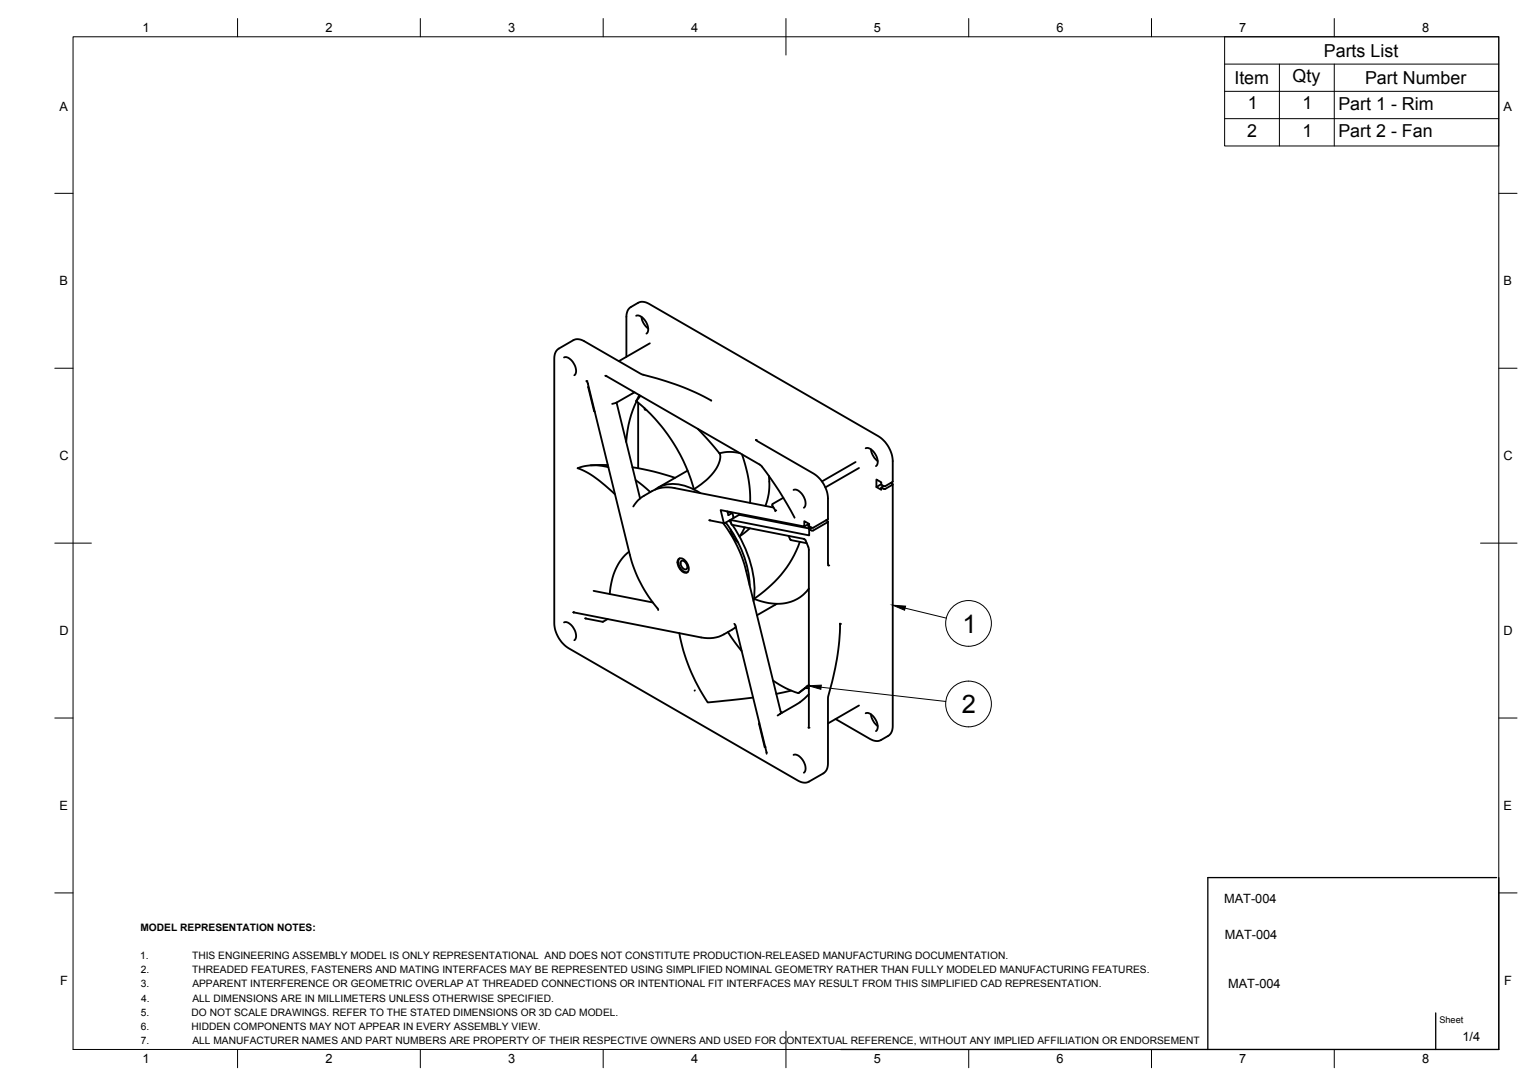
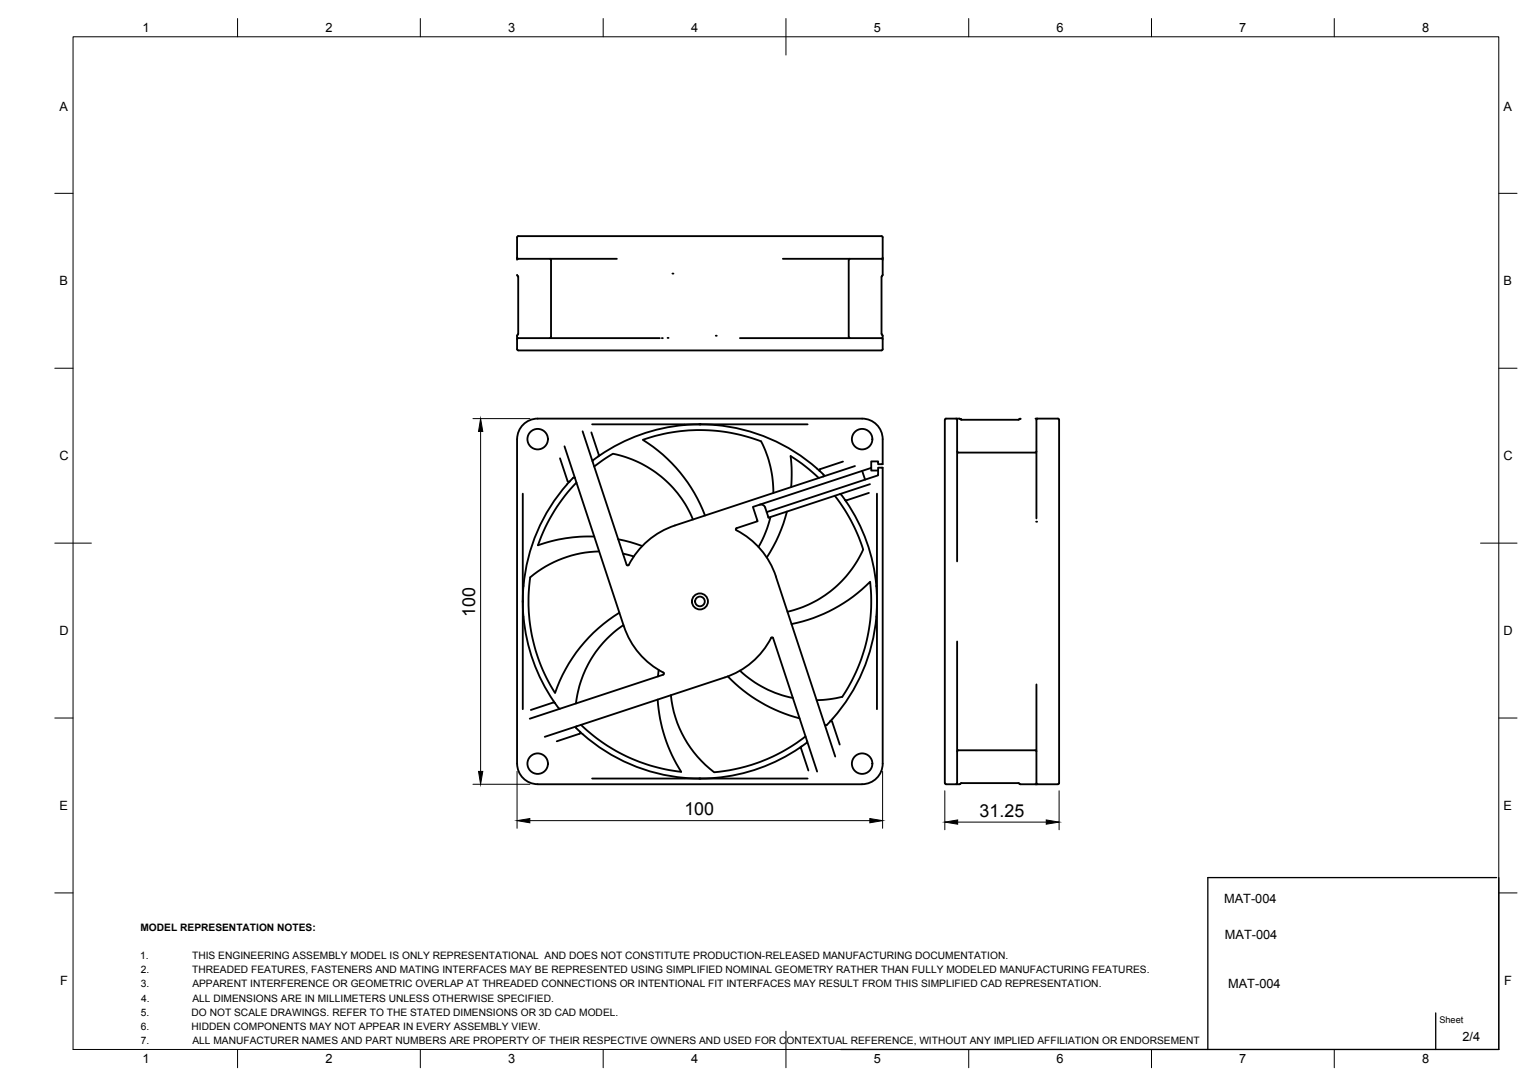
ISO-10303-21;
HEADER;
/* Generated by software containing ST-Developer
 * from STEP Tools, Inc. (www.steptools.com) 
 */

FILE_DESCRIPTION(
/* description */ ('STEP AP214'),
/* implementation_level */ '2;1');

FILE_NAME(
/* name */ 'MAT-004.step',
/* time_stamp */ '2026-11-14T05:34:33-08:00',
/* author */ (''),
/* organization */ (''),
/* preprocessor_version */ 'ST-DEVELOPER v20.2',
/* originating_system */ 'Autodesk Translation Framework v15.17.0.0',
/* authorisation */ '');

FILE_SCHEMA (('AUTOMOTIVE_DESIGN { 1 0 10303 214 3 1 1 }'));
ENDSEC;

DATA;
#10=MECHANICAL_DESIGN_GEOMETRIC_PRESENTATION_REPRESENTATION('',(#23,#24),
#37625);
#11=ITEM_DEFINED_TRANSFORMATION($,$,#11523,#12991);
#12=ITEM_DEFINED_TRANSFORMATION($,$,#12950,#12992);
#13=(
REPRESENTATION_RELATIONSHIP($,$,#37639,#37638)
REPRESENTATION_RELATIONSHIP_WITH_TRANSFORMATION(#11)
SHAPE_REPRESENTATION_RELATIONSHIP()
);
#14=(
REPRESENTATION_RELATIONSHIP($,$,#37640,#37638)
REPRESENTATION_RELATIONSHIP_WITH_TRANSFORMATION(#12)
SHAPE_REPRESENTATION_RELATIONSHIP()
);
#15=CONTEXT_DEPENDENT_SHAPE_REPRESENTATION(#13,#37636);
#16=CONTEXT_DEPENDENT_SHAPE_REPRESENTATION(#14,#37637);
#17=NEXT_ASSEMBLY_USAGE_OCCURRENCE('Part 1 - Rim:1','Part 1 - Rim:1',
'Part 1 - Rim:1',#37642,#37643,'Part 1 - Rim:1');
#18=NEXT_ASSEMBLY_USAGE_OCCURRENCE('Part 2 - Fan:1','Part 2 - Fan:1',
'Part 2 - Fan:1',#37642,#37644,'Part 2 - Fan:1');
#19=SHAPE_REPRESENTATION_RELATIONSHIP('SRR','None',#37639,#21);
#20=SHAPE_REPRESENTATION_RELATIONSHIP('SRR','None',#37640,#22);
#21=ADVANCED_BREP_SHAPE_REPRESENTATION('',(#25),#37623);
#22=ADVANCED_BREP_SHAPE_REPRESENTATION('',(#26),#37624);
#23=STYLED_ITEM('',(#37658),#25);
#24=STYLED_ITEM('',(#37659),#26);
#25=MANIFOLD_SOLID_BREP('Body1',#11497);
#26=MANIFOLD_SOLID_BREP('Body1',#11498);
#27=SPHERICAL_SURFACE('',#12271,0.3125);
#28=SPHERICAL_SURFACE('',#12276,0.3125);
#29=SPHERICAL_SURFACE('',#12302,0.3125);
#30=SPHERICAL_SURFACE('',#12304,0.3125);
#31=SPHERICAL_SURFACE('',#12340,0.3125);
#32=SPHERICAL_SURFACE('',#12342,0.3125);
#33=SPHERICAL_SURFACE('',#12382,0.3125);
#34=SPHERICAL_SURFACE('',#12385,0.3125);
#35=SPHERICAL_SURFACE('',#12394,0.3125);
#36=SPHERICAL_SURFACE('',#12396,0.3125);
#37=SPHERICAL_SURFACE('',#12445,0.3125);
#38=SPHERICAL_SURFACE('',#12447,0.3125);
#39=SPHERICAL_SURFACE('',#12466,0.3125);
#40=SPHERICAL_SURFACE('',#12481,0.3125);
#41=SPHERICAL_SURFACE('',#12525,0.3125);
#42=SPHERICAL_SURFACE('',#12532,0.3125);
#43=SPHERICAL_SURFACE('',#12539,0.3125);
#44=SPHERICAL_SURFACE('',#12541,0.3125);
#45=SPHERICAL_SURFACE('',#12549,0.3125);
#46=SPHERICAL_SURFACE('',#12552,0.3125);
#47=SPHERICAL_SURFACE('',#12570,0.3125);
#48=SPHERICAL_SURFACE('',#12573,0.3125);
#49=SPHERICAL_SURFACE('',#12575,0.3125);
#50=SPHERICAL_SURFACE('',#12580,0.3125);
#51=SPHERICAL_SURFACE('',#12597,0.3125);
#52=SPHERICAL_SURFACE('',#12605,0.3125);
#53=SPHERICAL_SURFACE('',#12628,0.3125);
#54=SPHERICAL_SURFACE('',#12633,0.3125);
#55=SPHERICAL_SURFACE('',#12637,0.3125);
#56=SPHERICAL_SURFACE('',#12640,0.3125);
#57=SPHERICAL_SURFACE('',#12665,0.3125);
#58=SPHERICAL_SURFACE('',#12668,0.3125);
#59=SPHERICAL_SURFACE('',#12674,0.3125);
#60=SPHERICAL_SURFACE('',#12676,0.3125);
#61=SPHERICAL_SURFACE('',#12702,0.3125);
#62=SPHERICAL_SURFACE('',#12704,0.3125);
#63=SPHERICAL_SURFACE('',#12706,0.3125);
#64=SPHERICAL_SURFACE('',#12711,0.3125);
#65=SPHERICAL_SURFACE('',#12733,0.3125);
#66=SPHERICAL_SURFACE('',#12735,0.3125);
#67=SPHERICAL_SURFACE('',#12759,0.3125);
#68=SPHERICAL_SURFACE('',#12761,0.3125);
#69=SPHERICAL_SURFACE('',#12763,0.3125);
#70=SPHERICAL_SURFACE('',#12765,0.3125);
#71=SPHERICAL_SURFACE('',#12779,0.3125);
#72=SPHERICAL_SURFACE('',#12781,0.3125);
#73=SPHERICAL_SURFACE('',#12788,0.3125);
#74=SPHERICAL_SURFACE('',#12790,0.3125);
#75=(
BOUNDED_SURFACE()
B_SPLINE_SURFACE(3,2,((#23896,#23897,#23898),(#23899,#23900,#23901),(#23902,
#23903,#23904),(#23905,#23906,#23907)),.UNSPECIFIED.,.F.,.F.,.F.)
B_SPLINE_SURFACE_WITH_KNOTS((4,4),(3,3),(0.0326127356995135,0.0421285143028756),
(0.,1.),.UNSPECIFIED.)
GEOMETRIC_REPRESENTATION_ITEM()
RATIONAL_B_SPLINE_SURFACE(((1.,0.77336849210705,1.),(1.,0.770480922349025,
1.),(1.,0.767957745429666,1.),(1.,0.765689104422505,1.)))
REPRESENTATION_ITEM('')
SURFACE()
);
#76=(
BOUNDED_SURFACE()
B_SPLINE_SURFACE(3,2,((#23985,#23986,#23987),(#23988,#23989,#23990),(#23991,
#23992,#23993),(#23994,#23995,#23996),(#23997,#23998,#23999),(#24000,#24001,
#24002),(#24003,#24004,#24005),(#24006,#24007,#24008)),.UNSPECIFIED.,.F.,
 .F.,.F.)
B_SPLINE_SURFACE_WITH_KNOTS((4,2,2,4),(3,3),(0.000802853902805026,0.00108948501086238,
0.00137611611891974,0.00194937833503446),(0.,1.),.UNSPECIFIED.)
GEOMETRIC_REPRESENTATION_ITEM()
RATIONAL_B_SPLINE_SURFACE(((1.,0.923879532511285,1.),(1.,0.93126028758527,
1.),(1.,0.931596165488004,1.),(1.,0.918734528780574,1.),(1.,0.905994810924641,
1.),(1.,0.858462949893107,1.),(1.,0.814112175968656,1.),(1.,0.765689104422502,
1.)))
REPRESENTATION_ITEM('')
SURFACE()
);
#77=(
BOUNDED_SURFACE()
B_SPLINE_SURFACE(3,2,((#24068,#24069,#24070),(#24071,#24072,#24073),(#24074,
#24075,#24076),(#24077,#24078,#24079),(#24080,#24081,#24082),(#24083,#24084,
#24085),(#24086,#24087,#24088),(#24089,#24090,#24091)),.UNSPECIFIED.,.F.,
 .F.,.F.)
B_SPLINE_SURFACE_WITH_KNOTS((4,2,2,4),(3,3),(0.000686358375502128,0.000929437613321109,
0.00117251685114009,0.00165867532677805),(0.,1.),.UNSPECIFIED.)
GEOMETRIC_REPRESENTATION_ITEM()
RATIONAL_B_SPLINE_SURFACE(((1.,0.923879532511287,1.),(1.,0.92889985757716,
1.),(1.,0.929018384212628,1.),(1.,0.920008474882563,1.),(1.,0.910871684991149,
1.),(1.,0.87513924549097,1.),(1.,0.84081307837336,1.),(1.,0.802338883728525,
1.)))
REPRESENTATION_ITEM('')
SURFACE()
);
#78=(
BOUNDED_SURFACE()
B_SPLINE_SURFACE(3,2,((#24101,#24102,#24103),(#24104,#24105,#24106),(#24107,
#24108,#24109),(#24110,#24111,#24112),(#24113,#24114,#24115),(#24116,#24117,
#24118),(#24119,#24120,#24121),(#24122,#24123,#24124),(#24125,#24126,#24127),
(#24128,#24129,#24130)),.UNSPECIFIED.,.F.,.F.,.F.)
B_SPLINE_SURFACE_WITH_KNOTS((4,2,2,2,4),(3,3),(0.0314170682308584,0.0383717968941293,
0.0418491612257648,0.0453265255574003,0.0592359828839421),(0.,1.00015514532272),
 .UNSPECIFIED.)
GEOMETRIC_REPRESENTATION_ITEM()
RATIONAL_B_SPLINE_SURFACE(((1.,0.893712741719904,1.00003297994197),(1.,
0.896924595267972,1.00003198333386),(1.,0.900137133821891,1.0000309865132),
(1.,0.904798383538125,1.00002954017102),(1.,0.906325496636901,1.00002906632211),
(1.,0.909290323001115,1.00002814636422),(1.,0.910726187593686,1.00002770082887),
(1.,0.917498844645671,1.00002559933674),(1.,0.921671404518462,1.00002430463045),
(1.,0.923199103012375,1.0000238305999)))
REPRESENTATION_ITEM('')
SURFACE()
);
#79=(
BOUNDED_SURFACE()
B_SPLINE_SURFACE(3,2,((#24156,#24157,#24158),(#24159,#24160,#24161),(#24162,
#24163,#24164),(#24165,#24166,#24167),(#24168,#24169,#24170),(#24171,#24172,
#24173),(#24174,#24175,#24176),(#24177,#24178,#24179),(#24180,#24181,#24182),
(#24183,#24184,#24185)),.UNSPECIFIED.,.F.,.F.,.F.)
B_SPLINE_SURFACE_WITH_KNOTS((4,2,2,2,4),(3,3),(0.0303364035364412,0.0372910338575461,
0.0407683490180985,0.0442456641786509,0.0581549248208605),(0.,1.),
 .UNSPECIFIED.)
GEOMETRIC_REPRESENTATION_ITEM()
RATIONAL_B_SPLINE_SURFACE(((1.,0.893729285230293,1.),(1.,0.8969398694082,
1.),(1.,0.900150686104865,1.),(1.,0.904808789101856,1.),(1.,0.906334760566901,
1.),(1.,0.909297199463308,1.),(1.,0.91073457572851,1.),(1.,0.917512859277436,
1.),(1.,0.921684639637439,1.),(1.,0.923210992612934,1.)))
REPRESENTATION_ITEM('')
SURFACE()
);
#80=(
BOUNDED_SURFACE()
B_SPLINE_SURFACE(3,2,((#24220,#24221,#24222),(#24223,#24224,#24225),(#24226,
#24227,#24228),(#24229,#24230,#24231),(#24232,#24233,#24234),(#24235,#24236,
#24237)),.UNSPECIFIED.,.F.,.F.,.F.)
B_SPLINE_SURFACE_WITH_KNOTS((4,2,4),(3,3),(0.000158496916905221,0.000711650690198974,
0.00126480446349273),(0.,1.),.UNSPECIFIED.)
GEOMETRIC_REPRESENTATION_ITEM()
RATIONAL_B_SPLINE_SURFACE(((1.,0.707106781186549,1.),(1.,0.750150820630032,
1.),(1.,0.789088418359452,1.),(1.,0.861437064777228,1.),(1.,0.895323131481853,
1.),(1.,0.92387953251129,1.)))
REPRESENTATION_ITEM('')
SURFACE()
);
#81=(
BOUNDED_SURFACE()
B_SPLINE_SURFACE(3,2,((#24242,#24243,#24244),(#24245,#24246,#24247),(#24248,
#24249,#24250),(#24251,#24252,#24253),(#24254,#24255,#24256),(#24257,#24258,
#24259),(#24260,#24261,#24262),(#24263,#24264,#24265)),.UNSPECIFIED.,.F.,
 .F.,.F.)
B_SPLINE_SURFACE_WITH_KNOTS((4,2,2,4),(3,3),(0.000174437971377146,0.00101920216019031,
0.00137118723886246,0.00186396634900332),(0.,1.00024356555363),
 .UNSPECIFIED.)
GEOMETRIC_REPRESENTATION_ITEM()
RATIONAL_B_SPLINE_SURFACE(((1.,0.539098756316927,1.00022451933317),(1.,
0.633858154865208,1.00017835908243),(1.,0.717178341053912,1.00013777122788),
(1.,0.814824555144991,1.00009020471949),(1.,0.841538081526998,1.0000771917298),
(1.,0.898531920368047,1.00004942825798),(1.,0.925786672706503,1.0000361516203),
(1.,0.937456960617578,1.00003046666003)))
REPRESENTATION_ITEM('')
SURFACE()
);
#82=(
BOUNDED_SURFACE()
B_SPLINE_SURFACE(3,2,((#24441,#24442,#24443),(#24444,#24445,#24446),(#24447,
#24448,#24449),(#24450,#24451,#24452),(#24453,#24454,#24455),(#24456,#24457,
#24458)),.UNSPECIFIED.,.F.,.F.,.F.)
B_SPLINE_SURFACE_WITH_KNOTS((4,2,4),(3,3),(0.000796035510927852,0.00146280219164561,
0.00212956887236337),(0.,1.00047905246342),.UNSPECIFIED.)
GEOMETRIC_REPRESENTATION_ITEM()
RATIONAL_B_SPLINE_SURFACE(((1.,0.680382792871542,1.00030622682085),(1.,
0.734649451169007,1.00025423366818),(1.,0.782184849656497,1.00020868976868),
(1.,0.8686687938328,1.00012582907568),(1.,0.90836300942771,1.00008779785215),
(1.,0.940539343963641,1.0000569695475)))
REPRESENTATION_ITEM('')
SURFACE()
);
#83=(
BOUNDED_SURFACE()
B_SPLINE_SURFACE(3,2,((#24462,#24463,#24464),(#24465,#24466,#24467),(#24468,
#24469,#24470),(#24471,#24472,#24473)),.UNSPECIFIED.,.F.,.F.,.F.)
B_SPLINE_SURFACE_WITH_KNOTS((4,4),(3,3),(0.0647248597593566,0.0667277597197425),
(0.,1.),.UNSPECIFIED.)
GEOMETRIC_REPRESENTATION_ITEM()
RATIONAL_B_SPLINE_SURFACE(((1.,0.77254330703138,1.),(1.,0.773053168552101,
1.),(1.,0.773574707201174,1.),(1.,0.774108727913442,1.)))
REPRESENTATION_ITEM('')
SURFACE()
);
#84=(
BOUNDED_SURFACE()
B_SPLINE_SURFACE(3,2,((#24557,#24558,#24559),(#24560,#24561,#24562),(#24563,
#24564,#24565),(#24566,#24567,#24568)),.UNSPECIFIED.,.F.,.F.,.F.)
B_SPLINE_SURFACE_WITH_KNOTS((4,4),(3,3),(0.0554293707990946,0.067219986976584),
(0.,1.00093204202966),.UNSPECIFIED.)
GEOMETRIC_REPRESENTATION_ITEM()
RATIONAL_B_SPLINE_SURFACE(((1.,0.586730971631016,1.00077036820799),(1.,
0.580458668850621,1.00078206030762),(1.,0.573277155045983,1.00079544725303),
(1.,0.564689221730742,1.00081145588262)))
REPRESENTATION_ITEM('')
SURFACE()
);
#85=(
BOUNDED_SURFACE()
B_SPLINE_SURFACE(3,2,((#24588,#24589,#24590),(#24591,#24592,#24593),(#24594,
#24595,#24596),(#24597,#24598,#24599),(#24600,#24601,#24602),(#24603,#24604,
#24605),(#24606,#24607,#24608),(#24609,#24610,#24611),(#24612,#24613,#24614),
(#24615,#24616,#24617)),.UNSPECIFIED.,.F.,.F.,.F.)
B_SPLINE_SURFACE_WITH_KNOTS((4,2,2,2,4),(3,3),(0.000140109886117696,0.000666559814939625,
0.00108521714444999,0.00150387447396035,0.00203032440278269),(-0.000871030384560204,
1.),.UNSPECIFIED.)
GEOMETRIC_REPRESENTATION_ITEM()
RATIONAL_B_SPLINE_SURFACE(((1.00092572483597,0.468603591574399,1.),(1.00081905401985,
0.5298361375373,1.),(1.00071568618447,0.589172664263207,1.),(1.00054995854446,
0.684305763488853,1.),(1.00048250324099,0.723027319401472,1.),(1.00035800741942,
0.794492002940391,1.),(1.00030258788071,0.826304635251683,1.),(1.00018948908564,
0.891227051893231,1.),(1.00013836850255,0.920571942721851,1.),(1.00011502671673,
0.933970893113149,1.)))
REPRESENTATION_ITEM('')
SURFACE()
);
#86=(
BOUNDED_SURFACE()
B_SPLINE_SURFACE(3,2,((#24621,#24622,#24623),(#24624,#24625,#24626),(#24627,
#24628,#24629),(#24630,#24631,#24632)),.UNSPECIFIED.,.F.,.F.,.F.)
B_SPLINE_SURFACE_WITH_KNOTS((4,4),(3,3),(0.0554293708282248,0.0672199869474538),
(0.,1.00093204200053),.UNSPECIFIED.)
GEOMETRIC_REPRESENTATION_ITEM()
RATIONAL_B_SPLINE_SURFACE(((1.,0.586730971596549,1.00077036818398),(1.,
0.580458668842862,1.00078206028319),(1.,0.573277155072649,1.00079544722812),
(1.,0.564689221807079,1.00081145585712)))
REPRESENTATION_ITEM('')
SURFACE()
);
#87=(
BOUNDED_SURFACE()
B_SPLINE_SURFACE(3,2,((#24651,#24652,#24653),(#24654,#24655,#24656),(#24657,
#24658,#24659),(#24660,#24661,#24662),(#24663,#24664,#24665),(#24666,#24667,
#24668)),.UNSPECIFIED.,.F.,.F.,.F.)
B_SPLINE_SURFACE_WITH_KNOTS((4,2,4),(3,3),(0.000315513320331966,0.000961720209151386,
0.00160792712680523),(-0.00216992936483643,1.),.UNSPECIFIED.)
GEOMETRIC_REPRESENTATION_ITEM()
RATIONAL_B_SPLINE_SURFACE(((1.00140856318051,0.675435706956244,1.),(1.00113480498433,
0.73851568564515,1.),(1.00088601384726,0.795842698473231,1.),(1.00048533380217,
0.888168294775817,1.),(1.00032603746989,0.924873713592471,1.),(1.00031273915803,
0.927937940493073,1.)))
REPRESENTATION_ITEM('')
SURFACE()
);
#88=(
BOUNDED_SURFACE()
B_SPLINE_SURFACE(3,2,((#24670,#24671,#24672),(#24673,#24674,#24675),(#24676,
#24677,#24678),(#24679,#24680,#24681),(#24682,#24683,#24684),(#24685,#24686,
#24687)),.UNSPECIFIED.,.F.,.F.,.F.)
B_SPLINE_SURFACE_WITH_KNOTS((4,2,4),(3,3),(0.000402895580047919,0.000905401753400751,
0.00140790792675358),(0.,1.),.UNSPECIFIED.)
GEOMETRIC_REPRESENTATION_ITEM()
RATIONAL_B_SPLINE_SURFACE(((1.,0.813540597401216,1.),(1.,0.813784197152837,
1.),(1.,0.801974141898952,1.),(1.,0.763153562323537,1.),(1.,0.735816595983232,
1.),(1.,0.707106781186551,1.)))
REPRESENTATION_ITEM('')
SURFACE()
);
#89=(
BOUNDED_SURFACE()
B_SPLINE_SURFACE(3,2,((#24694,#24695,#24696),(#24697,#24698,#24699),(#24700,
#24701,#24702),(#24703,#24704,#24705),(#24706,#24707,#24708),(#24709,#24710,
#24711)),.UNSPECIFIED.,.F.,.F.,.F.)
B_SPLINE_SURFACE_WITH_KNOTS((4,2,4),(3,3),(0.000800222346544408,0.00146699934948425,
0.00213377635242409),(0.,1.0004790524742),.UNSPECIFIED.)
GEOMETRIC_REPRESENTATION_ITEM()
RATIONAL_B_SPLINE_SURFACE(((1.,0.680382792868073,1.00030622682775),(1.,
0.73464945116617,1.0002542336739),(1.,0.782184849654142,1.00020868977338),
(1.,0.868668793831392,1.00012582907851),(1.,0.908363009426711,1.00008779785413),
(1.,0.940539343963006,1.00005696954878)))
REPRESENTATION_ITEM('')
SURFACE()
);
#90=(
BOUNDED_SURFACE()
B_SPLINE_SURFACE(3,2,((#24741,#24742,#24743),(#24744,#24745,#24746),(#24747,
#24748,#24749),(#24750,#24751,#24752),(#24753,#24754,#24755),(#24756,#24757,
#24758),(#24759,#24760,#24761),(#24762,#24763,#24764),(#24765,#24766,#24767),
(#24768,#24769,#24770)),.UNSPECIFIED.,.F.,.F.,.F.)
B_SPLINE_SURFACE_WITH_KNOTS((4,2,2,2,4),(3,3),(0.0314170682308576,0.0383717968941285,
0.041849161225764,0.0453265255573995,0.0592359828839414),(0.,1.00015514533033),
 .UNSPECIFIED.)
GEOMETRIC_REPRESENTATION_ITEM()
RATIONAL_B_SPLINE_SURFACE(((1.,0.893712741719095,1.00003297994359),(1.,
0.896924595266501,1.00003198333543),(1.,0.900137133822039,1.00003098651472),
(1.,0.904798383536946,1.00002954017247),(1.,0.906325496636188,1.00002906632354),
(1.,0.909290323000425,1.0000281463656),(1.,0.910726187593075,1.00002770083023),
(1.,0.917498844644786,1.000025599338),(1.,0.921671404518056,1.00002430463164),
(1.,0.923199103011791,1.00002383060107)))
REPRESENTATION_ITEM('')
SURFACE()
);
#91=(
BOUNDED_SURFACE()
B_SPLINE_SURFACE(3,2,((#24796,#24797,#24798),(#24799,#24800,#24801),(#24802,
#24803,#24804),(#24805,#24806,#24807),(#24808,#24809,#24810),(#24811,#24812,
#24813),(#24814,#24815,#24816),(#24817,#24818,#24819),(#24820,#24821,#24822),
(#24823,#24824,#24825)),.UNSPECIFIED.,.F.,.F.,.F.)
B_SPLINE_SURFACE_WITH_KNOTS((4,2,2,2,4),(3,3),(0.0303364035364412,0.0372910338575461,
0.0407683490180985,0.0442456641786509,0.0581549248208606),(0.,1.),
 .UNSPECIFIED.)
GEOMETRIC_REPRESENTATION_ITEM()
RATIONAL_B_SPLINE_SURFACE(((1.,0.893729285230296,1.),(1.,0.89693986940752,
1.),(1.,0.900150686105771,1.),(1.,0.904808789101402,1.),(1.,0.906334760567093,
1.),(1.,0.909297199463109,1.),(1.,0.91073457572825,1.),(1.,0.917512859278478,
1.),(1.,0.921684639636655,1.),(1.,0.923210992612934,1.)))
REPRESENTATION_ITEM('')
SURFACE()
);
#92=(
BOUNDED_SURFACE()
B_SPLINE_SURFACE(3,2,((#24827,#24828,#24829),(#24830,#24831,#24832),(#24833,
#24834,#24835),(#24836,#24837,#24838),(#24839,#24840,#24841),(#24842,#24843,
#24844),(#24845,#24846,#24847),(#24848,#24849,#24850),(#24851,#24852,#24853),
(#24854,#24855,#24856)),.UNSPECIFIED.,.F.,.F.,.F.)
B_SPLINE_SURFACE_WITH_KNOTS((4,2,2,2,4),(3,3),(0.000140109886348097,0.00066655981493961,
0.00108521714444997,0.00150387447396033,0.00203032440255225),(-0.000871030383072034,
1.),.UNSPECIFIED.)
GEOMETRIC_REPRESENTATION_ITEM()
RATIONAL_B_SPLINE_SURFACE(((1.00092572483425,0.468603591655602,1.),(1.00081905401836,
0.529836137589938,1.),(1.00071568618321,0.589172664287011,1.),(1.00054995854352,
0.684305763489321,1.),(1.00048250324016,0.723027319402148,1.),(1.00035800741881,
0.794492002940432,1.),(1.00030258788019,0.826304635252028,1.),(1.00018948908534,
0.891227051877456,1.),(1.00013836850236,0.920571942696442,1.),(1.00011502671656,
0.933970893095549,1.)))
REPRESENTATION_ITEM('')
SURFACE()
);
#93=(
BOUNDED_SURFACE()
B_SPLINE_SURFACE(3,2,((#24858,#24859,#24860),(#24861,#24862,#24863),(#24864,
#24865,#24866),(#24867,#24868,#24869),(#24870,#24871,#24872),(#24873,#24874,
#24875),(#24876,#24877,#24878),(#24879,#24880,#24881)),.UNSPECIFIED.,.F.,
 .F.,.F.)
B_SPLINE_SURFACE_WITH_KNOTS((4,2,2,4),(3,3),(0.000174437971377159,0.00101920216019031,
0.00137118723886246,0.00186396634900331),(0.,1.00024356555507),
 .UNSPECIFIED.)
GEOMETRIC_REPRESENTATION_ITEM()
RATIONAL_B_SPLINE_SURFACE(((1.,0.53909875631573,1.0002245193345),(1.,0.633858154865746,
1.00017835908349),(1.,0.717178341052667,1.0001377712287),(1.,0.814824555145073,
1.00009020472002),(1.,0.841538081527084,1.00007719173026),(1.,0.89853192036746,
1.00004942825828),(1.,0.92578667270721,1.00003615162051),(1.,0.937456960616711,
1.00003046666021)))
REPRESENTATION_ITEM('')
SURFACE()
);
#94=(
BOUNDED_SURFACE()
B_SPLINE_SURFACE(3,2,((#24935,#24936,#24937),(#24938,#24939,#24940),(#24941,
#24942,#24943),(#24944,#24945,#24946),(#24947,#24948,#24949),(#24950,#24951,
#24952),(#24953,#24954,#24955),(#24956,#24957,#24958),(#24959,#24960,#24961),
(#24962,#24963,#24964)),.UNSPECIFIED.,.F.,.F.,.F.)
B_SPLINE_SURFACE_WITH_KNOTS((4,2,2,2,4),(3,3),(0.000329019594184255,0.000643209132708098,
0.000817758876492274,0.00116685836406063,0.00200469706399122),(-0.00396994925378904,
1.),.UNSPECIFIED.)
GEOMETRIC_REPRESENTATION_ITEM()
RATIONAL_B_SPLINE_SURFACE(((1.00073501708023,0.907427396013615,1.),(1.000615151231,
0.922524043548762,1.),(1.00054588724346,0.931247579180259,1.),(1.00054531256499,
0.931319957746567,1.),(1.00056655237271,0.928644884796654,1.),(1.00068340691792,
0.913927499543016,1.),(1.00082907221214,0.895581510097415,1.),(1.00142178903535,
0.820931081928685,1.),(1.00200380422997,0.747628483153123,1.),(1.00265356605592,
0.665793453986162,1.)))
REPRESENTATION_ITEM('')
SURFACE()
);
#95=(
BOUNDED_SURFACE()
B_SPLINE_SURFACE(3,2,((#25082,#25083,#25084),(#25085,#25086,#25087),(#25088,
#25089,#25090),(#25091,#25092,#25093)),.UNSPECIFIED.,.F.,.F.,.F.)
B_SPLINE_SURFACE_WITH_KNOTS((4,4),(3,3),(0.0650014074844314,0.0670796431839287),
(0.,1.),.UNSPECIFIED.)
GEOMETRIC_REPRESENTATION_ITEM()
RATIONAL_B_SPLINE_SURFACE(((1.,0.601781042690493,1.),(1.,0.600836260738882,
1.),(1.,0.599866989417514,1.),(1.,0.598871405423905,1.)))
REPRESENTATION_ITEM('')
SURFACE()
);
#96=(
BOUNDED_SURFACE()
B_SPLINE_SURFACE(3,2,((#25157,#25158,#25159),(#25160,#25161,#25162),(#25163,
#25164,#25165),(#25166,#25167,#25168),(#25169,#25170,#25171),(#25172,#25173,
#25174)),.UNSPECIFIED.,.F.,.F.,.F.)
B_SPLINE_SURFACE_WITH_KNOTS((4,2,4),(3,3),(0.000158380329178595,0.000711237088130122,
0.00126409384708165),(0.,1.),.UNSPECIFIED.)
GEOMETRIC_REPRESENTATION_ITEM()
RATIONAL_B_SPLINE_SURFACE(((1.,0.707106781186546,1.),(1.,0.750152861189045,
1.),(1.,0.789073569306456,1.),(1.,0.861356580931207,1.),(1.,0.895247679276223,
1.),(1.,0.923879532511291,1.)))
REPRESENTATION_ITEM('')
SURFACE()
);
#97=(
BOUNDED_SURFACE()
B_SPLINE_SURFACE(3,2,((#25243,#25244,#25245),(#25246,#25247,#25248),(#25249,
#25250,#25251),(#25252,#25253,#25254)),.UNSPECIFIED.,.F.,.F.,.F.)
B_SPLINE_SURFACE_WITH_KNOTS((4,4),(3,3),(0.0650014074844314,0.0670796431839287),
(0.,1.),.UNSPECIFIED.)
GEOMETRIC_REPRESENTATION_ITEM()
RATIONAL_B_SPLINE_SURFACE(((1.,0.601781042690495,1.),(1.,0.600836260738928,
1.),(1.,0.599866989417502,1.),(1.,0.598871405423905,1.)))
REPRESENTATION_ITEM('')
SURFACE()
);
#98=(
BOUNDED_SURFACE()
B_SPLINE_SURFACE(3,2,((#25256,#25257,#25258),(#25259,#25260,#25261),(#25262,
#25263,#25264),(#25265,#25266,#25267),(#25268,#25269,#25270),(#25271,#25272,
#25273)),.UNSPECIFIED.,.F.,.F.,.F.)
B_SPLINE_SURFACE_WITH_KNOTS((4,2,4),(3,3),(0.000402651921819617,0.000906087614430024,
0.00140952330704043),(0.,1.),.UNSPECIFIED.)
GEOMETRIC_REPRESENTATION_ITEM()
RATIONAL_B_SPLINE_SURFACE(((1.,0.813540597401216,1.),(1.,0.813739345537075,
1.),(1.,0.802648961762859,1.),(1.,0.764608789261971,1.),(1.,0.737258306119054,
1.),(1.,0.707106781186554,1.)))
REPRESENTATION_ITEM('')
SURFACE()
);
#99=(
BOUNDED_SURFACE()
B_SPLINE_SURFACE(3,2,((#25312,#25313,#25314),(#25315,#25316,#25317),(#25318,
#25319,#25320),(#25321,#25322,#25323),(#25324,#25325,#25326),(#25327,#25328,
#25329),(#25330,#25331,#25332),(#25333,#25334,#25335),(#25336,#25337,#25338),
(#25339,#25340,#25341)),.UNSPECIFIED.,.F.,.F.,.F.)
B_SPLINE_SURFACE_WITH_KNOTS((4,2,2,2,4),(3,3),(0.000758206618216268,0.00101809884720581,
0.00127799107619535,0.00153788330518489,0.00179777553417443),(0.,1.),
 .UNSPECIFIED.)
GEOMETRIC_REPRESENTATION_ITEM()
RATIONAL_B_SPLINE_SURFACE(((1.,0.707106781186548,1.),(1.,0.686991483272875,
1.),(1.,0.666460369298716,1.),(1.,0.62447089523074,1.),(1.,0.604201592515098,
1.),(1.,0.566291012805826,1.),(1.,0.549844363605541,1.),(1.,0.525862225699567,
1.),(1.,0.51912808872997,1.),(1.,0.51911513123826,1.)))
REPRESENTATION_ITEM('')
SURFACE()
);
#100=(
BOUNDED_SURFACE()
B_SPLINE_SURFACE(3,2,((#25342,#25343,#25344),(#25345,#25346,#25347),(#25348,
#25349,#25350),(#25351,#25352,#25353),(#25354,#25355,#25356),(#25357,#25358,
#25359),(#25360,#25361,#25362),(#25363,#25364,#25365),(#25366,#25367,#25368),
(#25369,#25370,#25371)),.UNSPECIFIED.,.F.,.F.,.F.)
B_SPLINE_SURFACE_WITH_KNOTS((4,2,2,2,4),(3,3),(0.000329019594184018,0.000643209132708091,
0.000817758876492263,0.00116685836406061,0.00200469706399384),(-0.00396994923486767,
1.),.UNSPECIFIED.)
GEOMETRIC_REPRESENTATION_ITEM()
RATIONAL_B_SPLINE_SURFACE(((1.00073501707671,0.907427396016355,1.),(1.00061515122806,
0.922524043549619,1.),(1.00054588724085,0.931247579181756,1.),(1.00054531256238,
0.93131995774775,1.),(1.00056655237,0.928644884798117,1.),(1.00068340691465,
0.913927499544403,1.),(1.00082907220817,0.895581510099604,1.),(1.00142178902855,
0.820931081931361,1.),(1.00200380422038,0.74762848315811,1.),(1.00265356604323,
0.665793453991339,1.)))
REPRESENTATION_ITEM('')
SURFACE()
);
#101=(
BOUNDED_SURFACE()
B_SPLINE_SURFACE(3,2,((#25375,#25376,#25377),(#25378,#25379,#25380),(#25381,
#25382,#25383),(#25384,#25385,#25386)),.UNSPECIFIED.,.F.,.F.,.F.)
B_SPLINE_SURFACE_WITH_KNOTS((4,4),(3,3),(0.0326127356995135,0.0421285143028756),
(0.,1.),.UNSPECIFIED.)
GEOMETRIC_REPRESENTATION_ITEM()
RATIONAL_B_SPLINE_SURFACE(((1.,0.773368492107047,1.),(1.,0.770480922349026,
1.),(1.,0.767957745429661,1.),(1.,0.765689104422504,1.)))
REPRESENTATION_ITEM('')
SURFACE()
);
#102=(
BOUNDED_SURFACE()
B_SPLINE_SURFACE(3,2,((#25464,#25465,#25466),(#25467,#25468,#25469),(#25470,
#25471,#25472),(#25473,#25474,#25475)),.UNSPECIFIED.,.F.,.F.,.F.)
B_SPLINE_SURFACE_WITH_KNOTS((4,4),(3,3),(0.0313106092150184,0.0408266168605713),
(0.,1.),.UNSPECIFIED.)
GEOMETRIC_REPRESENTATION_ITEM()
RATIONAL_B_SPLINE_SURFACE(((1.,0.773368492015519,1.),(1.,0.77048091928462,
1.),(1.,0.7679577451536,1.),(1.,0.765689104422504,1.)))
REPRESENTATION_ITEM('')
SURFACE()
);
#103=(
BOUNDED_SURFACE()
B_SPLINE_SURFACE(3,2,((#25567,#25568,#25569),(#25570,#25571,#25572),(#25573,
#25574,#25575),(#25576,#25577,#25578),(#25579,#25580,#25581),(#25582,#25583,
#25584)),.UNSPECIFIED.,.F.,.F.,.F.)
B_SPLINE_SURFACE_WITH_KNOTS((4,2,4),(3,3),(0.000315513320334842,0.000961720209151388,
0.00160792712680523),(-0.00216992936498931,1.),.UNSPECIFIED.)
GEOMETRIC_REPRESENTATION_ITEM()
RATIONAL_B_SPLINE_SURFACE(((1.0014085631806,0.675435706956732,1.),(1.0011348049844,
0.73851568564622,1.),(1.00088601384732,0.795842698472947,1.),(1.0004853338022,
0.888168294776257,1.),(1.00032603746992,0.924873713591867,1.),(1.00031273915805,
0.92793794049336,1.)))
REPRESENTATION_ITEM('')
SURFACE()
);
#104=(
BOUNDED_SURFACE()
B_SPLINE_SURFACE(3,2,((#25632,#25633,#25634),(#25635,#25636,#25637),(#25638,
#25639,#25640),(#25641,#25642,#25643),(#25644,#25645,#25646),(#25647,#25648,
#25649),(#25650,#25651,#25652),(#25653,#25654,#25655)),.UNSPECIFIED.,.F.,
 .F.,.F.)
B_SPLINE_SURFACE_WITH_KNOTS((4,2,2,4),(3,3),(0.000802853902805014,0.00108948501086237,
0.00137611611891973,0.00194937833503444),(0.,1.),.UNSPECIFIED.)
GEOMETRIC_REPRESENTATION_ITEM()
RATIONAL_B_SPLINE_SURFACE(((1.,0.923879532511287,1.),(1.,0.931260287585301,
1.),(1.,0.931596165487967,1.),(1.,0.918734528780613,1.),(1.,0.90599481092429,
1.),(1.,0.858462949893807,1.),(1.,0.81411217596811,1.),(1.,0.765689104422511,
1.)))
REPRESENTATION_ITEM('')
SURFACE()
);
#105=(
BOUNDED_SURFACE()
B_SPLINE_SURFACE(3,2,((#25715,#25716,#25717),(#25718,#25719,#25720),(#25721,
#25722,#25723),(#25724,#25725,#25726),(#25727,#25728,#25729),(#25730,#25731,
#25732),(#25733,#25734,#25735),(#25736,#25737,#25738)),.UNSPECIFIED.,.F.,
 .F.,.F.)
B_SPLINE_SURFACE_WITH_KNOTS((4,2,2,4),(3,3),(0.000686358375502152,0.000929437613321132,
0.00117251685114011,0.00165867532677807),(0.,1.),.UNSPECIFIED.)
GEOMETRIC_REPRESENTATION_ITEM()
RATIONAL_B_SPLINE_SURFACE(((1.,0.923879532511286,1.),(1.,0.928899857577065,
1.),(1.,0.929018384212755,1.),(1.,0.920008474882436,1.),(1.,0.910871684991113,
1.),(1.,0.875139245491043,1.),(1.,0.840813078373301,1.),(1.,0.802338883728528,
1.)))
REPRESENTATION_ITEM('')
SURFACE()
);
#106=(
BOUNDED_SURFACE()
B_SPLINE_SURFACE(3,2,((#25739,#25740,#25741),(#25742,#25743,#25744),(#25745,
#25746,#25747),(#25748,#25749,#25750),(#25751,#25752,#25753),(#25754,#25755,
#25756),(#25757,#25758,#25759),(#25760,#25761,#25762)),.UNSPECIFIED.,.F.,
 .F.,.F.)
B_SPLINE_SURFACE_WITH_KNOTS((4,2,2,4),(3,3),(0.000802853902805007,0.00108948501086237,
0.00137611611891972,0.00194937833503444),(0.,1.),.UNSPECIFIED.)
GEOMETRIC_REPRESENTATION_ITEM()
RATIONAL_B_SPLINE_SURFACE(((1.,0.923879532511287,1.),(1.,0.931260287585252,
1.),(1.,0.931596165488031,1.),(1.,0.918734528780548,1.),(1.,0.905994810924283,
1.),(1.,0.858462949893815,1.),(1.,0.814112175968112,1.),(1.,0.765689104422505,
1.)))
REPRESENTATION_ITEM('')
SURFACE()
);
#107=(
BOUNDED_SURFACE()
B_SPLINE_SURFACE(3,2,((#25822,#25823,#25824),(#25825,#25826,#25827),(#25828,
#25829,#25830),(#25831,#25832,#25833),(#25834,#25835,#25836),(#25837,#25838,
#25839),(#25840,#25841,#25842),(#25843,#25844,#25845)),.UNSPECIFIED.,.F.,
 .F.,.F.)
B_SPLINE_SURFACE_WITH_KNOTS((4,2,2,4),(3,3),(0.000686358375502721,0.000929437613321688,
0.00117251685114066,0.00165867532677859),(0.,1.),.UNSPECIFIED.)
GEOMETRIC_REPRESENTATION_ITEM()
RATIONAL_B_SPLINE_SURFACE(((1.,0.923879532511325,1.),(1.,0.928899857576951,
1.),(1.,0.929018384212867,1.),(1.,0.920008474882321,1.),(1.,0.910871684991292,
1.),(1.,0.875139245490692,1.),(1.,0.840813078373569,1.),(1.,0.802338883728525,
1.)))
REPRESENTATION_ITEM('')
SURFACE()
);
#108=(
BOUNDED_SURFACE()
B_SPLINE_SURFACE(3,2,((#25905,#25906,#25907),(#25908,#25909,#25910),(#25911,
#25912,#25913),(#25914,#25915,#25916),(#25917,#25918,#25919),(#25920,#25921,
#25922),(#25923,#25924,#25925),(#25926,#25927,#25928),(#25929,#25930,#25931),
(#25932,#25933,#25934)),.UNSPECIFIED.,.F.,.F.,.F.)
B_SPLINE_SURFACE_WITH_KNOTS((4,2,2,2,4),(3,3),(0.00051215679899462,0.000771582496110788,
0.00103100819322696,0.00129043389034312,0.00154985958745929),(0.,1.),
 .UNSPECIFIED.)
GEOMETRIC_REPRESENTATION_ITEM()
RATIONAL_B_SPLINE_SURFACE(((1.,0.707106781186548,1.),(1.,0.687254414974402,
1.),(1.,0.666880865311976,1.),(1.,0.625068437161317,1.),(1.,0.604779625068006,
1.),(1.,0.566741718306699,1.),(1.,0.550156755482303,1.),(1.,0.52595679230038,
1.),(1.,0.519123228378,1.),(1.,0.51911513123826,1.)))
REPRESENTATION_ITEM('')
SURFACE()
);
#109=(
BOUNDED_SURFACE()
B_SPLINE_SURFACE(3,2,((#25985,#25986,#25987),(#25988,#25989,#25990),(#25991,
#25992,#25993),(#25994,#25995,#25996)),.UNSPECIFIED.,.F.,.F.,.F.)
B_SPLINE_SURFACE_WITH_KNOTS((4,4),(3,3),(0.0647248597593566,0.0667277597197425),
(0.,1.),.UNSPECIFIED.)
GEOMETRIC_REPRESENTATION_ITEM()
RATIONAL_B_SPLINE_SURFACE(((1.,0.772543307031375,1.),(1.,0.773053168552095,
1.),(1.,0.773574707201188,1.),(1.,0.774108727913435,1.)))
REPRESENTATION_ITEM('')
SURFACE()
);
#110=(
BOUNDED_SURFACE()
B_SPLINE_SURFACE(3,2,((#26003,#26004,#26005),(#26006,#26007,#26008),(#26009,
#26010,#26011),(#26012,#26013,#26014),(#26015,#26016,#26017),(#26018,#26019,
#26020),(#26021,#26022,#26023),(#26024,#26025,#26026),(#26027,#26028,#26029),
(#26030,#26031,#26032)),.UNSPECIFIED.,.F.,.F.,.F.)
B_SPLINE_SURFACE_WITH_KNOTS((4,2,2,2,4),(3,3),(0.031417068230858,0.0383717968941289,
0.0418491612257644,0.0453265255573999,0.0592359828839417),(0.,1.00015514531871),
 .UNSPECIFIED.)
GEOMETRIC_REPRESENTATION_ITEM()
RATIONAL_B_SPLINE_SURFACE(((1.,0.893712741720332,1.00003297994112),(1.,
0.896924595268385,1.00003198333304),(1.,0.900137133822292,1.0000309865124),
(1.,0.904798383538507,1.00002954017025),(1.,0.906325496637147,1.00002906632136),
(1.,0.90929032300161,1.0000281463635),(1.,0.910726187594044,1.00002770082816),
(1.,0.917498844646002,1.00002559933608),(1.,0.921671404518776,1.00002430462982),
(1.,0.923199103012683,1.00002383059928)))
REPRESENTATION_ITEM('')
SURFACE()
);
#111=(
BOUNDED_SURFACE()
B_SPLINE_SURFACE(3,2,((#26058,#26059,#26060),(#26061,#26062,#26063),(#26064,
#26065,#26066),(#26067,#26068,#26069),(#26070,#26071,#26072),(#26073,#26074,
#26075),(#26076,#26077,#26078),(#26079,#26080,#26081),(#26082,#26083,#26084),
(#26085,#26086,#26087)),.UNSPECIFIED.,.F.,.F.,.F.)
B_SPLINE_SURFACE_WITH_KNOTS((4,2,2,2,4),(3,3),(0.03033640353644,0.0372910338575448,
0.0407683490180972,0.0442456641786496,0.0581549248208593),(0.,1.),
 .UNSPECIFIED.)
GEOMETRIC_REPRESENTATION_ITEM()
RATIONAL_B_SPLINE_SURFACE(((1.,0.893729285230292,1.),(1.,0.896939869408588,
1.),(1.,0.900150686104346,1.),(1.,0.904808789102115,1.),(1.,0.906334760566706,
1.),(1.,0.909297199463503,1.),(1.,0.91073457572825,1.),(1.,0.917512859278477,
1.),(1.,0.921684639636657,1.),(1.,0.923210992612934,1.)))
REPRESENTATION_ITEM('')
SURFACE()
);
#112=(
BOUNDED_SURFACE()
B_SPLINE_SURFACE(3,2,((#26122,#26123,#26124),(#26125,#26126,#26127),(#26128,
#26129,#26130),(#26131,#26132,#26133),(#26134,#26135,#26136),(#26137,#26138,
#26139)),.UNSPECIFIED.,.F.,.F.,.F.)
B_SPLINE_SURFACE_WITH_KNOTS((4,2,4),(3,3),(0.000158484458110993,0.000711605405373087,
0.00126472635263518),(0.,1.),.UNSPECIFIED.)
GEOMETRIC_REPRESENTATION_ITEM()
RATIONAL_B_SPLINE_SURFACE(((1.,0.707106781186548,1.),(1.,0.750150943531002,
1.),(1.,0.789086629669813,1.),(1.,0.861428008632711,1.),(1.,0.895315681224068,
1.),(1.,0.923879532511287,1.)))
REPRESENTATION_ITEM('')
SURFACE()
);
#113=(
BOUNDED_SURFACE()
B_SPLINE_SURFACE(3,2,((#26146,#26147,#26148),(#26149,#26150,#26151),(#26152,
#26153,#26154),(#26155,#26156,#26157),(#26158,#26159,#26160),(#26161,#26162,
#26163),(#26164,#26165,#26166),(#26167,#26168,#26169),(#26170,#26171,#26172),
(#26173,#26174,#26175)),.UNSPECIFIED.,.F.,.F.,.F.)
B_SPLINE_SURFACE_WITH_KNOTS((4,2,2,2,4),(3,3),(0.000758206618216247,0.00101809884720579,
0.00127799107619532,0.00153788330518486,0.0017977755341744),(0.,1.),
 .UNSPECIFIED.)
GEOMETRIC_REPRESENTATION_ITEM()
RATIONAL_B_SPLINE_SURFACE(((1.,0.707106781186548,1.),(1.,0.686991483272796,
1.),(1.,0.666460369298813,1.),(1.,0.624470895230632,1.),(1.,0.604201592515102,
1.),(1.,0.56629101280583,1.),(1.,0.549844363605635,1.),(1.,0.525862225699477,
1.),(1.,0.519128088730044,1.),(1.,0.51911513123826,1.)))
REPRESENTATION_ITEM('')
SURFACE()
);
#114=(
BOUNDED_SURFACE()
B_SPLINE_SURFACE(3,2,((#26306,#26307,#26308),(#26309,#26310,#26311),(#26312,
#26313,#26314),(#26315,#26316,#26317),(#26318,#26319,#26320),(#26321,#26322,
#26323)),.UNSPECIFIED.,.F.,.F.,.F.)
B_SPLINE_SURFACE_WITH_KNOTS((4,2,4),(3,3),(0.0008282178255691,0.00149505479343247,
0.00216189176129584),(0.,1.00047905254905),.UNSPECIFIED.)
GEOMETRIC_REPRESENTATION_ITEM()
RATIONAL_B_SPLINE_SURFACE(((1.,0.680382792843981,1.00030622687562),(1.,
0.734649451146706,1.00025423371364),(1.,0.782184849637538,1.00020868980601),
(1.,0.868668793821875,1.00012582909818),(1.,0.908363009419454,1.00008779786785),
(1.,0.940539343958763,1.00005696955769)))
REPRESENTATION_ITEM('')
SURFACE()
);
#115=(
BOUNDED_SURFACE()
B_SPLINE_SURFACE(3,2,((#26327,#26328,#26329),(#26330,#26331,#26332),(#26333,
#26334,#26335),(#26336,#26337,#26338)),.UNSPECIFIED.,.F.,.F.,.F.)
B_SPLINE_SURFACE_WITH_KNOTS((4,4),(3,3),(0.0647248597593566,0.0667277597197425),
(0.,1.),.UNSPECIFIED.)
GEOMETRIC_REPRESENTATION_ITEM()
RATIONAL_B_SPLINE_SURFACE(((1.,0.772543307031376,1.),(1.,0.773053168552096,
1.),(1.,0.773574707201185,1.),(1.,0.774108727913434,1.)))
REPRESENTATION_ITEM('')
SURFACE()
);
#116=(
BOUNDED_SURFACE()
B_SPLINE_SURFACE(3,2,((#26514,#26515,#26516),(#26517,#26518,#26519),(#26520,
#26521,#26522),(#26523,#26524,#26525)),.UNSPECIFIED.,.F.,.F.,.F.)
B_SPLINE_SURFACE_WITH_KNOTS((4,4),(3,3),(0.0554293708229056,0.0672199869527731),
(0.,1.00093204200585),.UNSPECIFIED.)
GEOMETRIC_REPRESENTATION_ITEM()
RATIONAL_B_SPLINE_SURFACE(((1.,0.586730971602853,1.00077036818836),(1.,
0.580458668844265,1.00078206028765),(1.,0.573277155067799,1.00079544723266),
(1.,0.564689221793136,1.00081145586177)))
REPRESENTATION_ITEM('')
SURFACE()
);
#117=(
BOUNDED_SURFACE()
B_SPLINE_SURFACE(3,2,((#26544,#26545,#26546),(#26547,#26548,#26549),(#26550,
#26551,#26552),(#26553,#26554,#26555),(#26556,#26557,#26558),(#26559,#26560,
#26561)),.UNSPECIFIED.,.F.,.F.,.F.)
B_SPLINE_SURFACE_WITH_KNOTS((4,2,4),(3,3),(0.000315513320331309,0.000961720209151386,
0.00160792712678291),(-0.00216992935563672,1.),.UNSPECIFIED.)
GEOMETRIC_REPRESENTATION_ITEM()
RATIONAL_B_SPLINE_SURFACE(((1.00140856317452,0.675435706958829,1.),(1.0011348049795,
0.738515685647825,1.),(1.00088601384349,0.795842698474753,1.),(1.00048533380011,
0.888168294775546,1.),(1.00032603746852,0.924873713590241,1.),(1.0003127391567,
0.927937940493613,1.)))
REPRESENTATION_ITEM('')
SURFACE()
);
#118=(
BOUNDED_SURFACE()
B_SPLINE_SURFACE(3,2,((#26563,#26564,#26565),(#26566,#26567,#26568),(#26569,
#26570,#26571),(#26572,#26573,#26574),(#26575,#26576,#26577),(#26578,#26579,
#26580)),.UNSPECIFIED.,.F.,.F.,.F.)
B_SPLINE_SURFACE_WITH_KNOTS((4,2,4),(3,3),(0.000402895580047916,0.000905401753400752,
0.00140790792675359),(0.,1.),.UNSPECIFIED.)
GEOMETRIC_REPRESENTATION_ITEM()
RATIONAL_B_SPLINE_SURFACE(((1.,0.813540597401216,1.),(1.,0.813784197152609,
1.),(1.,0.801974141899261,1.),(1.,0.763153562323214,1.),(1.,0.735816595983473,
1.),(1.,0.707106781186551,1.)))
REPRESENTATION_ITEM('')
SURFACE()
);
#119=(
BOUNDED_SURFACE()
B_SPLINE_SURFACE(3,2,((#26581,#26582,#26583),(#26584,#26585,#26586),(#26587,
#26588,#26589),(#26590,#26591,#26592),(#26593,#26594,#26595),(#26596,#26597,
#26598),(#26599,#26600,#26601),(#26602,#26603,#26604),(#26605,#26606,#26607),
(#26608,#26609,#26610)),.UNSPECIFIED.,.F.,.F.,.F.)
B_SPLINE_SURFACE_WITH_KNOTS((4,2,2,2,4),(3,3),(0.000512156798994636,0.000771582496110804,
0.00103100819322697,0.00129043389034314,0.00154985958745931),(0.,1.),
 .UNSPECIFIED.)
GEOMETRIC_REPRESENTATION_ITEM()
RATIONAL_B_SPLINE_SURFACE(((1.,0.707106781186548,1.),(1.,0.687254414974208,
1.),(1.,0.666880865312242,1.),(1.,0.625068437161066,1.),(1.,0.604779625068108,
1.),(1.,0.566741718306607,1.),(1.,0.550156755482368,1.),(1.,0.525956792300315,
1.),(1.,0.519123228378055,1.),(1.,0.51911513123826,1.)))
REPRESENTATION_ITEM('')
SURFACE()
);
#120=(
BOUNDED_SURFACE()
B_SPLINE_SURFACE(3,2,((#26613,#26614,#26615),(#26616,#26617,#26618),(#26619,
#26620,#26621),(#26622,#26623,#26624),(#26625,#26626,#26627),(#26628,#26629,
#26630)),.UNSPECIFIED.,.F.,.F.,.F.)
B_SPLINE_SURFACE_WITH_KNOTS((4,2,4),(3,3),(0.000402895580047916,0.000905401753400748,
0.00140790792675358),(0.,1.),.UNSPECIFIED.)
GEOMETRIC_REPRESENTATION_ITEM()
RATIONAL_B_SPLINE_SURFACE(((1.,0.813540597401212,1.),(1.,0.813784197152736,
1.),(1.,0.801974141899088,1.),(1.,0.763153562323395,1.),(1.,0.735816595983341,
1.),(1.,0.707106781186551,1.)))
REPRESENTATION_ITEM('')
SURFACE()
);
#121=(
BOUNDED_SURFACE()
B_SPLINE_SURFACE(3,2,((#26632,#26633,#26634),(#26635,#26636,#26637),(#26638,
#26639,#26640),(#26641,#26642,#26643),(#26644,#26645,#26646),(#26647,#26648,
#26649),(#26650,#26651,#26652),(#26653,#26654,#26655),(#26656,#26657,#26658),
(#26659,#26660,#26661)),.UNSPECIFIED.,.F.,.F.,.F.)
B_SPLINE_SURFACE_WITH_KNOTS((4,2,2,2,4),(3,3),(0.000140109886326165,0.000666559814939612,
0.00108521714444997,0.00150387447396033,0.00203032440257419),(-0.000871030383667572,
1.),.UNSPECIFIED.)
GEOMETRIC_REPRESENTATION_ITEM()
RATIONAL_B_SPLINE_SURFACE(((1.0009257248349,0.468603591646683,1.),(1.00081905401893,
0.529836137586218,1.),(1.0007156861837,0.58917266428352,1.),(1.0005499585439,
0.684305763489983,1.),(1.0004825032405,0.723027319401027,1.),(1.00035800741905,
0.794492002941265,1.),(1.0003025878804,0.82630463525224,1.),(1.00018948908547,
0.891227051878505,1.),(1.00013836850245,0.920571942699409,1.),(1.00011502671664,
0.933970893096821,1.)))
REPRESENTATION_ITEM('')
SURFACE()
);
#122=(
BOUNDED_SURFACE()
B_SPLINE_SURFACE(3,2,((#26662,#26663,#26664),(#26665,#26666,#26667),(#26668,
#26669,#26670),(#26671,#26672,#26673),(#26674,#26675,#26676),(#26677,#26678,
#26679),(#26680,#26681,#26682),(#26683,#26684,#26685)),.UNSPECIFIED.,.F.,
 .F.,.F.)
B_SPLINE_SURFACE_WITH_KNOTS((4,2,2,4),(3,3),(0.000174437971377122,0.00101920216019029,
0.00137118723886245,0.00186396634900331),(0.,1.00024356555371),
 .UNSPECIFIED.)
GEOMETRIC_REPRESENTATION_ITEM()
RATIONAL_B_SPLINE_SURFACE(((1.,0.539098756316595,1.00022451933325),(1.,
0.633858154865795,1.00017835908249),(1.,0.71717834105338,1.00013777122792),
(1.,0.814824555145193,1.00009020471952),(1.,0.841538081526984,1.00007719172983),
(1.,0.898531920368038,1.000049428258),(1.,0.925786672706506,1.00003615162031),
(1.,0.937456960617548,1.00003046666004)))
REPRESENTATION_ITEM('')
SURFACE()
);
#123=(
BOUNDED_SURFACE()
B_SPLINE_SURFACE(3,2,((#26739,#26740,#26741),(#26742,#26743,#26744),(#26745,
#26746,#26747),(#26748,#26749,#26750),(#26751,#26752,#26753),(#26754,#26755,
#26756),(#26757,#26758,#26759),(#26760,#26761,#26762),(#26763,#26764,#26765),
(#26766,#26767,#26768)),.UNSPECIFIED.,.F.,.F.,.F.)
B_SPLINE_SURFACE_WITH_KNOTS((4,2,2,2,4),(3,3),(0.000329019594182719,0.000643209132708097,
0.00081775887649227,0.00116685836406061,0.00200469706399139),(-0.00396994925120382,
1.),.UNSPECIFIED.)
GEOMETRIC_REPRESENTATION_ITEM()
RATIONAL_B_SPLINE_SURFACE(((1.00073501707975,0.907427396014608,1.),(1.0006151512306,
0.922524043548314,1.),(1.0005458872431,0.931247579180626,1.),(1.00054531256463,
0.93131995774664,1.),(1.00056655237234,0.928644884796926,1.),(1.00068340691748,
0.913927499543062,1.),(1.0008290722116,0.895581510097823,1.),(1.00142178903442,
0.820931081928786,1.),(1.00200380422865,0.747628483154187,1.),(1.00265356605419,
0.665793453986733,1.)))
REPRESENTATION_ITEM('')
SURFACE()
);
#124=(
BOUNDED_SURFACE()
B_SPLINE_SURFACE(3,2,((#26878,#26879,#26880),(#26881,#26882,#26883),(#26884,
#26885,#26886),(#26887,#26888,#26889)),.UNSPECIFIED.,.F.,.F.,.F.)
B_SPLINE_SURFACE_WITH_KNOTS((4,4),(3,3),(0.0650014074844314,0.0670796431839287),
(0.,1.),.UNSPECIFIED.)
GEOMETRIC_REPRESENTATION_ITEM()
RATIONAL_B_SPLINE_SURFACE(((1.,0.601781042690497,1.),(1.,0.600836260738914,
1.),(1.,0.599866989417508,1.),(1.,0.598871405423911,1.)))
REPRESENTATION_ITEM('')
SURFACE()
);
#125=(
BOUNDED_SURFACE()
B_SPLINE_SURFACE(3,2,((#26893,#26894,#26895),(#26896,#26897,#26898),(#26899,
#26900,#26901),(#26902,#26903,#26904),(#26905,#26906,#26907),(#26908,#26909,
#26910)),.UNSPECIFIED.,.F.,.F.,.F.)
B_SPLINE_SURFACE_WITH_KNOTS((4,2,4),(3,3),(0.000402651921819611,0.000906087614430015,
0.00140952330704042),(0.,1.),.UNSPECIFIED.)
GEOMETRIC_REPRESENTATION_ITEM()
RATIONAL_B_SPLINE_SURFACE(((1.,0.813540597401223,1.),(1.,0.81373934553701,
1.),(1.,0.802648961762943,1.),(1.,0.764608789261887,1.),(1.,0.737258306119129,
1.),(1.,0.707106781186548,1.)))
REPRESENTATION_ITEM('')
SURFACE()
);
#126=(
BOUNDED_SURFACE()
B_SPLINE_SURFACE(3,2,((#26948,#26949,#26950),(#26951,#26952,#26953),(#26954,
#26955,#26956),(#26957,#26958,#26959),(#26960,#26961,#26962),(#26963,#26964,
#26965)),.UNSPECIFIED.,.F.,.F.,.F.)
B_SPLINE_SURFACE_WITH_KNOTS((4,2,4),(3,3),(0.000351891753521461,0.000906087614430015,
0.00146028347533855),(0.,1.0000507601683),.UNSPECIFIED.)
GEOMETRIC_REPRESENTATION_ITEM()
RATIONAL_B_SPLINE_SURFACE(((1.,0.813123248342986,1.00001897179073),(1.,
0.815885817109806,1.00001869133382),(1.,0.804556789508961,1.00001984146051),
(1.,0.762678995446481,1.00002409290826),(1.,0.731644634342391,1.00002724352705),
(0.999999999999999,0.697891377178904,1.00003067016908)))
REPRESENTATION_ITEM('')
SURFACE()
);
#127=(
BOUNDED_SURFACE()
B_SPLINE_SURFACE(3,2,((#26983,#26984,#26985),(#26986,#26987,#26988),(#26989,
#26990,#26991),(#26992,#26993,#26994),(#26995,#26996,#26997),(#26998,#26999,
#27000),(#27001,#27002,#27003),(#27004,#27005,#27006),(#27007,#27008,#27009),
(#27010,#27011,#27012)),.UNSPECIFIED.,.F.,.F.,.F.)
B_SPLINE_SURFACE_WITH_KNOTS((4,2,2,2,4),(3,3),(0.000758206618216247,0.00101809884720579,
0.00127799107619532,0.00153788330518486,0.0017977755341744),(0.,1.),
 .UNSPECIFIED.)
GEOMETRIC_REPRESENTATION_ITEM()
RATIONAL_B_SPLINE_SURFACE(((1.,0.707106781186548,1.),(1.,0.686991483272722,
1.),(1.,0.666460369298913,1.),(1.,0.624470895230527,1.),(1.,0.604201592515,
1.),(1.,0.566291012805924,1.),(1.,0.54984436360562,1.),(1.,0.525862225699491,
1.),(1.,0.519128088730035,1.),(1.,0.51911513123826,1.)))
REPRESENTATION_ITEM('')
SURFACE()
);
#128=(
BOUNDED_SURFACE()
B_SPLINE_SURFACE(3,2,((#27110,#27111,#27112),(#27113,#27114,#27115),(#27116,
#27117,#27118),(#27119,#27120,#27121),(#27122,#27123,#27124),(#27125,#27126,
#27127),(#27128,#27129,#27130),(#27131,#27132,#27133),(#27134,#27135,#27136),
(#27137,#27138,#27139)),.UNSPECIFIED.,.F.,.F.,.F.)
B_SPLINE_SURFACE_WITH_KNOTS((4,2,2,2,4),(3,3),(0.000512156798994631,0.0007715824961108,
0.00103100819322697,0.00129043389034314,0.00154985958745931),(0.,1.),
 .UNSPECIFIED.)
GEOMETRIC_REPRESENTATION_ITEM()
RATIONAL_B_SPLINE_SURFACE(((1.,0.707106781186548,1.),(1.,0.687254414974094,
1.),(1.,0.666880865312397,1.),(1.,0.62506843716091,1.),(1.,0.604779625068046,
1.),(1.,0.56674171830669,1.),(1.,0.550156755482675,1.),(1.,0.525956792299999,
1.),(1.,0.519123228378293,1.),(1.,0.51911513123826,1.)))
REPRESENTATION_ITEM('')
SURFACE()
);
#129=(
BOUNDED_SURFACE()
B_SPLINE_SURFACE(3,2,((#27247,#27248,#27249),(#27250,#27251,#27252),(#27253,
#27254,#27255),(#27256,#27257,#27258),(#27259,#27260,#27261),(#27262,#27263,
#27264),(#27265,#27266,#27267),(#27268,#27269,#27270),(#27271,#27272,#27273),
(#27274,#27275,#27276)),.UNSPECIFIED.,.F.,.F.,.F.)
B_SPLINE_SURFACE_WITH_KNOTS((4,2,2,2,4),(3,3),(0.000758206618216244,0.00101809884720578,
0.00127799107619532,0.00153788330518486,0.0017977755341744),(0.,1.),
 .UNSPECIFIED.)
GEOMETRIC_REPRESENTATION_ITEM()
RATIONAL_B_SPLINE_SURFACE(((1.,0.707106781186548,1.),(1.,0.686991483272723,
1.),(1.,0.666460369298916,1.),(1.,0.62447089523053,1.),(1.,0.604201592515084,
1.),(1.,0.566291012805851,1.),(1.,0.549844363605341,1.),(1.,0.525862225699786,
1.),(1.,0.519128088729817,1.),(1.,0.519115131238269,1.)))
REPRESENTATION_ITEM('')
SURFACE()
);
#130=(
BOUNDED_SURFACE()
B_SPLINE_SURFACE(3,2,((#27282,#27283,#27284),(#27285,#27286,#27287),(#27288,
#27289,#27290),(#27291,#27292,#27293)),.UNSPECIFIED.,.F.,.F.,.F.)
B_SPLINE_SURFACE_WITH_KNOTS((4,4),(3,3),(0.0650014074844314,0.0670796431839287),
(0.,1.),.UNSPECIFIED.)
GEOMETRIC_REPRESENTATION_ITEM()
RATIONAL_B_SPLINE_SURFACE(((1.,0.601781042690495,1.),(1.,0.600836260738911,
1.),(1.,0.599866989417508,1.),(1.,0.598871405423905,1.)))
REPRESENTATION_ITEM('')
SURFACE()
);
#131=(
BOUNDED_SURFACE()
B_SPLINE_SURFACE(3,2,((#27355,#27356,#27357),(#27358,#27359,#27360),(#27361,
#27362,#27363),(#27364,#27365,#27366),(#27367,#27368,#27369),(#27370,#27371,
#27372),(#27373,#27374,#27375),(#27376,#27377,#27378)),.UNSPECIFIED.,.F.,
 .F.,.F.)
B_SPLINE_SURFACE_WITH_KNOTS((4,2,2,4),(3,3),(0.000174437971377159,0.00101920216019031,
0.00137118723886246,0.00186396634900331),(0.,1.00024356555379),
 .UNSPECIFIED.)
GEOMETRIC_REPRESENTATION_ITEM()
RATIONAL_B_SPLINE_SURFACE(((1.,0.53909875631675,1.00022451933332),(1.,0.633858154865377,
1.00017835908255),(1.,0.717178341053683,1.00013777122797),(1.,0.81482455514504,
1.00009020471955),(1.,0.841538081527261,1.00007719172985),(1.,0.898531920367626,
1.00004942825801),(1.,0.925786672707243,1.00003615162032),(1.,0.937456960616858,
1.00003046666005)))
REPRESENTATION_ITEM('')
SURFACE()
);
#132=(
BOUNDED_SURFACE()
B_SPLINE_SURFACE(3,2,((#27432,#27433,#27434),(#27435,#27436,#27437),(#27438,
#27439,#27440),(#27441,#27442,#27443),(#27444,#27445,#27446),(#27447,#27448,
#27449),(#27450,#27451,#27452),(#27453,#27454,#27455),(#27456,#27457,#27458),
(#27459,#27460,#27461)),.UNSPECIFIED.,.F.,.F.,.F.)
B_SPLINE_SURFACE_WITH_KNOTS((4,2,2,2,4),(3,3),(0.000329019594184677,0.000643209132708098,
0.000817758876492274,0.00116685836406063,0.0020046970639932),(-0.00396994925886359,
1.),.UNSPECIFIED.)
GEOMETRIC_REPRESENTATION_ITEM()
RATIONAL_B_SPLINE_SURFACE(((1.00073501708117,0.907427396013494,1.),(1.00061515123179,
0.922524043548232,1.),(1.00054588724416,0.931247579179964,1.),(1.00054531256569,
0.93131995774619,1.),(1.00056655237344,0.928644884796249,1.),(1.0006834069188,
0.913927499542673,1.),(1.0008290722132,0.89558151009713,1.),(1.00142178903718,
0.820931081927077,1.),(1.00200380423254,0.747628483152259,1.),(1.00265356605933,
0.665793453983509,1.)))
REPRESENTATION_ITEM('')
SURFACE()
);
#133=(
BOUNDED_SURFACE()
B_SPLINE_SURFACE(3,2,((#27466,#27467,#27468),(#27469,#27470,#27471),(#27472,
#27473,#27474),(#27475,#27476,#27477)),.UNSPECIFIED.,.F.,.F.,.F.)
B_SPLINE_SURFACE_WITH_KNOTS((4,4),(3,3),(0.0554293708055474,0.0672199869701312),
(0.,1.00093204202321),.UNSPECIFIED.)
GEOMETRIC_REPRESENTATION_ITEM()
RATIONAL_B_SPLINE_SURFACE(((1.,0.586730971623377,1.00077036820267),(1.,
0.580458668848917,1.00078206030221),(1.,0.573277155051876,1.00079544724751),
(1.,0.564689221747664,1.00081145587697)))
REPRESENTATION_ITEM('')
SURFACE()
);
#134=(
BOUNDED_SURFACE()
B_SPLINE_SURFACE(3,2,((#27492,#27493,#27494),(#27495,#27496,#27497),(#27498,
#27499,#27500),(#27501,#27502,#27503),(#27504,#27505,#27506),(#27507,#27508,
#27509),(#27510,#27511,#27512),(#27513,#27514,#27515),(#27516,#27517,#27518),
(#27519,#27520,#27521)),.UNSPECIFIED.,.F.,.F.,.F.)
B_SPLINE_SURFACE_WITH_KNOTS((4,2,2,2,4),(3,3),(0.000512156798994632,0.000771582496110797,
0.00103100819322696,0.00129043389034313,0.00154985958745929),(0.,1.),
 .UNSPECIFIED.)
GEOMETRIC_REPRESENTATION_ITEM()
RATIONAL_B_SPLINE_SURFACE(((1.,0.707106781186553,1.),(1.,0.687254414974218,
1.),(1.,0.66688086531225,1.),(1.,0.625068437161066,1.),(1.,0.604779625067387,
1.),(1.,0.566741718307357,1.),(1.,0.550156755482311,1.),(1.,0.525956792300389,
1.),(1.,0.519123228378017,1.),(1.,0.519115131238272,1.)))
REPRESENTATION_ITEM('')
SURFACE()
);
#135=(
BOUNDED_SURFACE()
B_SPLINE_SURFACE(3,2,((#27525,#27526,#27527),(#27528,#27529,#27530),(#27531,
#27532,#27533),(#27534,#27535,#27536),(#27537,#27538,#27539),(#27540,#27541,
#27542)),.UNSPECIFIED.,.F.,.F.,.F.)
B_SPLINE_SURFACE_WITH_KNOTS((4,2,4),(3,3),(0.00081372363230002,0.00148053147917474,
0.00214733932604946),(0.,1.00047905251364),.UNSPECIFIED.)
GEOMETRIC_REPRESENTATION_ITEM()
RATIONAL_B_SPLINE_SURFACE(((1.,0.680382792855505,1.00030622685297),(1.,
0.734649451155677,1.00025423369484),(1.,0.782184849645572,1.00020868979057),
(1.,0.868668793826199,1.00012582908887),(1.,0.908363009423125,1.00008779786136),
(1.,0.940539343960651,1.00005696955348)))
REPRESENTATION_ITEM('')
SURFACE()
);
#136=(
BOUNDED_SURFACE()
B_SPLINE_SURFACE(3,2,((#27569,#27570,#27571),(#27572,#27573,#27574),(#27575,
#27576,#27577),(#27578,#27579,#27580),(#27581,#27582,#27583),(#27584,#27585,
#27586),(#27587,#27588,#27589),(#27590,#27591,#27592),(#27593,#27594,#27595),
(#27596,#27597,#27598)),.UNSPECIFIED.,.F.,.F.,.F.)
B_SPLINE_SURFACE_WITH_KNOTS((4,2,2,2,4),(3,3),(0.00014010988641719,0.000666559814939611,
0.00108521714444997,0.00150387447396033,0.00203032440248315),(-0.000871030382132827,
1.),.UNSPECIFIED.)
GEOMETRIC_REPRESENTATION_ITEM()
RATIONAL_B_SPLINE_SURFACE(((1.00092572483321,0.468603591680183,1.),(1.00081905401745,
0.529836137605996,1.),(1.00071568618242,0.589172664294323,1.),(1.00054995854293,
0.684305763489641,1.),(1.00048250323964,0.723027319402385,1.),(1.00035800741842,
0.794492002940648,1.),(1.00030258787986,0.826304635252159,1.),(1.00018948908515,
0.89122705187285,1.),(1.00013836850222,0.920571942688749,1.),(1.00011502671645,
0.933970893090378,1.)))
REPRESENTATION_ITEM('')
SURFACE()
);
#137=(
BOUNDED_SURFACE()
B_SPLINE_SURFACE(3,2,((#27638,#27639,#27640),(#27641,#27642,#27643),(#27644,
#27645,#27646),(#27647,#27648,#27649),(#27650,#27651,#27652),(#27653,#27654,
#27655),(#27656,#27657,#27658),(#27659,#27660,#27661),(#27662,#27663,#27664),
(#27665,#27666,#27667)),.UNSPECIFIED.,.F.,.F.,.F.)
B_SPLINE_SURFACE_WITH_KNOTS((4,2,2,2,4),(3,3),(0.0314170682308593,0.0383717968941302,
0.0418491612257657,0.0453265255574011,0.059235982883943),(0.,1.00015514532807),
 .UNSPECIFIED.)
GEOMETRIC_REPRESENTATION_ITEM()
RATIONAL_B_SPLINE_SURFACE(((1.,0.893712741719336,1.00003297994311),(1.,
0.896924595267128,1.00003198333497),(1.,0.900137133821746,1.00003098651427),
(1.,0.904798383537421,1.00002954017204),(1.,0.90632549663627,1.00002906632311),
(1.,0.90929032300076,1.00002814636519),(1.,0.910726187593208,1.00002770082983),
(1.,0.917498844645229,1.00002559933763),(1.,0.921671404518043,1.00002430463129),
(1.,0.923199103011964,1.00002383060072)))
REPRESENTATION_ITEM('')
SURFACE()
);
#138=(
BOUNDED_SURFACE()
B_SPLINE_SURFACE(3,2,((#27693,#27694,#27695),(#27696,#27697,#27698),(#27699,
#27700,#27701),(#27702,#27703,#27704),(#27705,#27706,#27707),(#27708,#27709,
#27710),(#27711,#27712,#27713),(#27714,#27715,#27716),(#27717,#27718,#27719),
(#27720,#27721,#27722)),.UNSPECIFIED.,.F.,.F.,.F.)
B_SPLINE_SURFACE_WITH_KNOTS((4,2,2,2,4),(3,3),(0.030336403536441,0.0372910338575459,
0.0407683490180983,0.0442456641786507,0.0581549248208604),(0.,1.),
 .UNSPECIFIED.)
GEOMETRIC_REPRESENTATION_ITEM()
RATIONAL_B_SPLINE_SURFACE(((1.,0.893729285230291,1.),(1.,0.89693986940859,
1.),(1.,0.900150686104346,1.),(1.,0.904808789102114,1.),(1.,0.906334760566898,
1.),(1.,0.909297199463304,1.),(1.,0.91073457572851,1.),(1.,0.917512859277436,
1.),(1.,0.921684639637439,1.),(1.,0.923210992612934,1.)))
REPRESENTATION_ITEM('')
SURFACE()
);
#139=(
BOUNDED_SURFACE()
B_SPLINE_SURFACE(3,2,((#27724,#27725,#27726),(#27727,#27728,#27729),(#27730,
#27731,#27732),(#27733,#27734,#27735),(#27736,#27737,#27738),(#27739,#27740,
#27741)),.UNSPECIFIED.,.F.,.F.,.F.)
B_SPLINE_SURFACE_WITH_KNOTS((4,2,4),(3,3),(0.000351891754458639,0.000906087614430021,
0.00146028347440139),(0.,1.00005076016736),.UNSPECIFIED.)
GEOMETRIC_REPRESENTATION_ITEM()
RATIONAL_B_SPLINE_SURFACE(((1.,0.813123248357043,1.00001897179038),(1.,
0.815885817072131,1.00001869133348),(1.,0.804556789473276,1.00001984146015),
(1.,0.762678995482577,1.00002409290781),(1.,0.73164463444712,1.00002724352654),
(1.,0.697891377350557,1.00003067016849)))
REPRESENTATION_ITEM('')
SURFACE()
);
#140=(
BOUNDED_SURFACE()
B_SPLINE_SURFACE(3,2,((#27745,#27746,#27747),(#27748,#27749,#27750),(#27751,
#27752,#27753),(#27754,#27755,#27756),(#27757,#27758,#27759),(#27760,#27761,
#27762)),.UNSPECIFIED.,.F.,.F.,.F.)
B_SPLINE_SURFACE_WITH_KNOTS((4,2,4),(3,3),(0.000158430205536936,0.000711411267607371,
0.00126439232967781),(0.,1.),.UNSPECIFIED.)
GEOMETRIC_REPRESENTATION_ITEM()
RATIONAL_B_SPLINE_SURFACE(((1.,0.707106781186549,1.),(1.,0.750151746622362,
1.),(1.,0.789079409670008,1.),(1.,0.861389858264012,1.),(1.,0.895281520101449,
1.),(1.,0.92387953251129,1.)))
REPRESENTATION_ITEM('')
SURFACE()
);
#141=(
BOUNDED_SURFACE()
B_SPLINE_SURFACE(3,2,((#27872,#27873,#27874),(#27875,#27876,#27877),(#27878,
#27879,#27880),(#27881,#27882,#27883),(#27884,#27885,#27886),(#27887,#27888,
#27889)),.UNSPECIFIED.,.F.,.F.,.F.)
B_SPLINE_SURFACE_WITH_KNOTS((4,2,4),(3,3),(0.000402895580047922,0.000905401753400751,
0.00140790792675358),(0.,1.),.UNSPECIFIED.)
GEOMETRIC_REPRESENTATION_ITEM()
RATIONAL_B_SPLINE_SURFACE(((1.,0.813540597401209,1.),(1.,0.813784197152548,
1.),(1.,0.801974141899337,1.),(1.,0.763153562323141,1.),(1.,0.735816595983534,
1.),(1.,0.707106781186548,1.)))
REPRESENTATION_ITEM('')
SURFACE()
);
#142=(
BOUNDED_SURFACE()
B_SPLINE_SURFACE(3,2,((#27891,#27892,#27893),(#27894,#27895,#27896),(#27897,
#27898,#27899),(#27900,#27901,#27902),(#27903,#27904,#27905),(#27906,#27907,
#27908)),.UNSPECIFIED.,.F.,.F.,.F.)
B_SPLINE_SURFACE_WITH_KNOTS((4,2,4),(3,3),(0.000315513320329165,0.000961720209151403,
0.00160792712680524),(-0.00216992936573831,1.),.UNSPECIFIED.)
GEOMETRIC_REPRESENTATION_ITEM()
RATIONAL_B_SPLINE_SURFACE(((1.0014085631811,0.675435706954971,1.),(1.0011348049848,
0.738515685644707,1.),(1.00088601384763,0.795842698472626,1.),(1.00048533380237,
0.88816829477593,1.),(1.00032603747003,0.924873713592137,1.),(1.00031273915816,
0.927937940493142,1.)))
REPRESENTATION_ITEM('')
SURFACE()
);
#143=(
BOUNDED_SURFACE()
B_SPLINE_SURFACE(3,2,((#27955,#27956,#27957),(#27958,#27959,#27960),(#27961,
#27962,#27963),(#27964,#27965,#27966),(#27967,#27968,#27969),(#27970,#27971,
#27972),(#27973,#27974,#27975),(#27976,#27977,#27978)),.UNSPECIFIED.,.F.,
 .F.,.F.)
B_SPLINE_SURFACE_WITH_KNOTS((4,2,2,4),(3,3),(0.000686358375502124,0.000929437613321101,
0.00117251685114008,0.00165867532677803),(0.,1.),.UNSPECIFIED.)
GEOMETRIC_REPRESENTATION_ITEM()
RATIONAL_B_SPLINE_SURFACE(((1.,0.923879532511285,1.),(1.,0.928899857577083,
1.),(1.,0.929018384212736,1.),(1.,0.920008474882453,1.),(1.,0.91087168499111,
1.),(1.,0.875139245491054,1.),(1.,0.840813078373297,1.),(1.,0.802338883728532,
1.)))
REPRESENTATION_ITEM('')
SURFACE()
);
#144=(
BOUNDED_SURFACE()
B_SPLINE_SURFACE(3,2,((#28068,#28069,#28070),(#28071,#28072,#28073),(#28074,
#28075,#28076),(#28077,#28078,#28079)),.UNSPECIFIED.,.F.,.F.,.F.)
B_SPLINE_SURFACE_WITH_KNOTS((4,4),(3,3),(0.0647248597593566,0.0667277597197425),
(0.,1.),.UNSPECIFIED.)
GEOMETRIC_REPRESENTATION_ITEM()
RATIONAL_B_SPLINE_SURFACE(((1.,0.772543307031377,1.),(1.,0.773053168552098,
1.),(1.,0.773574707201177,1.),(1.,0.774108727913437,1.)))
REPRESENTATION_ITEM('')
SURFACE()
);
#145=(
BOUNDED_SURFACE()
B_SPLINE_SURFACE(3,2,((#28081,#28082,#28083),(#28084,#28085,#28086),(#28087,
#28088,#28089),(#28090,#28091,#28092)),.UNSPECIFIED.,.F.,.F.,.F.)
B_SPLINE_SURFACE_WITH_KNOTS((4,4),(3,3),(0.0326127356995135,0.0421285143028756),
(0.,1.),.UNSPECIFIED.)
GEOMETRIC_REPRESENTATION_ITEM()
RATIONAL_B_SPLINE_SURFACE(((1.,0.773368492107045,1.),(1.,0.770480922349017,
1.),(1.,0.767957745429662,1.),(1.,0.765689104422499,1.)))
REPRESENTATION_ITEM('')
SURFACE()
);
#146=(
BOUNDED_SURFACE()
B_SPLINE_SURFACE(3,2,((#28185,#28186,#28187),(#28188,#28189,#28190),(#28191,
#28192,#28193),(#28194,#28195,#28196),(#28197,#28198,#28199),(#28200,#28201,
#28202),(#28203,#28204,#28205),(#28206,#28207,#28208)),.UNSPECIFIED.,.F.,
 .F.,.F.)
B_SPLINE_SURFACE_WITH_KNOTS((4,2,2,4),(3,3),(0.000802853902804998,0.00108948501086235,
0.00137611611891971,0.00194937833503442),(0.,1.),.UNSPECIFIED.)
GEOMETRIC_REPRESENTATION_ITEM()
RATIONAL_B_SPLINE_SURFACE(((1.,0.923879532511286,1.),(1.,0.93126028758523,
1.),(1.,0.931596165488065,1.),(1.,0.918734528780506,1.),(1.,0.905994810924508,
1.),(1.,0.858462949893356,1.),(1.,0.814112175968461,1.),(1.,0.765689104422506,
1.)))
REPRESENTATION_ITEM('')
SURFACE()
);
#147=(
BOUNDED_SURFACE()
B_SPLINE_SURFACE(3,2,((#28242,#28243,#28244),(#28245,#28246,#28247),(#28248,
#28249,#28250),(#28251,#28252,#28253),(#28254,#28255,#28256),(#28257,#28258,
#28259)),.UNSPECIFIED.,.F.,.F.,.F.)
B_SPLINE_SURFACE_WITH_KNOTS((4,2,4),(3,3),(0.00125184933893988,0.00239738856741525,
0.00354292779589063),(0.,1.),.UNSPECIFIED.)
GEOMETRIC_REPRESENTATION_ITEM()
RATIONAL_B_SPLINE_SURFACE(((1.,0.707106781186548,1.),(1.,0.752499298133503,
1.),(1.,0.791707406457373,1.),(1.,0.86205547054867,1.),(1.,0.893085809396533,
1.),(1.,0.9210299078221,1.)))
REPRESENTATION_ITEM('')
SURFACE()
);
#148=(
BOUNDED_SURFACE()
B_SPLINE_SURFACE(3,2,((#28264,#28265,#28266),(#28267,#28268,#28269),(#28270,
#28271,#28272),(#28273,#28274,#28275)),.UNSPECIFIED.,.F.,.F.,.F.)
B_SPLINE_SURFACE_WITH_KNOTS((4,4),(3,3),(0.307250934553085,0.313798890571649),
(0.,1.),.UNSPECIFIED.)
GEOMETRIC_REPRESENTATION_ITEM()
RATIONAL_B_SPLINE_SURFACE(((1.,0.712804186852904,1.),(1.,0.71296450813891,
1.),(1.,0.71313821972869,1.),(1.,0.713329401304079,1.)))
REPRESENTATION_ITEM('')
SURFACE()
);
#149=(
BOUNDED_SURFACE()
B_SPLINE_SURFACE(3,2,((#28299,#28300,#28301),(#28302,#28303,#28304),(#28305,
#28306,#28307),(#28308,#28309,#28310),(#28311,#28312,#28313),(#28314,#28315,
#28316),(#28317,#28318,#28319),(#28320,#28321,#28322)),.UNSPECIFIED.,.F.,
 .F.,.F.)
B_SPLINE_SURFACE_WITH_KNOTS((4,2,2,4),(3,3),(0.0301024650456266,0.0387558943228362,
0.0430826089614409,0.0474093236000457),(0.,1.),.UNSPECIFIED.)
GEOMETRIC_REPRESENTATION_ITEM()
RATIONAL_B_SPLINE_SURFACE(((1.,0.921029907823249,1.),(1.,0.922877070064105,
1.),(1.,0.923876933766823,1.),(1.,0.92388082420723,1.),(1.,0.923630934244524,
1.),(1.,0.92266268253527,1.),(1.,0.921946472339213,1.),(1.,0.921029907823249,
1.)))
REPRESENTATION_ITEM('')
SURFACE()
);
#150=(
BOUNDED_SURFACE()
B_SPLINE_SURFACE(3,2,((#28335,#28336,#28337),(#28338,#28339,#28340),(#28341,
#28342,#28343),(#28344,#28345,#28346),(#28347,#28348,#28349),(#28350,#28351,
#28352)),.UNSPECIFIED.,.F.,.F.,.F.)
B_SPLINE_SURFACE_WITH_KNOTS((4,2,4),(3,3),(0.000625612417698575,0.00177266924615975,
0.00291972607462092),(0.,1.),.UNSPECIFIED.)
GEOMETRIC_REPRESENTATION_ITEM()
RATIONAL_B_SPLINE_SURFACE(((1.,0.921029907823245,1.),(1.,0.89303286027976,
1.),(1.,0.862014836405081,1.),(1.,0.791625319509651,1.),(1.,0.752373092952147,
1.),(1.,0.707106781186546,1.)))
REPRESENTATION_ITEM('')
SURFACE()
);
#151=(
BOUNDED_SURFACE()
B_SPLINE_SURFACE(3,2,((#28383,#28384,#28385),(#28386,#28387,#28388),(#28389,
#28390,#28391),(#28392,#28393,#28394)),.UNSPECIFIED.,.F.,.F.,.F.)
B_SPLINE_SURFACE_WITH_KNOTS((4,4),(3,3),(0.307250934553085,0.313798890571649),
(0.,1.),.UNSPECIFIED.)
GEOMETRIC_REPRESENTATION_ITEM()
RATIONAL_B_SPLINE_SURFACE(((1.,0.712804186852904,1.),(1.,0.712964508138907,
1.),(1.,0.713138219728696,1.),(1.,0.713329401304078,1.)))
REPRESENTATION_ITEM('')
SURFACE()
);
#152=(
BOUNDED_SURFACE()
B_SPLINE_SURFACE(3,2,((#28421,#28422,#28423),(#28424,#28425,#28426),(#28427,
#28428,#28429),(#28430,#28431,#28432),(#28433,#28434,#28435),(#28436,#28437,
#28438)),.UNSPECIFIED.,.F.,.F.,.F.)
B_SPLINE_SURFACE_WITH_KNOTS((4,2,4),(3,3),(0.000678304539097152,0.00122793525694894,
0.00177756597480073),(0.,1.),.UNSPECIFIED.)
GEOMETRIC_REPRESENTATION_ITEM()
RATIONAL_B_SPLINE_SURFACE(((1.,0.70710678118654,1.),(1.,0.746184084332961,
1.),(1.,0.782509959683157,1.),(1.,0.849214842808394,1.),(1.,0.879717238316117,
1.),(1.,0.907850513788111,1.)))
REPRESENTATION_ITEM('')
SURFACE()
);
#153=(
BOUNDED_SURFACE()
B_SPLINE_SURFACE(3,2,((#28448,#28449,#28450),(#28451,#28452,#28453),(#28454,
#28455,#28456),(#28457,#28458,#28459),(#28460,#28461,#28462),(#28463,#28464,
#28465)),.UNSPECIFIED.,.F.,.F.,.F.)
B_SPLINE_SURFACE_WITH_KNOTS((4,2,4),(3,3),(0.000625612417698574,0.00177266924615979,
0.002919726074621),(0.,1.),.UNSPECIFIED.)
GEOMETRIC_REPRESENTATION_ITEM()
RATIONAL_B_SPLINE_SURFACE(((1.,0.921029907823249,1.),(1.,0.893032860280521,
1.),(1.,0.862014836404084,1.),(1.,0.791625319510648,1.),(1.,0.7523730929514,
1.),(1.,0.707106781186553,1.)))
REPRESENTATION_ITEM('')
SURFACE()
);
#154=(
BOUNDED_SURFACE()
B_SPLINE_SURFACE(3,2,((#28474,#28475,#28476),(#28477,#28478,#28479),(#28480,
#28481,#28482),(#28483,#28484,#28485),(#28486,#28487,#28488),(#28489,#28490,
#28491),(#28492,#28493,#28494),(#28495,#28496,#28497),(#28498,#28499,#28500),
(#28501,#28502,#28503),(#28504,#28505,#28506),(#28507,#28508,#28509),(#28510,
#28511,#28512),(#28513,#28514,#28515),(#28516,#28517,#28518),(#28519,#28520,
#28521),(#28522,#28523,#28524),(#28525,#28526,#28527)),.UNSPECIFIED.,.F.,
 .F.,.F.)
B_SPLINE_SURFACE_WITH_KNOTS((4,2,2,2,2,2,2,2,4),(3,3),(0.0489197875214898,
0.0601853600247889,0.0657063758111463,0.068466883704325,0.0712273915975036,
0.0822694231702183,0.085029931063397,0.0877904389565757,0.093311454742933),
(0.,1.00022354093058),.UNSPECIFIED.)
GEOMETRIC_REPRESENTATION_ITEM()
RATIONAL_B_SPLINE_SURFACE(((1.,0.907555692141296,1.00004133017321),(1.,
0.912172103884354,1.00003926625926),(1.,0.91629725938563,1.00003742197706),
(1.,0.92068483810848,1.0000354603702),(1.,0.921842485532916,1.00003494280703),
(1.,0.92303257596533,1.00003441073919),(1.,0.923338391926672,1.00003427401442),
(1.,0.923751986701146,1.0000340891037),(1.,0.923857671595064,1.0000340418539),
(1.,0.923881080298134,1.00003403138829),(1.,0.922241806174626,1.00003476427802),
(1.,0.918599911621013,1.00003639250301),(1.,0.917794373423119,1.00003675264453),
(1.,0.916066405850502,1.00003752518749),(1.,0.91514227300216,1.00003793835052),
(1.,0.912223658689289,1.00003924321004),(1.,0.910083556365811,1.00004020001097),
(1.,0.907829914607839,1.00004120757332)))
REPRESENTATION_ITEM('')
SURFACE()
);
#155=(
BOUNDED_SURFACE()
B_SPLINE_SURFACE(3,2,((#28569,#28570,#28571),(#28572,#28573,#28574),(#28575,
#28576,#28577),(#28578,#28579,#28580),(#28581,#28582,#28583),(#28584,#28585,
#28586),(#28587,#28588,#28589),(#28590,#28591,#28592)),.UNSPECIFIED.,.F.,
 .F.,.F.)
B_SPLINE_SURFACE_WITH_KNOTS((4,2,2,4),(3,3),(0.0301024650456266,0.0387558943228361,
0.0430826089614409,0.0474093236000456),(0.,1.),.UNSPECIFIED.)
GEOMETRIC_REPRESENTATION_ITEM()
RATIONAL_B_SPLINE_SURFACE(((1.,0.921029907823249,1.),(1.,0.922877070064102,
1.),(1.,0.923876933766823,1.),(1.,0.92388082420723,1.),(1.,0.923630934244043,
1.),(1.,0.922662682535757,1.),(1.,0.921946472338846,1.),(1.,0.921029907823249,
1.)))
REPRESENTATION_ITEM('')
SURFACE()
);
#156=(
BOUNDED_SURFACE()
B_SPLINE_SURFACE(3,2,((#28598,#28599,#28600),(#28601,#28602,#28603),(#28604,
#28605,#28606),(#28607,#28608,#28609)),.UNSPECIFIED.,.F.,.F.,.F.)
B_SPLINE_SURFACE_WITH_KNOTS((4,4),(3,3),(0.307250934553084,0.313798890571649),
(0.,1.),.UNSPECIFIED.)
GEOMETRIC_REPRESENTATION_ITEM()
RATIONAL_B_SPLINE_SURFACE(((1.,0.712804186852904,1.),(1.,0.712964508138908,
1.),(1.,0.713138219728696,1.),(1.,0.713329401304078,1.)))
REPRESENTATION_ITEM('')
SURFACE()
);
#157=(
BOUNDED_SURFACE()
B_SPLINE_SURFACE(3,2,((#28616,#28617,#28618),(#28619,#28620,#28621),(#28622,
#28623,#28624),(#28625,#28626,#28627),(#28628,#28629,#28630),(#28631,#28632,
#28633)),.UNSPECIFIED.,.F.,.F.,.F.)
B_SPLINE_SURFACE_WITH_KNOTS((4,2,4),(3,3),(0.00086265399393263,0.00141381336854384,
0.00196497274315506),(0.,1.),.UNSPECIFIED.)
GEOMETRIC_REPRESENTATION_ITEM()
RATIONAL_B_SPLINE_SURFACE(((1.,0.707106781186548,1.),(1.,0.746708654901981,
1.),(1.,0.782505247018089,1.),(1.,0.84894802268141,1.),(1.,0.87977370861613,
1.),(1.,0.90785051378974,1.)))
REPRESENTATION_ITEM('')
SURFACE()
);
#158=(
BOUNDED_SURFACE()
B_SPLINE_SURFACE(3,2,((#28637,#28638,#28639),(#28640,#28641,#28642),(#28643,
#28644,#28645),(#28646,#28647,#28648),(#28649,#28650,#28651),(#28652,#28653,
#28654)),.UNSPECIFIED.,.F.,.F.,.F.)
B_SPLINE_SURFACE_WITH_KNOTS((4,2,4),(3,3),(0.00125184933893988,0.00239738856741524,
0.00354292779589061),(0.,1.),.UNSPECIFIED.)
GEOMETRIC_REPRESENTATION_ITEM()
RATIONAL_B_SPLINE_SURFACE(((1.,0.707106781186555,1.),(1.,0.752499298132554,
1.),(1.,0.791707406458655,1.),(1.,0.862055470547405,1.),(1.,0.893085809397482,
1.),(1.,0.921029907822106,1.)))
REPRESENTATION_ITEM('')
SURFACE()
);
#159=(
BOUNDED_SURFACE()
B_SPLINE_SURFACE(3,2,((#28656,#28657,#28658),(#28659,#28660,#28661),(#28662,
#28663,#28664),(#28665,#28666,#28667),(#28668,#28669,#28670),(#28671,#28672,
#28673)),.UNSPECIFIED.,.F.,.F.,.F.)
B_SPLINE_SURFACE_WITH_KNOTS((4,2,4),(3,3),(0.00125184933893988,0.00239738856741526,
0.00354292779589064),(0.,1.),.UNSPECIFIED.)
GEOMETRIC_REPRESENTATION_ITEM()
RATIONAL_B_SPLINE_SURFACE(((1.,0.707106781186548,1.),(1.,0.752499298132371,
1.),(1.,0.791707406458881,1.),(1.,0.862055470547165,1.),(1.,0.893085809397659,
1.),(1.,0.9210299078221,1.)))
REPRESENTATION_ITEM('')
SURFACE()
);
#160=(
BOUNDED_SURFACE()
B_SPLINE_SURFACE(3,2,((#28721,#28722,#28723),(#28724,#28725,#28726),(#28727,
#28728,#28729),(#28730,#28731,#28732),(#28733,#28734,#28735),(#28736,#28737,
#28738)),.UNSPECIFIED.,.F.,.F.,.F.)
B_SPLINE_SURFACE_WITH_KNOTS((4,2,4),(3,3),(0.0491065561917184,0.0576730069527121,
0.0662394577137058),(0.,1.),.UNSPECIFIED.)
GEOMETRIC_REPRESENTATION_ITEM()
RATIONAL_B_SPLINE_SURFACE(((1.,0.921029907823248,1.),(1.,0.922875643094769,
1.),(1.,0.923881929396489,1.),(1.,0.923877126948933,1.),(1.,0.922867245922119,
1.),(1.,0.921029907823249,1.)))
REPRESENTATION_ITEM('')
SURFACE()
);
#161=(
BOUNDED_SURFACE()
B_SPLINE_SURFACE(3,2,((#28750,#28751,#28752),(#28753,#28754,#28755),(#28756,
#28757,#28758),(#28759,#28760,#28761),(#28762,#28763,#28764),(#28765,#28766,
#28767)),.UNSPECIFIED.,.F.,.F.,.F.)
B_SPLINE_SURFACE_WITH_KNOTS((4,2,4),(3,3),(0.000862653993932642,0.00141381336854385,
0.00196497274315505),(0.,1.),.UNSPECIFIED.)
GEOMETRIC_REPRESENTATION_ITEM()
RATIONAL_B_SPLINE_SURFACE(((1.,0.70710678118654,1.),(1.,0.746708654901505,
1.),(1.,0.782505247018736,1.),(1.,0.84894802268075,1.),(1.,0.879773708616637,
1.),(1.,0.907850513789743,1.)))
REPRESENTATION_ITEM('')
SURFACE()
);
#162=(
BOUNDED_SURFACE()
B_SPLINE_SURFACE(3,2,((#28777,#28778,#28779),(#28780,#28781,#28782),(#28783,
#28784,#28785),(#28786,#28787,#28788),(#28789,#28790,#28791),(#28792,#28793,
#28794)),.UNSPECIFIED.,.F.,.F.,.F.)
B_SPLINE_SURFACE_WITH_KNOTS((4,2,4),(3,3),(0.000625612417698576,0.00177266924615977,
0.00291972607462096),(0.,1.),.UNSPECIFIED.)
GEOMETRIC_REPRESENTATION_ITEM()
RATIONAL_B_SPLINE_SURFACE(((1.,0.92102990782325,1.),(1.,0.893032860280475,
1.),(1.,0.862014836404147,1.),(1.,0.791625319510585,1.),(1.,0.752373092951458,
1.),(1.,0.707106781186553,1.)))
REPRESENTATION_ITEM('')
SURFACE()
);
#163=(
BOUNDED_SURFACE()
B_SPLINE_SURFACE(3,2,((#28818,#28819,#28820),(#28821,#28822,#28823),(#28824,
#28825,#28826),(#28827,#28828,#28829),(#28830,#28831,#28832),(#28833,#28834,
#28835),(#28836,#28837,#28838),(#28839,#28840,#28841),(#28842,#28843,#28844),
(#28845,#28846,#28847),(#28848,#28849,#28850),(#28851,#28852,#28853),(#28854,
#28855,#28856),(#28857,#28858,#28859),(#28860,#28861,#28862),(#28863,#28864,
#28865),(#28866,#28867,#28868),(#28869,#28870,#28871)),.UNSPECIFIED.,.F.,
 .F.,.F.)
B_SPLINE_SURFACE_WITH_KNOTS((4,2,2,2,2,2,2,2,4),(3,3),(0.0489197875016647,
0.060185360024789,0.0657063758111463,0.068466883704325,0.0712273915975037,
0.0822694231702183,0.085029931063397,0.0877904389565757,0.0933114547429331),
(0.,1.00022354095041),.UNSPECIFIED.)
GEOMETRIC_REPRESENTATION_ITEM()
RATIONAL_B_SPLINE_SURFACE(((1.,0.907555692115104,1.00004133017689),(1.,
0.912172103867759,1.00003926626275),(1.,0.916297259379205,1.00003742198038),
(1.,0.920684838106704,1.00003546037334),(1.,0.921842485531367,1.00003494281013),
(1.,0.923032575963804,1.00003441074224),(1.,0.923338391925153,1.00003427401746),
(1.,0.923751986699634,1.00003408910672),(1.,0.923857671593554,1.00003404185692),
(1.,0.923881080296625,1.00003403139131),(1.,0.922241806173293,1.0000347642811),
(1.,0.918599911619347,1.00003639250624),(1.,0.917794373421593,1.00003675264779),
(1.,0.916066405848735,1.00003752519082),(1.,0.915142273000684,1.00003793835389),
(1.,0.912223658687137,1.00003924321352),(1.,0.910083556364339,1.00004020001454),
(1.,0.907829914606016,1.00004120757698)))
REPRESENTATION_ITEM('')
SURFACE()
);
#164=(
BOUNDED_SURFACE()
B_SPLINE_SURFACE(3,2,((#28898,#28899,#28900),(#28901,#28902,#28903),(#28904,
#28905,#28906),(#28907,#28908,#28909)),.UNSPECIFIED.,.F.,.F.,.F.)
B_SPLINE_SURFACE_WITH_KNOTS((4,4),(3,3),(0.306318309032005,0.312866265050619),
(0.,1.),.UNSPECIFIED.)
GEOMETRIC_REPRESENTATION_ITEM()
RATIONAL_B_SPLINE_SURFACE(((1.,0.712804186852904,1.),(1.,0.712964508138909,
1.),(1.,0.713138219728695,1.),(1.,0.713329401304078,1.)))
REPRESENTATION_ITEM('')
SURFACE()
);
#165=(
BOUNDED_SURFACE()
B_SPLINE_SURFACE(3,2,((#28925,#28926,#28927),(#28928,#28929,#28930),(#28931,
#28932,#28933),(#28934,#28935,#28936)),.UNSPECIFIED.,.F.,.F.,.F.)
B_SPLINE_SURFACE_WITH_KNOTS((4,4),(3,3),(0.307250934553084,0.313798890571649),
(0.,1.),.UNSPECIFIED.)
GEOMETRIC_REPRESENTATION_ITEM()
RATIONAL_B_SPLINE_SURFACE(((1.,0.712804186852904,1.),(1.,0.712964508138909,
1.),(1.,0.713138219728695,1.),(1.,0.713329401304078,1.)))
REPRESENTATION_ITEM('')
SURFACE()
);
#166=(
BOUNDED_SURFACE()
B_SPLINE_SURFACE(3,2,((#28962,#28963,#28964),(#28965,#28966,#28967),(#28968,
#28969,#28970),(#28971,#28972,#28973),(#28974,#28975,#28976),(#28977,#28978,
#28979)),.UNSPECIFIED.,.F.,.F.,.F.)
B_SPLINE_SURFACE_WITH_KNOTS((4,2,4),(3,3),(0.00067830453909708,0.00122793525694887,
0.00177756597480066),(0.,1.),.UNSPECIFIED.)
GEOMETRIC_REPRESENTATION_ITEM()
RATIONAL_B_SPLINE_SURFACE(((1.,0.70710678118654,1.),(1.,0.74618408433299,
1.),(1.,0.78250995968311,1.),(1.,0.849214842808429,1.),(1.,0.879717238316075,
1.),(1.,0.907850513788108,1.)))
REPRESENTATION_ITEM('')
SURFACE()
);
#167=(
BOUNDED_SURFACE()
B_SPLINE_SURFACE(3,2,((#28981,#28982,#28983),(#28984,#28985,#28986),(#28987,
#28988,#28989),(#28990,#28991,#28992),(#28993,#28994,#28995),(#28996,#28997,
#28998)),.UNSPECIFIED.,.F.,.F.,.F.)
B_SPLINE_SURFACE_WITH_KNOTS((4,2,4),(3,3),(0.000678304539097056,0.00122793525694883,
0.0017775659748006),(0.,1.),.UNSPECIFIED.)
GEOMETRIC_REPRESENTATION_ITEM()
RATIONAL_B_SPLINE_SURFACE(((1.,0.707106781186548,1.),(1.,0.746184084332992,
1.),(1.,0.782509959683127,1.),(1.,0.849214842808424,1.),(1.,0.8797172383161,
1.),(1.,0.90785051378811,1.)))
REPRESENTATION_ITEM('')
SURFACE()
);
#168=(
BOUNDED_SURFACE()
B_SPLINE_SURFACE(3,2,((#29008,#29009,#29010),(#29011,#29012,#29013),(#29014,
#29015,#29016),(#29017,#29018,#29019),(#29020,#29021,#29022),(#29023,#29024,
#29025)),.UNSPECIFIED.,.F.,.F.,.F.)
B_SPLINE_SURFACE_WITH_KNOTS((4,2,4),(3,3),(0.000625612417698575,0.00177266924615975,
0.00291972607462092),(0.,1.),.UNSPECIFIED.)
GEOMETRIC_REPRESENTATION_ITEM()
RATIONAL_B_SPLINE_SURFACE(((1.,0.921029907823245,1.),(1.,0.89303286027976,
1.),(1.,0.862014836405081,1.),(1.,0.791625319509651,1.),(1.,0.752373092952147,
1.),(1.,0.707106781186546,1.)))
REPRESENTATION_ITEM('')
SURFACE()
);
#169=(
BOUNDED_SURFACE()
B_SPLINE_SURFACE(3,2,((#29047,#29048,#29049),(#29050,#29051,#29052),(#29053,
#29054,#29055),(#29056,#29057,#29058),(#29059,#29060,#29061),(#29062,#29063,
#29064),(#29065,#29066,#29067),(#29068,#29069,#29070),(#29071,#29072,#29073),
(#29074,#29075,#29076),(#29077,#29078,#29079),(#29080,#29081,#29082),(#29083,
#29084,#29085),(#29086,#29087,#29088),(#29089,#29090,#29091),(#29092,#29093,
#29094),(#29095,#29096,#29097),(#29098,#29099,#29100),(#29101,#29102,#29103),
(#29104,#29105,#29106)),.UNSPECIFIED.,.F.,.F.,.F.)
B_SPLINE_SURFACE_WITH_KNOTS((4,2,2,2,2,2,2,2,2,4),(3,3),(0.0165870372170484,
0.0222388347236946,0.0250006537634149,0.0277624728031351,0.0388097489620161,
0.0415715680017363,0.0443333870414566,0.049857025120897,0.0553806632003375,
0.0610324607069837),(-0.000128159427205692,1.),.UNSPECIFIED.)
GEOMETRIC_REPRESENTATION_ITEM()
RATIONAL_B_SPLINE_SURFACE(((1.00002366285482,0.907681957774734,1.),(1.00002307158425,
0.909988735295067,1.),(1.00002250978471,0.912180534803509,1.),(1.0000217503978,
0.915143199855024,1.),(1.00002151350586,0.916067407863037,1.),(1.00002107037521,
0.917796233671169,1.),(1.00002086466642,0.918598784051383,1.),(1.00001993577826,
0.922222739703994,1.),(1.00001951311599,0.923871710355246,1.),(1.00001951373601,
0.923869291421499,1.),(1.00001953985541,0.923767389414861,1.),(1.00001964298269,
0.923365049627104,1.),(1.00001971973799,0.923065597204644,1.),(1.00002002011192,
0.921893721121883,1.),(1.0000203140672,0.920746886721891,1.),(1.0000210516324,
0.917869356720474,1.),(1.00002149497007,0.916139723229799,1.),(1.00002250053566,
0.912216618982122,1.),(1.00002306616987,0.910009858911181,1.),(1.00002366324673,
0.907680428794268,1.)))
REPRESENTATION_ITEM('')
SURFACE()
);
#170=(
BOUNDED_SURFACE()
B_SPLINE_SURFACE(3,2,((#29115,#29116,#29117),(#29118,#29119,#29120),(#29121,
#29122,#29123),(#29124,#29125,#29126),(#29127,#29128,#29129),(#29130,#29131,
#29132),(#29133,#29134,#29135),(#29136,#29137,#29138)),.UNSPECIFIED.,.F.,
 .F.,.F.)
B_SPLINE_SURFACE_WITH_KNOTS((4,2,2,4),(3,3),(0.0301024650456266,0.0387558943228362,
0.0430826089614409,0.0474093236000457),(0.,1.),.UNSPECIFIED.)
GEOMETRIC_REPRESENTATION_ITEM()
RATIONAL_B_SPLINE_SURFACE(((1.,0.921029907823249,1.),(1.,0.922877070064105,
1.),(1.,0.923876933766823,1.),(1.,0.92388082420723,1.),(1.,0.923630934244524,
1.),(1.,0.92266268253527,1.),(1.,0.921946472339213,1.),(1.,0.921029907823249,
1.)))
REPRESENTATION_ITEM('')
SURFACE()
);
#171=(
BOUNDED_SURFACE()
B_SPLINE_SURFACE(3,2,((#29148,#29149,#29150),(#29151,#29152,#29153),(#29154,
#29155,#29156),(#29157,#29158,#29159),(#29160,#29161,#29162),(#29163,#29164,
#29165)),.UNSPECIFIED.,.F.,.F.,.F.)
B_SPLINE_SURFACE_WITH_KNOTS((4,2,4),(3,3),(0.000862653993932655,0.00141381336854386,
0.00196497274315507),(0.,1.),.UNSPECIFIED.)
GEOMETRIC_REPRESENTATION_ITEM()
RATIONAL_B_SPLINE_SURFACE(((1.,0.707106781186548,1.),(1.,0.746708654901537,
1.),(1.,0.782505247018702,1.),(1.,0.848948022680798,1.),(1.,0.879773708616591,
1.),(1.,0.907850513789744,1.)))
REPRESENTATION_ITEM('')
SURFACE()
);
#172=(
BOUNDED_SURFACE()
B_SPLINE_SURFACE(3,2,((#29188,#29189,#29190),(#29191,#29192,#29193),(#29194,
#29195,#29196),(#29197,#29198,#29199),(#29200,#29201,#29202),(#29203,#29204,
#29205)),.UNSPECIFIED.,.F.,.F.,.F.)
B_SPLINE_SURFACE_WITH_KNOTS((4,2,4),(3,3),(0.00125184933893988,0.00239738856741524,
0.00354292779589061),(0.,1.),.UNSPECIFIED.)
GEOMETRIC_REPRESENTATION_ITEM()
RATIONAL_B_SPLINE_SURFACE(((1.,0.707106781186555,1.),(1.,0.752499298132528,
1.),(1.,0.791707406458668,1.),(1.,0.862055470547376,1.),(1.,0.893085809397505,
1.),(1.,0.9210299078221,1.)))
REPRESENTATION_ITEM('')
SURFACE()
);
#173=(
BOUNDED_SURFACE()
B_SPLINE_SURFACE(3,2,((#29229,#29230,#29231),(#29232,#29233,#29234),(#29235,
#29236,#29237),(#29238,#29239,#29240)),.UNSPECIFIED.,.F.,.F.,.F.)
B_SPLINE_SURFACE_WITH_KNOTS((4,4),(3,3),(0.306318309032005,0.312866265050619),
(0.,1.),.UNSPECIFIED.)
GEOMETRIC_REPRESENTATION_ITEM()
RATIONAL_B_SPLINE_SURFACE(((1.,0.71280418685291,1.),(1.,0.712964508138911,
1.),(1.,0.713138219728701,1.),(1.,0.713329401304078,1.)))
REPRESENTATION_ITEM('')
SURFACE()
);
#174=(
BOUNDED_SURFACE()
B_SPLINE_SURFACE(3,2,((#29271,#29272,#29273),(#29274,#29275,#29276),(#29277,
#29278,#29279),(#29280,#29281,#29282),(#29283,#29284,#29285),(#29286,#29287,
#29288)),.UNSPECIFIED.,.F.,.F.,.F.)
B_SPLINE_SURFACE_WITH_KNOTS((4,2,4),(3,3),(0.00086265399393263,0.00141381336854384,
0.00196497274315506),(0.,1.),.UNSPECIFIED.)
GEOMETRIC_REPRESENTATION_ITEM()
RATIONAL_B_SPLINE_SURFACE(((1.,0.707106781186548,1.),(1.,0.746708654901981,
1.),(1.,0.782505247018089,1.),(1.,0.84894802268141,1.),(1.,0.87977370861613,
1.),(1.,0.907850513789739,1.)))
REPRESENTATION_ITEM('')
SURFACE()
);
#175=(
BOUNDED_SURFACE()
B_SPLINE_SURFACE(3,2,((#29300,#29301,#29302),(#29303,#29304,#29305),(#29306,
#29307,#29308),(#29309,#29310,#29311),(#29312,#29313,#29314),(#29315,#29316,
#29317),(#29318,#29319,#29320),(#29321,#29322,#29323),(#29324,#29325,#29326),
(#29327,#29328,#29329),(#29330,#29331,#29332),(#29333,#29334,#29335),(#29336,
#29337,#29338),(#29339,#29340,#29341),(#29342,#29343,#29344),(#29345,#29346,
#29347),(#29348,#29349,#29350),(#29351,#29352,#29353)),.UNSPECIFIED.,.F.,
 .F.,.F.)
B_SPLINE_SURFACE_WITH_KNOTS((4,2,2,2,2,2,2,2,4),(3,3),(0.0489197875179387,
0.0601853600247889,0.0657063758111463,0.068466883704325,0.0712273915975036,
0.0822694231702183,0.085029931063397,0.0877904389565757,0.093311454742933),
(0.,1.00022354093414),.UNSPECIFIED.)
GEOMETRIC_REPRESENTATION_ITEM()
RATIONAL_B_SPLINE_SURFACE(((1.,0.907555692136622,1.00004133017387),(1.,
0.912172103881105,1.00003926625988),(1.,0.916297259384821,1.00003742197765),
(1.,0.920684838107995,1.00003546037076),(1.,0.921842485532638,1.00003494280759),
(1.,0.923032575965056,1.00003441073973),(1.,0.9233383919264,1.00003427401496),
(1.,0.923751986700875,1.00003408910424),(1.,0.923857671594793,1.00003404185444),
(1.,0.923881080297864,1.00003403138883),(1.,0.922241806174143,1.00003476427857),
(1.,0.918599911620776,1.00003639250359),(1.,0.917794373422827,1.00003675264511),
(1.,0.916066405850204,1.00003752518808),(1.,0.915142273001859,1.00003793835112),
(1.,0.912223658688977,1.00003924321066),(1.,0.910083556365492,1.00004020001161),
(1.,0.907829914607512,1.00004120757398)))
REPRESENTATION_ITEM('')
SURFACE()
);
#176=(
BOUNDED_SURFACE()
B_SPLINE_SURFACE(3,2,((#29363,#29364,#29365),(#29366,#29367,#29368),(#29369,
#29370,#29371),(#29372,#29373,#29374)),.UNSPECIFIED.,.F.,.F.,.F.)
B_SPLINE_SURFACE_WITH_KNOTS((4,4),(3,3),(0.307250934553086,0.31379889057165),
(0.,1.),.UNSPECIFIED.)
GEOMETRIC_REPRESENTATION_ITEM()
RATIONAL_B_SPLINE_SURFACE(((1.,0.712804186852904,1.),(1.,0.712964508138908,
1.),(1.,0.713138219728696,1.),(1.,0.713329401304078,1.)))
REPRESENTATION_ITEM('')
SURFACE()
);
#177=(
BOUNDED_SURFACE()
B_SPLINE_SURFACE(3,2,((#29376,#29377,#29378),(#29379,#29380,#29381),(#29382,
#29383,#29384),(#29385,#29386,#29387),(#29388,#29389,#29390),(#29391,#29392,
#29393)),.UNSPECIFIED.,.F.,.F.,.F.)
B_SPLINE_SURFACE_WITH_KNOTS((4,2,4),(3,3),(0.000678304539097038,0.00122793525694883,
0.00177756597480063),(0.,1.),.UNSPECIFIED.)
GEOMETRIC_REPRESENTATION_ITEM()
RATIONAL_B_SPLINE_SURFACE(((1.,0.70710678118654,1.),(1.,0.746184084332961,
1.),(1.,0.782509959683157,1.),(1.,0.849214842808395,1.),(1.,0.879717238316122,
1.),(1.,0.907850513788111,1.)))
REPRESENTATION_ITEM('')
SURFACE()
);
#178=(
BOUNDED_SURFACE()
B_SPLINE_SURFACE(3,2,((#29431,#29432,#29433),(#29434,#29435,#29436),(#29437,
#29438,#29439),(#29440,#29441,#29442)),.UNSPECIFIED.,.F.,.F.,.F.)
B_SPLINE_SURFACE_WITH_KNOTS((4,4),(3,3),(0.307250934553086,0.31379889057165),
(0.,1.),.UNSPECIFIED.)
GEOMETRIC_REPRESENTATION_ITEM()
RATIONAL_B_SPLINE_SURFACE(((1.,0.712804186852903,1.),(1.,0.712964508138911,
1.),(1.,0.713138219728697,1.),(1.,0.713329401304077,1.)))
REPRESENTATION_ITEM('')
SURFACE()
);
#179=(
BOUNDED_SURFACE()
B_SPLINE_SURFACE(3,2,((#31143,#31144,#31145),(#31146,#31147,#31148),(#31149,
#31150,#31151),(#31152,#31153,#31154),(#31155,#31156,#31157),(#31158,#31159,
#31160)),.UNSPECIFIED.,.F.,.F.,.F.)
B_SPLINE_SURFACE_WITH_KNOTS((4,2,4),(3,3),(0.00106076019035493,0.00169847101257237,
0.00233618183478981),(0.,1.),.UNSPECIFIED.)
GEOMETRIC_REPRESENTATION_ITEM()
RATIONAL_B_SPLINE_SURFACE(((1.,0.707106781186634,1.),(1.,0.749398144477624,
1.),(1.,0.787950893928372,1.),(1.,0.859993702049886,1.),(1.,0.893886360722003,
1.),(1.,0.923879532510764,1.)))
REPRESENTATION_ITEM('')
SURFACE()
);
#180=(
BOUNDED_SURFACE()
B_SPLINE_SURFACE(3,2,((#31184,#31185,#31186),(#31187,#31188,#31189),(#31190,
#31191,#31192),(#31193,#31194,#31195),(#31196,#31197,#31198),(#31199,#31200,
#31201)),.UNSPECIFIED.,.F.,.F.,.F.)
B_SPLINE_SURFACE_WITH_KNOTS((4,2,4),(3,3),(0.000793141102904165,0.00155796281789264,
0.00232278453288111),(-0.000567486199232424,1.),.UNSPECIFIED.)
GEOMETRIC_REPRESENTATION_ITEM()
RATIONAL_B_SPLINE_SURFACE(((1.0003619027993,0.681135153781566,1.),(1.0003023133926,
0.733638110485494,1.),(1.00024889602588,0.780703014258753,1.),(1.00015092061996,
0.867027057078915,1.),(1.00010588522079,0.906706787818273,1.),(1.00006613376639,
0.941730947393786,1.)))
REPRESENTATION_ITEM('')
SURFACE()
);
#181=(
BOUNDED_SURFACE()
B_SPLINE_SURFACE(3,2,((#31225,#31226,#31227),(#31228,#31229,#31230),(#31231,
#31232,#31233),(#31234,#31235,#31236),(#31237,#31238,#31239),(#31240,#31241,
#31242),(#31243,#31244,#31245),(#31246,#31247,#31248)),.UNSPECIFIED.,.F.,
 .F.,.F.)
B_SPLINE_SURFACE_WITH_KNOTS((4,2,2,4),(3,3),(0.0113699589602356,0.0215499319036472,
0.0263330282216041,0.031727010144494),(0.,1.00072721389233),
 .UNSPECIFIED.)
GEOMETRIC_REPRESENTATION_ITEM()
RATIONAL_B_SPLINE_SURFACE(((0.999999999999999,0.904674950757355,1.00013864340019),
(1.,0.909119912835753,1.00013217852384),(1.,0.913289332689208,1.00012611440376),
(1.,0.918180475671682,1.00011900058951),(1.,0.91955733112885,1.00011699805268),
(1.,0.92190730676968,1.00011358018281),(1.,0.922815134510754,1.00011225981292),
(1.,0.923326705446227,1.00011151576994)))
REPRESENTATION_ITEM('')
SURFACE()
);
#182=(
BOUNDED_SURFACE()
B_SPLINE_SURFACE(3,2,((#31249,#31250,#31251),(#31252,#31253,#31254),(#31255,
#31256,#31257),(#31258,#31259,#31260),(#31261,#31262,#31263),(#31264,#31265,
#31266),(#31267,#31268,#31269),(#31270,#31271,#31272)),.UNSPECIFIED.,.F.,
 .F.,.F.)
B_SPLINE_SURFACE_WITH_KNOTS((4,2,2,4),(3,3),(0.0119004725603816,0.0216177878121986,
0.0264008481563397,0.0313322083477393),(-0.000264627279374309,1.),
 .UNSPECIFIED.)
GEOMETRIC_REPRESENTATION_ITEM()
RATIONAL_B_SPLINE_SURFACE(((1.00005010827284,0.90532292634548,1.),(1.00004787696662,
0.909538867776431,1.),(1.0000457907739,0.913480624500144,1.),(1.0000432831544,
0.918218646038307,1.),(1.00004255484361,0.919594752826323,1.),(1.00004136830048,
0.921836666698683,1.),(1.00004091524432,0.922692693631796,1.),(1.0000406351647,
0.923221890052849,1.)))
REPRESENTATION_ITEM('')
SURFACE()
);
#183=(
BOUNDED_SURFACE()
B_SPLINE_SURFACE(3,2,((#31405,#31406,#31407),(#31408,#31409,#31410),(#31411,
#31412,#31413),(#31414,#31415,#31416),(#31417,#31418,#31419),(#31420,#31421,
#31422)),.UNSPECIFIED.,.F.,.F.,.F.)
B_SPLINE_SURFACE_WITH_KNOTS((4,2,4),(3,3),(0.000848991610552184,0.00148839833350338,
0.00212780505645457),(0.,1.),.UNSPECIFIED.)
GEOMETRIC_REPRESENTATION_ITEM()
RATIONAL_B_SPLINE_SURFACE(((1.,0.707106781186638,1.),(1.,0.749413725208667,
1.),(1.,0.788293333703998,1.),(1.,0.860148103423894,1.),(1.,0.893310888592562,
1.),(1.,0.923879532511264,1.)))
REPRESENTATION_ITEM('')
SURFACE()
);
#184=(
BOUNDED_SURFACE()
B_SPLINE_SURFACE(3,2,((#31448,#31449,#31450),(#31451,#31452,#31453),(#31454,
#31455,#31456),(#31457,#31458,#31459),(#31460,#31461,#31462),(#31463,#31464,
#31465)),.UNSPECIFIED.,.F.,.F.,.F.)
B_SPLINE_SURFACE_WITH_KNOTS((4,2,4),(3,3),(0.00106076019035492,0.00169895425208248,
0.00233714831381003),(0.,1.),.UNSPECIFIED.)
GEOMETRIC_REPRESENTATION_ITEM()
RATIONAL_B_SPLINE_SURFACE(((1.,0.707106781186618,1.),(1.,0.749428557966193,
1.),(1.,0.787940856472646,1.),(1.,0.859781915358774,1.),(1.,0.893307888347381,
1.),(1.,0.923879532511264,1.)))
REPRESENTATION_ITEM('')
SURFACE()
);
#185=(
BOUNDED_SURFACE()
B_SPLINE_SURFACE(3,2,((#31489,#31490,#31491),(#31492,#31493,#31494),(#31495,
#31496,#31497),(#31498,#31499,#31500),(#31501,#31502,#31503),(#31504,#31505,
#31506)),.UNSPECIFIED.,.F.,.F.,.F.)
B_SPLINE_SURFACE_WITH_KNOTS((4,2,4),(3,3),(0.00106076019035499,0.00169856943267974,
0.00233637867500449),(0.,1.),.UNSPECIFIED.)
GEOMETRIC_REPRESENTATION_ITEM()
RATIONAL_B_SPLINE_SURFACE(((1.,0.707106781186626,1.),(1.,0.749404516349508,
1.),(1.,0.787956723757177,1.),(1.,0.859986866015709,1.),(1.,0.893873946401784,
1.),(1.,0.923879532510069,1.)))
REPRESENTATION_ITEM('')
SURFACE()
);
#186=(
BOUNDED_SURFACE()
B_SPLINE_SURFACE(3,2,((#31530,#31531,#31532),(#31533,#31534,#31535),(#31536,
#31537,#31538),(#31539,#31540,#31541),(#31542,#31543,#31544),(#31545,#31546,
#31547),(#31548,#31549,#31550),(#31551,#31552,#31553)),.UNSPECIFIED.,.F.,
 .F.,.F.)
B_SPLINE_SURFACE_WITH_KNOTS((4,2,2,4),(3,3),(0.0119004725412382,0.0216177878121984,
0.0264008481563395,0.0313322083668821),(-0.000264627298517322,1.),
 .UNSPECIFIED.)
GEOMETRIC_REPRESENTATION_ITEM()
RATIONAL_B_SPLINE_SURFACE(((1.00005010827648,0.905322926318752,1.),(1.00004787697009,
0.90953886775917,1.),(1.00004579077722,0.913480624492233,1.),(1.00004328315754,
0.918218646036742,1.),(1.00004255484669,0.919594752824784,1.),(1.00004136830347,
0.921836666701605,1.),(1.00004091524728,0.922692693636962,1.),(1.00004063516764,
0.923221890057542,1.)))
REPRESENTATION_ITEM('')
SURFACE()
);
#187=(
BOUNDED_SURFACE()
B_SPLINE_SURFACE(3,2,((#31556,#31557,#31558),(#31559,#31560,#31561),(#31562,
#31563,#31564),(#31565,#31566,#31567),(#31568,#31569,#31570),(#31571,#31572,
#31573),(#31574,#31575,#31576),(#31577,#31578,#31579)),.UNSPECIFIED.,.F.,
 .F.,.F.)
B_SPLINE_SURFACE_WITH_KNOTS((4,2,2,4),(3,3),(0.0113699590143702,0.0215499319036474,
0.0263330282216043,0.0317270100903599),(0.,1.0007272138382),
 .UNSPECIFIED.)
GEOMETRIC_REPRESENTATION_ITEM()
RATIONAL_B_SPLINE_SURFACE(((1.,0.904674950833136,1.00013864338976),(1.,
0.9091199128866,1.00013217851393),(1.,0.913289332709887,1.00012611439435),
(1.,0.918180475676915,1.00011900058065),(1.,0.91955733113338,1.00011699804396),
(1.,0.921907306761203,1.00011358017437),(1.,0.922815134496923,1.00011225980459),
(1.,0.923326705434899,1.00011151576166)))
REPRESENTATION_ITEM('')
SURFACE()
);
#188=(
BOUNDED_SURFACE()
B_SPLINE_SURFACE(3,2,((#31580,#31581,#31582),(#31583,#31584,#31585),(#31586,
#31587,#31588),(#31589,#31590,#31591),(#31592,#31593,#31594),(#31595,#31596,
#31597),(#31598,#31599,#31600),(#31601,#31602,#31603)),.UNSPECIFIED.,.F.,
 .F.,.F.)
B_SPLINE_SURFACE_WITH_KNOTS((4,2,2,4),(3,3),(0.0119004725305903,0.0216177878121981,
0.0264008481563393,0.0313322083775296),(-0.000264627309164933,1.),
 .UNSPECIFIED.)
GEOMETRIC_REPRESENTATION_ITEM()
RATIONAL_B_SPLINE_SURFACE(((1.0000501082785,0.905322926303854,1.),(1.00004787697202,
0.909538867750149,1.),(1.00004579077906,0.913480624487108,1.),(1.00004328315928,
0.918218646036229,1.),(1.00004255484841,0.919594752823839,1.),(1.00004136830513,
0.921836666703322,1.),(1.00004091524892,0.922692693639759,1.),(1.00004063516927,
0.92322189006016,1.)))
REPRESENTATION_ITEM('')
SURFACE()
);
#189=(
BOUNDED_SURFACE()
B_SPLINE_SURFACE(3,2,((#31614,#31615,#31616),(#31617,#31618,#31619),(#31620,
#31621,#31622),(#31623,#31624,#31625),(#31626,#31627,#31628),(#31629,#31630,
#31631),(#31632,#31633,#31634),(#31635,#31636,#31637)),.UNSPECIFIED.,.F.,
 .F.,.F.)
B_SPLINE_SURFACE_WITH_KNOTS((4,2,2,4),(3,3),(0.0113699590001087,0.0215499319036469,
0.0263330282216038,0.0317270101046203),(0.,1.00072721385246),
 .UNSPECIFIED.)
GEOMETRIC_REPRESENTATION_ITEM()
RATIONAL_B_SPLINE_SURFACE(((1.,0.904674950813353,1.00013864339251),(1.,
0.909119912872212,1.00013217851654),(1.,0.913289332705507,1.00012611439682),
(1.,0.918180475675032,1.00011900058298),(1.,0.919557331132055,1.00011699804626),
(1.,0.921907306763585,1.00011358017659),(1.,0.922815134500407,1.00011225980678),
(1.,0.923326705437937,1.00011151576384)))
REPRESENTATION_ITEM('')
SURFACE()
);
#190=(
BOUNDED_SURFACE()
B_SPLINE_SURFACE(3,2,((#31840,#31841,#31842),(#31843,#31844,#31845),(#31846,
#31847,#31848),(#31849,#31850,#31851),(#31852,#31853,#31854),(#31855,#31856,
#31857)),.UNSPECIFIED.,.F.,.F.,.F.)
B_SPLINE_SURFACE_WITH_KNOTS((4,2,4),(3,3),(0.000793141102904163,0.00155796281789264,
0.00232278453288111),(-0.000567486199155168,1.),.UNSPECIFIED.)
GEOMETRIC_REPRESENTATION_ITEM()
RATIONAL_B_SPLINE_SURFACE(((1.00036190279925,0.681135153781591,1.),(1.00030231339256,
0.733638110485514,1.),(1.00024889602585,0.78070301425877,1.),(1.00015092061994,
0.867027057078926,1.),(1.00010588522078,0.90670678781828,1.),(1.00006613376638,
0.941730947393792,1.)))
REPRESENTATION_ITEM('')
SURFACE()
);
#191=(
BOUNDED_SURFACE()
B_SPLINE_SURFACE(3,2,((#31881,#31882,#31883),(#31884,#31885,#31886),(#31887,
#31888,#31889),(#31890,#31891,#31892),(#31893,#31894,#31895),(#31896,#31897,
#31898)),.UNSPECIFIED.,.F.,.F.,.F.)
B_SPLINE_SURFACE_WITH_KNOTS((4,2,4),(3,3),(0.000885251653512216,0.00152482279265937,
0.00216439393180653),(0.,1.),.UNSPECIFIED.)
GEOMETRIC_REPRESENTATION_ITEM()
RATIONAL_B_SPLINE_SURFACE(((1.,0.70710678118663,1.),(1.,0.749482754810037,
1.),(1.,0.788287146221274,1.),(1.,0.860112372061843,1.),(1.,0.893279480387377,
1.),(1.,0.923879532511264,1.)))
REPRESENTATION_ITEM('')
SURFACE()
);
#192=(
BOUNDED_SURFACE()
B_SPLINE_SURFACE(3,2,((#31902,#31903,#31904),(#31905,#31906,#31907),(#31908,
#31909,#31910),(#31911,#31912,#31913),(#31914,#31915,#31916),(#31917,#31918,
#31919),(#31920,#31921,#31922),(#31923,#31924,#31925)),.UNSPECIFIED.,.F.,
 .F.,.F.)
B_SPLINE_SURFACE_WITH_KNOTS((4,2,2,4),(3,3),(0.0113699589780933,0.0215499319036469,
0.0263330282216038,0.0317270101266359),(0.,1.00072721387447),
 .UNSPECIFIED.)
GEOMETRIC_REPRESENTATION_ITEM()
RATIONAL_B_SPLINE_SURFACE(((1.,0.904674950782418,1.00013864339675),(1.,
0.909119912852179,1.00013217852057),(1.,0.913289332696403,1.00012611440066),
(1.,0.918180475673232,1.00011900058659),(1.,0.919557331130196,1.0001169980498),
(1.,0.921907306767051,1.00011358018003),(1.,0.922815134506009,1.00011225981017),
(1.,0.923326705442552,1.00011151576721)))
REPRESENTATION_ITEM('')
SURFACE()
);
#193=(
BOUNDED_SURFACE()
B_SPLINE_SURFACE(3,2,((#31979,#31980,#31981),(#31982,#31983,#31984),(#31985,
#31986,#31987),(#31988,#31989,#31990),(#31991,#31992,#31993),(#31994,#31995,
#31996)),.UNSPECIFIED.,.F.,.F.,.F.)
B_SPLINE_SURFACE_WITH_KNOTS((4,2,4),(3,3),(0.00106076019035493,0.00169847101257236,
0.0023361818347898),(0.,1.),.UNSPECIFIED.)
GEOMETRIC_REPRESENTATION_ITEM()
RATIONAL_B_SPLINE_SURFACE(((1.,0.707106781186638,1.),(1.,0.749398144477821,
1.),(1.,0.787950893928113,1.),(1.,0.859993702050145,1.),(1.,0.893886360721809,
1.),(1.,0.923879532510763,1.)))
REPRESENTATION_ITEM('')
SURFACE()
);
#194=(
BOUNDED_SURFACE()
B_SPLINE_SURFACE(3,2,((#32019,#32020,#32021),(#32022,#32023,#32024),(#32025,
#32026,#32027),(#32028,#32029,#32030),(#32031,#32032,#32033),(#32034,#32035,
#32036),(#32037,#32038,#32039),(#32040,#32041,#32042)),.UNSPECIFIED.,.F.,
 .F.,.F.)
B_SPLINE_SURFACE_WITH_KNOTS((4,2,2,4),(3,3),(0.0119004725361997,0.0216177878121993,
0.0264008481563403,0.0313322083719226),(-0.000264627303556973,1.),
 .UNSPECIFIED.)
GEOMETRIC_REPRESENTATION_ITEM()
RATIONAL_B_SPLINE_SURFACE(((1.00005010827744,0.905322926311723,1.),(1.00004787697101,
0.909538867754481,1.),(1.00004579077809,0.913480624490332,1.),(1.00004328315836,
0.918218646036241,1.),(1.0000425548475,0.919594752824379,1.),(1.00004136830425,
0.921836666702374,1.),(1.00004091524806,0.922692693638322,1.),(1.00004063516841,
0.923221890058778,1.)))
REPRESENTATION_ITEM('')
SURFACE()
);
#195=B_SPLINE_SURFACE_WITH_KNOTS('',3,3,((#22254,#22255,#22256,#22257,#22258,
#22259,#22260,#22261,#22262,#22263),(#22264,#22265,#22266,#22267,#22268,
#22269,#22270,#22271,#22272,#22273),(#22274,#22275,#22276,#22277,#22278,
#22279,#22280,#22281,#22282,#22283),(#22284,#22285,#22286,#22287,#22288,
#22289,#22290,#22291,#22292,#22293),(#22294,#22295,#22296,#22297,#22298,
#22299,#22300,#22301,#22302,#22303),(#22304,#22305,#22306,#22307,#22308,
#22309,#22310,#22311,#22312,#22313)),.UNSPECIFIED.,.F.,.F.,.F.,(4,2,4),
(4,2,2,2,4),(0.,0.5,1.),(0.,0.25,0.5,0.75,1.),.UNSPECIFIED.);
#196=B_SPLINE_SURFACE_WITH_KNOTS('',3,3,((#22344,#22345,#22346,#22347,#22348,
#22349,#22350,#22351),(#22352,#22353,#22354,#22355,#22356,#22357,#22358,
#22359),(#22360,#22361,#22362,#22363,#22364,#22365,#22366,#22367),(#22368,
#22369,#22370,#22371,#22372,#22373,#22374,#22375),(#22376,#22377,#22378,
#22379,#22380,#22381,#22382,#22383),(#22384,#22385,#22386,#22387,#22388,
#22389,#22390,#22391),(#22392,#22393,#22394,#22395,#22396,#22397,#22398,
#22399),(#22400,#22401,#22402,#22403,#22404,#22405,#22406,#22407)),
 .UNSPECIFIED.,.F.,.F.,.F.,(4,2,2,4),(4,2,2,4),(0.,0.25,0.5,1.),(0.,0.25,
0.5,1.),.UNSPECIFIED.);
#197=B_SPLINE_SURFACE_WITH_KNOTS('',3,3,((#22425,#22426,#22427,#22428,#22429,
#22430),(#22431,#22432,#22433,#22434,#22435,#22436),(#22437,#22438,#22439,
#22440,#22441,#22442),(#22443,#22444,#22445,#22446,#22447,#22448),(#22449,
#22450,#22451,#22452,#22453,#22454),(#22455,#22456,#22457,#22458,#22459,
#22460),(#22461,#22462,#22463,#22464,#22465,#22466),(#22467,#22468,#22469,
#22470,#22471,#22472)),.UNSPECIFIED.,.F.,.F.,.F.,(4,2,2,4),(4,2,4),(0.,
0.25,0.5,1.),(0.,0.5,1.),.UNSPECIFIED.);
#198=B_SPLINE_SURFACE_WITH_KNOTS('',3,3,((#22495,#22496,#22497,#22498,#22499,
#22500,#22501,#22502),(#22503,#22504,#22505,#22506,#22507,#22508,#22509,
#22510),(#22511,#22512,#22513,#22514,#22515,#22516,#22517,#22518),(#22519,
#22520,#22521,#22522,#22523,#22524,#22525,#22526),(#22527,#22528,#22529,
#22530,#22531,#22532,#22533,#22534),(#22535,#22536,#22537,#22538,#22539,
#22540,#22541,#22542)),.UNSPECIFIED.,.F.,.F.,.F.,(4,2,4),(4,2,2,4),(0.,
0.5,1.),(0.,0.25,0.5,1.),.UNSPECIFIED.);
#199=B_SPLINE_SURFACE_WITH_KNOTS('',3,3,((#22566,#22567,#22568,#22569,#22570,
#22571,#22572,#22573),(#22574,#22575,#22576,#22577,#22578,#22579,#22580,
#22581),(#22582,#22583,#22584,#22585,#22586,#22587,#22588,#22589),(#22590,
#22591,#22592,#22593,#22594,#22595,#22596,#22597),(#22598,#22599,#22600,
#22601,#22602,#22603,#22604,#22605),(#22606,#22607,#22608,#22609,#22610,
#22611,#22612,#22613),(#22614,#22615,#22616,#22617,#22618,#22619,#22620,
#22621),(#22622,#22623,#22624,#22625,#22626,#22627,#22628,#22629)),
 .UNSPECIFIED.,.F.,.F.,.F.,(4,2,2,4),(4,2,2,4),(0.,0.25,0.5,1.),(0.,0.25,
0.5,1.),.UNSPECIFIED.);
#200=B_SPLINE_SURFACE_WITH_KNOTS('',3,3,((#22698,#22699,#22700,#22701,#22702,
#22703),(#22704,#22705,#22706,#22707,#22708,#22709),(#22710,#22711,#22712,
#22713,#22714,#22715),(#22716,#22717,#22718,#22719,#22720,#22721),(#22722,
#22723,#22724,#22725,#22726,#22727),(#22728,#22729,#22730,#22731,#22732,
#22733),(#22734,#22735,#22736,#22737,#22738,#22739),(#22740,#22741,#22742,
#22743,#22744,#22745)),.UNSPECIFIED.,.F.,.F.,.F.,(4,2,2,4),(4,2,4),(0.,
0.25,0.5,1.),(0.,0.5,1.),.UNSPECIFIED.);
#201=B_SPLINE_SURFACE_WITH_KNOTS('',3,3,((#22776,#22777,#22778,#22779,#22780,
#22781,#22782,#22783),(#22784,#22785,#22786,#22787,#22788,#22789,#22790,
#22791),(#22792,#22793,#22794,#22795,#22796,#22797,#22798,#22799),(#22800,
#22801,#22802,#22803,#22804,#22805,#22806,#22807),(#22808,#22809,#22810,
#22811,#22812,#22813,#22814,#22815),(#22816,#22817,#22818,#22819,#22820,
#22821,#22822,#22823)),.UNSPECIFIED.,.F.,.F.,.F.,(4,2,4),(4,2,2,4),(0.,
0.5,1.),(0.,0.25,0.5,1.),.UNSPECIFIED.);
#202=B_SPLINE_SURFACE_WITH_KNOTS('',3,3,((#22847,#22848,#22849,#22850,#22851,
#22852,#22853,#22854),(#22855,#22856,#22857,#22858,#22859,#22860,#22861,
#22862),(#22863,#22864,#22865,#22866,#22867,#22868,#22869,#22870),(#22871,
#22872,#22873,#22874,#22875,#22876,#22877,#22878),(#22879,#22880,#22881,
#22882,#22883,#22884,#22885,#22886),(#22887,#22888,#22889,#22890,#22891,
#22892,#22893,#22894),(#22895,#22896,#22897,#22898,#22899,#22900,#22901,
#22902),(#22903,#22904,#22905,#22906,#22907,#22908,#22909,#22910)),
 .UNSPECIFIED.,.F.,.F.,.F.,(4,2,2,4),(4,2,2,4),(0.,0.25,0.5,1.),(0.,0.25,
0.5,1.),.UNSPECIFIED.);
#203=B_SPLINE_SURFACE_WITH_KNOTS('',3,3,((#22928,#22929,#22930,#22931,#22932,
#22933),(#22934,#22935,#22936,#22937,#22938,#22939),(#22940,#22941,#22942,
#22943,#22944,#22945),(#22946,#22947,#22948,#22949,#22950,#22951),(#22952,
#22953,#22954,#22955,#22956,#22957),(#22958,#22959,#22960,#22961,#22962,
#22963),(#22964,#22965,#22966,#22967,#22968,#22969),(#22970,#22971,#22972,
#22973,#22974,#22975),(#22976,#22977,#22978,#22979,#22980,#22981),(#22982,
#22983,#22984,#22985,#22986,#22987)),.UNSPECIFIED.,.F.,.F.,.F.,(4,2,2,2,
4),(4,2,4),(0.,0.25,0.5,0.75,1.),(0.,0.5,1.),.UNSPECIFIED.);
#204=B_SPLINE_SURFACE_WITH_KNOTS('',3,3,((#23007,#23008,#23009,#23010,#23011,
#23012,#23013,#23014,#23015,#23016),(#23017,#23018,#23019,#23020,#23021,
#23022,#23023,#23024,#23025,#23026),(#23027,#23028,#23029,#23030,#23031,
#23032,#23033,#23034,#23035,#23036),(#23037,#23038,#23039,#23040,#23041,
#23042,#23043,#23044,#23045,#23046),(#23047,#23048,#23049,#23050,#23051,
#23052,#23053,#23054,#23055,#23056),(#23057,#23058,#23059,#23060,#23061,
#23062,#23063,#23064,#23065,#23066)),.UNSPECIFIED.,.F.,.F.,.F.,(4,2,4),
(4,2,2,2,4),(0.,0.5,1.),(0.,0.25,0.5,0.75,1.),.UNSPECIFIED.);
#205=B_SPLINE_SURFACE_WITH_KNOTS('',3,3,((#23075,#23076,#23077,#23078,#23079,
#23080,#23081,#23082,#23083,#23084),(#23085,#23086,#23087,#23088,#23089,
#23090,#23091,#23092,#23093,#23094),(#23095,#23096,#23097,#23098,#23099,
#23100,#23101,#23102,#23103,#23104),(#23105,#23106,#23107,#23108,#23109,
#23110,#23111,#23112,#23113,#23114),(#23115,#23116,#23117,#23118,#23119,
#23120,#23121,#23122,#23123,#23124),(#23125,#23126,#23127,#23128,#23129,
#23130,#23131,#23132,#23133,#23134)),.UNSPECIFIED.,.F.,.F.,.F.,(4,2,4),
(4,2,2,2,4),(0.,0.5,1.),(0.,0.25,0.5,0.75,1.),.UNSPECIFIED.);
#206=B_SPLINE_SURFACE_WITH_KNOTS('',3,3,((#23165,#23166,#23167,#23168,#23169,
#23170,#23171,#23172),(#23173,#23174,#23175,#23176,#23177,#23178,#23179,
#23180),(#23181,#23182,#23183,#23184,#23185,#23186,#23187,#23188),(#23189,
#23190,#23191,#23192,#23193,#23194,#23195,#23196),(#23197,#23198,#23199,
#23200,#23201,#23202,#23203,#23204),(#23205,#23206,#23207,#23208,#23209,
#23210,#23211,#23212),(#23213,#23214,#23215,#23216,#23217,#23218,#23219,
#23220),(#23221,#23222,#23223,#23224,#23225,#23226,#23227,#23228)),
 .UNSPECIFIED.,.F.,.F.,.F.,(4,2,2,4),(4,2,2,4),(0.,0.25,0.5,1.),(0.,0.25,
0.5,1.),.UNSPECIFIED.);
#207=B_SPLINE_SURFACE_WITH_KNOTS('',3,3,((#23246,#23247,#23248,#23249,#23250,
#23251),(#23252,#23253,#23254,#23255,#23256,#23257),(#23258,#23259,#23260,
#23261,#23262,#23263),(#23264,#23265,#23266,#23267,#23268,#23269),(#23270,
#23271,#23272,#23273,#23274,#23275),(#23276,#23277,#23278,#23279,#23280,
#23281),(#23282,#23283,#23284,#23285,#23286,#23287),(#23288,#23289,#23290,
#23291,#23292,#23293)),.UNSPECIFIED.,.F.,.F.,.F.,(4,2,2,4),(4,2,4),(0.,
0.25,0.5,1.),(0.,0.5,1.),.UNSPECIFIED.);
#208=B_SPLINE_SURFACE_WITH_KNOTS('',3,3,((#23316,#23317,#23318,#23319,#23320,
#23321,#23322,#23323),(#23324,#23325,#23326,#23327,#23328,#23329,#23330,
#23331),(#23332,#23333,#23334,#23335,#23336,#23337,#23338,#23339),(#23340,
#23341,#23342,#23343,#23344,#23345,#23346,#23347),(#23348,#23349,#23350,
#23351,#23352,#23353,#23354,#23355),(#23356,#23357,#23358,#23359,#23360,
#23361,#23362,#23363)),.UNSPECIFIED.,.F.,.F.,.F.,(4,2,4),(4,2,2,4),(0.,
0.5,1.),(0.,0.25,0.5,1.),.UNSPECIFIED.);
#209=B_SPLINE_SURFACE_WITH_KNOTS('',3,3,((#23387,#23388,#23389,#23390,#23391,
#23392,#23393,#23394),(#23395,#23396,#23397,#23398,#23399,#23400,#23401,
#23402),(#23403,#23404,#23405,#23406,#23407,#23408,#23409,#23410),(#23411,
#23412,#23413,#23414,#23415,#23416,#23417,#23418),(#23419,#23420,#23421,
#23422,#23423,#23424,#23425,#23426),(#23427,#23428,#23429,#23430,#23431,
#23432,#23433,#23434),(#23435,#23436,#23437,#23438,#23439,#23440,#23441,
#23442),(#23443,#23444,#23445,#23446,#23447,#23448,#23449,#23450)),
 .UNSPECIFIED.,.F.,.F.,.F.,(4,2,2,4),(4,2,2,4),(0.,0.25,0.5,1.),(0.,0.25,
0.5,1.),.UNSPECIFIED.);
#210=B_SPLINE_SURFACE_WITH_KNOTS('',3,3,((#23519,#23520,#23521,#23522,#23523,
#23524),(#23525,#23526,#23527,#23528,#23529,#23530),(#23531,#23532,#23533,
#23534,#23535,#23536),(#23537,#23538,#23539,#23540,#23541,#23542),(#23543,
#23544,#23545,#23546,#23547,#23548),(#23549,#23550,#23551,#23552,#23553,
#23554),(#23555,#23556,#23557,#23558,#23559,#23560),(#23561,#23562,#23563,
#23564,#23565,#23566)),.UNSPECIFIED.,.F.,.F.,.F.,(4,2,2,4),(4,2,4),(0.,
0.25,0.5,1.),(0.,0.5,1.),.UNSPECIFIED.);
#211=B_SPLINE_SURFACE_WITH_KNOTS('',3,3,((#23597,#23598,#23599,#23600,#23601,
#23602,#23603,#23604),(#23605,#23606,#23607,#23608,#23609,#23610,#23611,
#23612),(#23613,#23614,#23615,#23616,#23617,#23618,#23619,#23620),(#23621,
#23622,#23623,#23624,#23625,#23626,#23627,#23628),(#23629,#23630,#23631,
#23632,#23633,#23634,#23635,#23636),(#23637,#23638,#23639,#23640,#23641,
#23642,#23643,#23644)),.UNSPECIFIED.,.F.,.F.,.F.,(4,2,4),(4,2,2,4),(0.,
0.5,1.),(0.,0.25,0.5,1.),.UNSPECIFIED.);
#212=B_SPLINE_SURFACE_WITH_KNOTS('',3,3,((#23668,#23669,#23670,#23671,#23672,
#23673,#23674,#23675),(#23676,#23677,#23678,#23679,#23680,#23681,#23682,
#23683),(#23684,#23685,#23686,#23687,#23688,#23689,#23690,#23691),(#23692,
#23693,#23694,#23695,#23696,#23697,#23698,#23699),(#23700,#23701,#23702,
#23703,#23704,#23705,#23706,#23707),(#23708,#23709,#23710,#23711,#23712,
#23713,#23714,#23715),(#23716,#23717,#23718,#23719,#23720,#23721,#23722,
#23723),(#23724,#23725,#23726,#23727,#23728,#23729,#23730,#23731)),
 .UNSPECIFIED.,.F.,.F.,.F.,(4,2,2,4),(4,2,2,4),(0.,0.25,0.5,1.),(0.,0.25,
0.5,1.),.UNSPECIFIED.);
#213=B_SPLINE_SURFACE_WITH_KNOTS('',3,3,((#23749,#23750,#23751,#23752,#23753,
#23754),(#23755,#23756,#23757,#23758,#23759,#23760),(#23761,#23762,#23763,
#23764,#23765,#23766),(#23767,#23768,#23769,#23770,#23771,#23772),(#23773,
#23774,#23775,#23776,#23777,#23778),(#23779,#23780,#23781,#23782,#23783,
#23784),(#23785,#23786,#23787,#23788,#23789,#23790),(#23791,#23792,#23793,
#23794,#23795,#23796),(#23797,#23798,#23799,#23800,#23801,#23802),(#23803,
#23804,#23805,#23806,#23807,#23808)),.UNSPECIFIED.,.F.,.F.,.F.,(4,2,2,2,
4),(4,2,4),(0.,0.25,0.5,0.75,1.),(0.,0.5,1.),.UNSPECIFIED.);
#214=B_SPLINE_SURFACE_WITH_KNOTS('',3,3,((#23828,#23829,#23830,#23831,#23832,
#23833,#23834,#23835,#23836,#23837),(#23838,#23839,#23840,#23841,#23842,
#23843,#23844,#23845,#23846,#23847),(#23848,#23849,#23850,#23851,#23852,
#23853,#23854,#23855,#23856,#23857),(#23858,#23859,#23860,#23861,#23862,
#23863,#23864,#23865,#23866,#23867),(#23868,#23869,#23870,#23871,#23872,
#23873,#23874,#23875,#23876,#23877),(#23878,#23879,#23880,#23881,#23882,
#23883,#23884,#23885,#23886,#23887)),.UNSPECIFIED.,.F.,.F.,.F.,(4,2,4),
(4,2,2,2,4),(0.,0.5,1.),(0.,0.25,0.5,0.75,1.),.UNSPECIFIED.);
#215=B_SPLINE_SURFACE_WITH_KNOTS('',3,3,((#24322,#24323,#24324,#24325,#24326,
#24327,#24328,#24329),(#24330,#24331,#24332,#24333,#24334,#24335,#24336,
#24337),(#24338,#24339,#24340,#24341,#24342,#24343,#24344,#24345),(#24346,
#24347,#24348,#24349,#24350,#24351,#24352,#24353),(#24354,#24355,#24356,
#24357,#24358,#24359,#24360,#24361),(#24362,#24363,#24364,#24365,#24366,
#24367,#24368,#24369),(#24370,#24371,#24372,#24373,#24374,#24375,#24376,
#24377),(#24378,#24379,#24380,#24381,#24382,#24383,#24384,#24385)),
 .UNSPECIFIED.,.F.,.F.,.F.,(4,2,2,4),(4,2,2,4),(0.,0.25,0.5,1.),(0.,0.25,
0.5,1.),.UNSPECIFIED.);
#216=B_SPLINE_SURFACE_WITH_KNOTS('',3,3,((#25176,#25177,#25178,#25179,#25180,
#25181),(#25182,#25183,#25184,#25185,#25186,#25187),(#25188,#25189,#25190,
#25191,#25192,#25193),(#25194,#25195,#25196,#25197,#25198,#25199),(#25200,
#25201,#25202,#25203,#25204,#25205),(#25206,#25207,#25208,#25209,#25210,
#25211),(#25212,#25213,#25214,#25215,#25216,#25217),(#25218,#25219,#25220,
#25221,#25222,#25223),(#25224,#25225,#25226,#25227,#25228,#25229),(#25230,
#25231,#25232,#25233,#25234,#25235)),.UNSPECIFIED.,.F.,.F.,.F.,(4,2,2,2,
4),(4,2,4),(0.,0.25,0.5,0.75,1.),(0.,0.5,1.),.UNSPECIFIED.);
#217=B_SPLINE_SURFACE_WITH_KNOTS('',3,3,((#26187,#26188,#26189,#26190,#26191,
#26192,#26193,#26194),(#26195,#26196,#26197,#26198,#26199,#26200,#26201,
#26202),(#26203,#26204,#26205,#26206,#26207,#26208,#26209,#26210),(#26211,
#26212,#26213,#26214,#26215,#26216,#26217,#26218),(#26219,#26220,#26221,
#26222,#26223,#26224,#26225,#26226),(#26227,#26228,#26229,#26230,#26231,
#26232,#26233,#26234),(#26235,#26236,#26237,#26238,#26239,#26240,#26241,
#26242),(#26243,#26244,#26245,#26246,#26247,#26248,#26249,#26250)),
 .UNSPECIFIED.,.F.,.F.,.F.,(4,2,2,4),(4,2,2,4),(0.,0.25,0.5,1.),(0.,0.25,
0.5,1.),.UNSPECIFIED.);
#218=B_SPLINE_SURFACE_WITH_KNOTS('',3,3,((#27764,#27765,#27766,#27767,#27768,
#27769),(#27770,#27771,#27772,#27773,#27774,#27775),(#27776,#27777,#27778,
#27779,#27780,#27781),(#27782,#27783,#27784,#27785,#27786,#27787),(#27788,
#27789,#27790,#27791,#27792,#27793),(#27794,#27795,#27796,#27797,#27798,
#27799),(#27800,#27801,#27802,#27803,#27804,#27805),(#27806,#27807,#27808,
#27809,#27810,#27811),(#27812,#27813,#27814,#27815,#27816,#27817),(#27818,
#27819,#27820,#27821,#27822,#27823)),.UNSPECIFIED.,.F.,.F.,.F.,(4,2,2,2,
4),(4,2,4),(0.,0.25,0.5,0.75,1.),(0.,0.5,1.),.UNSPECIFIED.);
#219=B_SPLINE_SURFACE_WITH_KNOTS('',3,3,((#29443,#29444,#29445,#29446,#29447,
#29448,#29449,#29450),(#29451,#29452,#29453,#29454,#29455,#29456,#29457,
#29458),(#29459,#29460,#29461,#29462,#29463,#29464,#29465,#29466),(#29467,
#29468,#29469,#29470,#29471,#29472,#29473,#29474),(#29475,#29476,#29477,
#29478,#29479,#29480,#29481,#29482),(#29483,#29484,#29485,#29486,#29487,
#29488,#29489,#29490)),.UNSPECIFIED.,.F.,.F.,.F.,(4,2,4),(4,2,2,4),(0.,
0.5,1.),(0.,0.25,0.5,1.),.UNSPECIFIED.);
#220=B_SPLINE_SURFACE_WITH_KNOTS('',3,3,((#29521,#29522,#29523,#29524,#29525,
#29526,#29527,#29528),(#29529,#29530,#29531,#29532,#29533,#29534,#29535,
#29536),(#29537,#29538,#29539,#29540,#29541,#29542,#29543,#29544),(#29545,
#29546,#29547,#29548,#29549,#29550,#29551,#29552),(#29553,#29554,#29555,
#29556,#29557,#29558,#29559,#29560),(#29561,#29562,#29563,#29564,#29565,
#29566,#29567,#29568),(#29569,#29570,#29571,#29572,#29573,#29574,#29575,
#29576),(#29577,#29578,#29579,#29580,#29581,#29582,#29583,#29584)),
 .UNSPECIFIED.,.F.,.F.,.F.,(4,2,2,4),(4,2,2,4),(0.,0.25,0.5,1.),(0.,0.25,
0.5,1.),.UNSPECIFIED.);
#221=B_SPLINE_SURFACE_WITH_KNOTS('',3,3,((#29602,#29603,#29604,#29605,#29606,
#29607),(#29608,#29609,#29610,#29611,#29612,#29613),(#29614,#29615,#29616,
#29617,#29618,#29619),(#29620,#29621,#29622,#29623,#29624,#29625),(#29626,
#29627,#29628,#29629,#29630,#29631),(#29632,#29633,#29634,#29635,#29636,
#29637),(#29638,#29639,#29640,#29641,#29642,#29643),(#29644,#29645,#29646,
#29647,#29648,#29649),(#29650,#29651,#29652,#29653,#29654,#29655),(#29656,
#29657,#29658,#29659,#29660,#29661)),.UNSPECIFIED.,.F.,.F.,.F.,(4,2,2,2,
4),(4,2,4),(0.,0.25,0.5,0.75,1.),(0.,0.5,1.),.UNSPECIFIED.);
#222=B_SPLINE_SURFACE_WITH_KNOTS('',3,3,((#29681,#29682,#29683,#29684,#29685,
#29686,#29687,#29688,#29689,#29690),(#29691,#29692,#29693,#29694,#29695,
#29696,#29697,#29698,#29699,#29700),(#29701,#29702,#29703,#29704,#29705,
#29706,#29707,#29708,#29709,#29710),(#29711,#29712,#29713,#29714,#29715,
#29716,#29717,#29718,#29719,#29720),(#29721,#29722,#29723,#29724,#29725,
#29726,#29727,#29728,#29729,#29730),(#29731,#29732,#29733,#29734,#29735,
#29736,#29737,#29738,#29739,#29740)),.UNSPECIFIED.,.F.,.F.,.F.,(4,2,4),
(4,2,2,2,4),(0.,0.5,1.),(0.,0.25,0.5,0.75,1.),.UNSPECIFIED.);
#223=B_SPLINE_SURFACE_WITH_KNOTS('',3,3,((#29764,#29765,#29766,#29767,#29768,
#29769,#29770,#29771),(#29772,#29773,#29774,#29775,#29776,#29777,#29778,
#29779),(#29780,#29781,#29782,#29783,#29784,#29785,#29786,#29787),(#29788,
#29789,#29790,#29791,#29792,#29793,#29794,#29795),(#29796,#29797,#29798,
#29799,#29800,#29801,#29802,#29803),(#29804,#29805,#29806,#29807,#29808,
#29809,#29810,#29811),(#29812,#29813,#29814,#29815,#29816,#29817,#29818,
#29819),(#29820,#29821,#29822,#29823,#29824,#29825,#29826,#29827)),
 .UNSPECIFIED.,.F.,.F.,.F.,(4,2,2,4),(4,2,2,4),(0.,0.25,0.5,1.),(0.,0.25,
0.5,1.),.UNSPECIFIED.);
#224=B_SPLINE_SURFACE_WITH_KNOTS('',3,3,((#29903,#29904,#29905,#29906,#29907,
#29908),(#29909,#29910,#29911,#29912,#29913,#29914),(#29915,#29916,#29917,
#29918,#29919,#29920),(#29921,#29922,#29923,#29924,#29925,#29926),(#29927,
#29928,#29929,#29930,#29931,#29932),(#29933,#29934,#29935,#29936,#29937,
#29938),(#29939,#29940,#29941,#29942,#29943,#29944),(#29945,#29946,#29947,
#29948,#29949,#29950)),.UNSPECIFIED.,.F.,.F.,.F.,(4,2,2,4),(4,2,4),(0.,
0.25,0.5,1.),(0.,0.5,1.),.UNSPECIFIED.);
#225=B_SPLINE_SURFACE_WITH_KNOTS('',3,3,((#29981,#29982,#29983,#29984,#29985,
#29986,#29987,#29988),(#29989,#29990,#29991,#29992,#29993,#29994,#29995,
#29996),(#29997,#29998,#29999,#30000,#30001,#30002,#30003,#30004),(#30005,
#30006,#30007,#30008,#30009,#30010,#30011,#30012),(#30013,#30014,#30015,
#30016,#30017,#30018,#30019,#30020),(#30021,#30022,#30023,#30024,#30025,
#30026,#30027,#30028)),.UNSPECIFIED.,.F.,.F.,.F.,(4,2,4),(4,2,2,4),(0.,
0.5,1.),(0.,0.25,0.5,1.),.UNSPECIFIED.);
#226=B_SPLINE_SURFACE_WITH_KNOTS('',3,3,((#30052,#30053,#30054,#30055,#30056,
#30057,#30058,#30059),(#30060,#30061,#30062,#30063,#30064,#30065,#30066,
#30067),(#30068,#30069,#30070,#30071,#30072,#30073,#30074,#30075),(#30076,
#30077,#30078,#30079,#30080,#30081,#30082,#30083),(#30084,#30085,#30086,
#30087,#30088,#30089,#30090,#30091),(#30092,#30093,#30094,#30095,#30096,
#30097,#30098,#30099),(#30100,#30101,#30102,#30103,#30104,#30105,#30106,
#30107),(#30108,#30109,#30110,#30111,#30112,#30113,#30114,#30115)),
 .UNSPECIFIED.,.F.,.F.,.F.,(4,2,2,4),(4,2,2,4),(0.,0.25,0.5,1.),(0.,0.25,
0.5,1.),.UNSPECIFIED.);
#227=B_SPLINE_SURFACE_WITH_KNOTS('',3,3,((#30133,#30134,#30135,#30136,#30137,
#30138),(#30139,#30140,#30141,#30142,#30143,#30144),(#30145,#30146,#30147,
#30148,#30149,#30150),(#30151,#30152,#30153,#30154,#30155,#30156),(#30157,
#30158,#30159,#30160,#30161,#30162),(#30163,#30164,#30165,#30166,#30167,
#30168),(#30169,#30170,#30171,#30172,#30173,#30174),(#30175,#30176,#30177,
#30178,#30179,#30180),(#30181,#30182,#30183,#30184,#30185,#30186),(#30187,
#30188,#30189,#30190,#30191,#30192)),.UNSPECIFIED.,.F.,.F.,.F.,(4,2,2,2,
4),(4,2,4),(0.,0.25,0.5,0.75,1.),(0.,0.5,1.),.UNSPECIFIED.);
#228=B_SPLINE_SURFACE_WITH_KNOTS('',3,3,((#30212,#30213,#30214,#30215,#30216,
#30217,#30218,#30219,#30220,#30221),(#30222,#30223,#30224,#30225,#30226,
#30227,#30228,#30229,#30230,#30231),(#30232,#30233,#30234,#30235,#30236,
#30237,#30238,#30239,#30240,#30241),(#30242,#30243,#30244,#30245,#30246,
#30247,#30248,#30249,#30250,#30251),(#30252,#30253,#30254,#30255,#30256,
#30257,#30258,#30259,#30260,#30261),(#30262,#30263,#30264,#30265,#30266,
#30267,#30268,#30269,#30270,#30271)),.UNSPECIFIED.,.F.,.F.,.F.,(4,2,4),
(4,2,2,2,4),(0.,0.5,1.),(0.,0.25,0.5,0.75,1.),.UNSPECIFIED.);
#229=B_SPLINE_SURFACE_WITH_KNOTS('',3,3,((#30280,#30281,#30282,#30283,#30284,
#30285,#30286,#30287,#30288,#30289),(#30290,#30291,#30292,#30293,#30294,
#30295,#30296,#30297,#30298,#30299),(#30300,#30301,#30302,#30303,#30304,
#30305,#30306,#30307,#30308,#30309),(#30310,#30311,#30312,#30313,#30314,
#30315,#30316,#30317,#30318,#30319),(#30320,#30321,#30322,#30323,#30324,
#30325,#30326,#30327,#30328,#30329),(#30330,#30331,#30332,#30333,#30334,
#30335,#30336,#30337,#30338,#30339)),.UNSPECIFIED.,.F.,.F.,.F.,(4,2,4),
(4,2,2,2,4),(0.,0.5,1.),(0.,0.25,0.5,0.75,1.),.UNSPECIFIED.);
#230=B_SPLINE_SURFACE_WITH_KNOTS('',3,3,((#30370,#30371,#30372,#30373,#30374,
#30375,#30376,#30377),(#30378,#30379,#30380,#30381,#30382,#30383,#30384,
#30385),(#30386,#30387,#30388,#30389,#30390,#30391,#30392,#30393),(#30394,
#30395,#30396,#30397,#30398,#30399,#30400,#30401),(#30402,#30403,#30404,
#30405,#30406,#30407,#30408,#30409),(#30410,#30411,#30412,#30413,#30414,
#30415,#30416,#30417),(#30418,#30419,#30420,#30421,#30422,#30423,#30424,
#30425),(#30426,#30427,#30428,#30429,#30430,#30431,#30432,#30433)),
 .UNSPECIFIED.,.F.,.F.,.F.,(4,2,2,4),(4,2,2,4),(0.,0.25,0.5,1.),(0.,0.25,
0.5,1.),.UNSPECIFIED.);
#231=B_SPLINE_SURFACE_WITH_KNOTS('',3,3,((#30451,#30452,#30453,#30454,#30455,
#30456),(#30457,#30458,#30459,#30460,#30461,#30462),(#30463,#30464,#30465,
#30466,#30467,#30468),(#30469,#30470,#30471,#30472,#30473,#30474),(#30475,
#30476,#30477,#30478,#30479,#30480),(#30481,#30482,#30483,#30484,#30485,
#30486),(#30487,#30488,#30489,#30490,#30491,#30492),(#30493,#30494,#30495,
#30496,#30497,#30498)),.UNSPECIFIED.,.F.,.F.,.F.,(4,2,2,4),(4,2,4),(0.,
0.25,0.5,1.),(0.,0.5,1.),.UNSPECIFIED.);
#232=B_SPLINE_SURFACE_WITH_KNOTS('',3,3,((#30521,#30522,#30523,#30524,#30525,
#30526,#30527,#30528),(#30529,#30530,#30531,#30532,#30533,#30534,#30535,
#30536),(#30537,#30538,#30539,#30540,#30541,#30542,#30543,#30544),(#30545,
#30546,#30547,#30548,#30549,#30550,#30551,#30552),(#30553,#30554,#30555,
#30556,#30557,#30558,#30559,#30560),(#30561,#30562,#30563,#30564,#30565,
#30566,#30567,#30568)),.UNSPECIFIED.,.F.,.F.,.F.,(4,2,4),(4,2,2,4),(0.,
0.5,1.),(0.,0.25,0.5,1.),.UNSPECIFIED.);
#233=B_SPLINE_SURFACE_WITH_KNOTS('',3,3,((#30592,#30593,#30594,#30595,#30596,
#30597,#30598,#30599),(#30600,#30601,#30602,#30603,#30604,#30605,#30606,
#30607),(#30608,#30609,#30610,#30611,#30612,#30613,#30614,#30615),(#30616,
#30617,#30618,#30619,#30620,#30621,#30622,#30623),(#30624,#30625,#30626,
#30627,#30628,#30629,#30630,#30631),(#30632,#30633,#30634,#30635,#30636,
#30637,#30638,#30639),(#30640,#30641,#30642,#30643,#30644,#30645,#30646,
#30647),(#30648,#30649,#30650,#30651,#30652,#30653,#30654,#30655)),
 .UNSPECIFIED.,.F.,.F.,.F.,(4,2,2,4),(4,2,2,4),(0.,0.25,0.5,1.),(0.,0.25,
0.5,1.),.UNSPECIFIED.);
#234=B_SPLINE_SURFACE_WITH_KNOTS('',3,3,((#30724,#30725,#30726,#30727,#30728,
#30729),(#30730,#30731,#30732,#30733,#30734,#30735),(#30736,#30737,#30738,
#30739,#30740,#30741),(#30742,#30743,#30744,#30745,#30746,#30747),(#30748,
#30749,#30750,#30751,#30752,#30753),(#30754,#30755,#30756,#30757,#30758,
#30759),(#30760,#30761,#30762,#30763,#30764,#30765),(#30766,#30767,#30768,
#30769,#30770,#30771)),.UNSPECIFIED.,.F.,.F.,.F.,(4,2,2,4),(4,2,4),(0.,
0.25,0.5,1.),(0.,0.5,1.),.UNSPECIFIED.);
#235=B_SPLINE_SURFACE_WITH_KNOTS('',3,3,((#30802,#30803,#30804,#30805,#30806,
#30807,#30808,#30809),(#30810,#30811,#30812,#30813,#30814,#30815,#30816,
#30817),(#30818,#30819,#30820,#30821,#30822,#30823,#30824,#30825),(#30826,
#30827,#30828,#30829,#30830,#30831,#30832,#30833),(#30834,#30835,#30836,
#30837,#30838,#30839,#30840,#30841),(#30842,#30843,#30844,#30845,#30846,
#30847,#30848,#30849)),.UNSPECIFIED.,.F.,.F.,.F.,(4,2,4),(4,2,2,4),(0.,
0.5,1.),(0.,0.25,0.5,1.),.UNSPECIFIED.);
#236=B_SPLINE_SURFACE_WITH_KNOTS('',3,3,((#30873,#30874,#30875,#30876,#30877,
#30878,#30879,#30880),(#30881,#30882,#30883,#30884,#30885,#30886,#30887,
#30888),(#30889,#30890,#30891,#30892,#30893,#30894,#30895,#30896),(#30897,
#30898,#30899,#30900,#30901,#30902,#30903,#30904),(#30905,#30906,#30907,
#30908,#30909,#30910,#30911,#30912),(#30913,#30914,#30915,#30916,#30917,
#30918,#30919,#30920),(#30921,#30922,#30923,#30924,#30925,#30926,#30927,
#30928),(#30929,#30930,#30931,#30932,#30933,#30934,#30935,#30936)),
 .UNSPECIFIED.,.F.,.F.,.F.,(4,2,2,4),(4,2,2,4),(0.,0.25,0.5,1.),(0.,0.25,
0.5,1.),.UNSPECIFIED.);
#237=B_SPLINE_SURFACE_WITH_KNOTS('',3,3,((#31005,#31006,#31007,#31008,#31009,
#31010),(#31011,#31012,#31013,#31014,#31015,#31016),(#31017,#31018,#31019,
#31020,#31021,#31022),(#31023,#31024,#31025,#31026,#31027,#31028),(#31029,
#31030,#31031,#31032,#31033,#31034),(#31035,#31036,#31037,#31038,#31039,
#31040),(#31041,#31042,#31043,#31044,#31045,#31046),(#31047,#31048,#31049,
#31050,#31051,#31052),(#31053,#31054,#31055,#31056,#31057,#31058),(#31059,
#31060,#31061,#31062,#31063,#31064)),.UNSPECIFIED.,.F.,.F.,.F.,(4,2,2,2,
4),(4,2,4),(0.,0.25,0.5,0.75,1.),(0.,0.5,1.),.UNSPECIFIED.);
#238=B_SPLINE_SURFACE_WITH_KNOTS('',3,3,((#31072,#31073,#31074,#31075,#31076,
#31077,#31078,#31079,#31080,#31081),(#31082,#31083,#31084,#31085,#31086,
#31087,#31088,#31089,#31090,#31091),(#31092,#31093,#31094,#31095,#31096,
#31097,#31098,#31099,#31100,#31101),(#31102,#31103,#31104,#31105,#31106,
#31107,#31108,#31109,#31110,#31111),(#31112,#31113,#31114,#31115,#31116,
#31117,#31118,#31119,#31120,#31121),(#31122,#31123,#31124,#31125,#31126,
#31127,#31128,#31129,#31130,#31131)),.UNSPECIFIED.,.F.,.F.,.F.,(4,2,4),
(4,2,2,2,4),(0.,0.5,1.),(0.,0.25,0.5,0.75,1.),.UNSPECIFIED.);
#239=B_SPLINE_SURFACE_WITH_KNOTS('',3,3,((#31286,#31287,#31288,#31289,#31290,
#31291,#31292,#31293),(#31294,#31295,#31296,#31297,#31298,#31299,#31300,
#31301),(#31302,#31303,#31304,#31305,#31306,#31307,#31308,#31309),(#31310,
#31311,#31312,#31313,#31314,#31315,#31316,#31317),(#31318,#31319,#31320,
#31321,#31322,#31323,#31324,#31325),(#31326,#31327,#31328,#31329,#31330,
#31331,#31332,#31333),(#31334,#31335,#31336,#31337,#31338,#31339,#31340,
#31341),(#31342,#31343,#31344,#31345,#31346,#31347,#31348,#31349)),
 .UNSPECIFIED.,.F.,.F.,.F.,(4,2,2,4),(4,2,2,4),(0.,0.25,0.5,1.),(0.,0.25,
0.5,1.),.UNSPECIFIED.);
#240=B_SPLINE_SURFACE_WITH_KNOTS('',3,3,((#31663,#31664,#31665,#31666,#31667,
#31668),(#31669,#31670,#31671,#31672,#31673,#31674),(#31675,#31676,#31677,
#31678,#31679,#31680),(#31681,#31682,#31683,#31684,#31685,#31686),(#31687,
#31688,#31689,#31690,#31691,#31692),(#31693,#31694,#31695,#31696,#31697,
#31698),(#31699,#31700,#31701,#31702,#31703,#31704),(#31705,#31706,#31707,
#31708,#31709,#31710),(#31711,#31712,#31713,#31714,#31715,#31716),(#31717,
#31718,#31719,#31720,#31721,#31722)),.UNSPECIFIED.,.F.,.F.,.F.,(4,2,2,2,
4),(4,2,4),(0.,0.25,0.5,0.75,1.),(0.,0.5,1.),.UNSPECIFIED.);
#241=B_SPLINE_SURFACE_WITH_KNOTS('',3,3,((#31724,#31725,#31726,#31727,#31728,
#31729,#31730,#31731),(#31732,#31733,#31734,#31735,#31736,#31737,#31738,
#31739),(#31740,#31741,#31742,#31743,#31744,#31745,#31746,#31747),(#31748,
#31749,#31750,#31751,#31752,#31753,#31754,#31755),(#31756,#31757,#31758,
#31759,#31760,#31761,#31762,#31763),(#31764,#31765,#31766,#31767,#31768,
#31769,#31770,#31771),(#31772,#31773,#31774,#31775,#31776,#31777,#31778,
#31779),(#31780,#31781,#31782,#31783,#31784,#31785,#31786,#31787)),
 .UNSPECIFIED.,.F.,.F.,.F.,(4,2,2,4),(4,2,2,4),(0.,0.25,0.5,1.),(0.,0.25,
0.5,1.),.UNSPECIFIED.);
#242=B_SPLINE_SURFACE_WITH_KNOTS('',3,3,((#31930,#31931,#31932,#31933,#31934,
#31935),(#31936,#31937,#31938,#31939,#31940,#31941),(#31942,#31943,#31944,
#31945,#31946,#31947),(#31948,#31949,#31950,#31951,#31952,#31953),(#31954,
#31955,#31956,#31957,#31958,#31959),(#31960,#31961,#31962,#31963,#31964,
#31965),(#31966,#31967,#31968,#31969,#31970,#31971),(#31972,#31973,#31974,
#31975,#31976,#31977)),.UNSPECIFIED.,.F.,.F.,.F.,(4,2,2,4),(4,2,4),(0.,
0.25,0.5,1.),(0.,0.5,1.),.UNSPECIFIED.);
#243=B_SPLINE_SURFACE_WITH_KNOTS('',3,3,((#32650,#32651,#32652,#32653,#32654,
#32655,#32656),(#32657,#32658,#32659,#32660,#32661,#32662,#32663),(#32664,
#32665,#32666,#32667,#32668,#32669,#32670),(#32671,#32672,#32673,#32674,
#32675,#32676,#32677),(#32678,#32679,#32680,#32681,#32682,#32683,#32684),
(#32685,#32686,#32687,#32688,#32689,#32690,#32691),(#32692,#32693,#32694,
#32695,#32696,#32697,#32698),(#32699,#32700,#32701,#32702,#32703,#32704,
#32705),(#32706,#32707,#32708,#32709,#32710,#32711,#32712),(#32713,#32714,
#32715,#32716,#32717,#32718,#32719),(#32720,#32721,#32722,#32723,#32724,
#32725,#32726),(#32727,#32728,#32729,#32730,#32731,#32732,#32733),(#32734,
#32735,#32736,#32737,#32738,#32739,#32740)),.UNSPECIFIED.,.F.,.F.,.F.,(4,
3,1,1,1,3,4),(4,3,4),(0.991784279387784,0.992409194183265,0.994306895637448,
0.996204597091632,0.998102298545816,1.,1.0001828629104),(-0.00779503841308724,
0.,0.779503841308724),.UNSPECIFIED.);
#244=B_SPLINE_SURFACE_WITH_KNOTS('',3,3,((#32756,#32757,#32758,#32759,#32760,
#32761,#32762,#32763,#32764,#32765,#32766,#32767,#32768,#32769,#32770,#32771,
#32772),(#32773,#32774,#32775,#32776,#32777,#32778,#32779,#32780,#32781,
#32782,#32783,#32784,#32785,#32786,#32787,#32788,#32789),(#32790,#32791,
#32792,#32793,#32794,#32795,#32796,#32797,#32798,#32799,#32800,#32801,#32802,
#32803,#32804,#32805,#32806),(#32807,#32808,#32809,#32810,#32811,#32812,
#32813,#32814,#32815,#32816,#32817,#32818,#32819,#32820,#32821,#32822,#32823),
(#32824,#32825,#32826,#32827,#32828,#32829,#32830,#32831,#32832,#32833,
#32834,#32835,#32836,#32837,#32838,#32839,#32840),(#32841,#32842,#32843,
#32844,#32845,#32846,#32847,#32848,#32849,#32850,#32851,#32852,#32853,#32854,
#32855,#32856,#32857),(#32858,#32859,#32860,#32861,#32862,#32863,#32864,
#32865,#32866,#32867,#32868,#32869,#32870,#32871,#32872,#32873,#32874),
(#32875,#32876,#32877,#32878,#32879,#32880,#32881,#32882,#32883,#32884,
#32885,#32886,#32887,#32888,#32889,#32890,#32891),(#32892,#32893,#32894,
#32895,#32896,#32897,#32898,#32899,#32900,#32901,#32902,#32903,#32904,#32905,
#32906,#32907,#32908),(#32909,#32910,#32911,#32912,#32913,#32914,#32915,
#32916,#32917,#32918,#32919,#32920,#32921,#32922,#32923,#32924,#32925),
(#32926,#32927,#32928,#32929,#32930,#32931,#32932,#32933,#32934,#32935,
#32936,#32937,#32938,#32939,#32940,#32941,#32942),(#32943,#32944,#32945,
#32946,#32947,#32948,#32949,#32950,#32951,#32952,#32953,#32954,#32955,#32956,
#32957,#32958,#32959),(#32960,#32961,#32962,#32963,#32964,#32965,#32966,
#32967,#32968,#32969,#32970,#32971,#32972,#32973,#32974,#32975,#32976),
(#32977,#32978,#32979,#32980,#32981,#32982,#32983,#32984,#32985,#32986,
#32987,#32988,#32989,#32990,#32991,#32992,#32993),(#32994,#32995,#32996,
#32997,#32998,#32999,#33000,#33001,#33002,#33003,#33004,#33005,#33006,#33007,
#33008,#33009,#33010),(#33011,#33012,#33013,#33014,#33015,#33016,#33017,
#33018,#33019,#33020,#33021,#33022,#33023,#33024,#33025,#33026,#33027)),
 .UNSPECIFIED.,.F.,.F.,.F.,(4,2,1,1,1,1,1,1,1,1,2,4),(4,2,1,1,1,1,1,1,1,
1,1,2,4),(-0.035701835836904,0.,0.090219017653024,0.22554754413256,0.315766561785584,
0.45109508826512,0.541314105918144,0.67664263239768,0.766861650050704,0.90219017653024,
0.992409194183265,1.02810227746674),(-0.0217729438654334,0.,0.0708639855735204,
0.141727971147041,0.212591956720561,0.318887935080842,0.389751920654362,
0.460615906227882,0.566911884588163,0.637775870161683,0.708639855735204,
0.779503841308724,0.801994948010107),.UNSPECIFIED.);
#245=B_SPLINE_SURFACE_WITH_KNOTS('',3,3,((#33062,#33063,#33064,#33065,#33066,
#33067,#33068,#33069,#33070,#33071,#33072,#33073,#33074,#33075,#33076,#33077,
#33078),(#33079,#33080,#33081,#33082,#33083,#33084,#33085,#33086,#33087,
#33088,#33089,#33090,#33091,#33092,#33093,#33094,#33095),(#33096,#33097,
#33098,#33099,#33100,#33101,#33102,#33103,#33104,#33105,#33106,#33107,#33108,
#33109,#33110,#33111,#33112),(#33113,#33114,#33115,#33116,#33117,#33118,
#33119,#33120,#33121,#33122,#33123,#33124,#33125,#33126,#33127,#33128,#33129),
(#33130,#33131,#33132,#33133,#33134,#33135,#33136,#33137,#33138,#33139,
#33140,#33141,#33142,#33143,#33144,#33145,#33146),(#33147,#33148,#33149,
#33150,#33151,#33152,#33153,#33154,#33155,#33156,#33157,#33158,#33159,#33160,
#33161,#33162,#33163),(#33164,#33165,#33166,#33167,#33168,#33169,#33170,
#33171,#33172,#33173,#33174,#33175,#33176,#33177,#33178,#33179,#33180),
(#33181,#33182,#33183,#33184,#33185,#33186,#33187,#33188,#33189,#33190,
#33191,#33192,#33193,#33194,#33195,#33196,#33197),(#33198,#33199,#33200,
#33201,#33202,#33203,#33204,#33205,#33206,#33207,#33208,#33209,#33210,#33211,
#33212,#33213,#33214),(#33215,#33216,#33217,#33218,#33219,#33220,#33221,
#33222,#33223,#33224,#33225,#33226,#33227,#33228,#33229,#33230,#33231),
(#33232,#33233,#33234,#33235,#33236,#33237,#33238,#33239,#33240,#33241,
#33242,#33243,#33244,#33245,#33246,#33247,#33248),(#33249,#33250,#33251,
#33252,#33253,#33254,#33255,#33256,#33257,#33258,#33259,#33260,#33261,#33262,
#33263,#33264,#33265),(#33266,#33267,#33268,#33269,#33270,#33271,#33272,
#33273,#33274,#33275,#33276,#33277,#33278,#33279,#33280,#33281,#33282),
(#33283,#33284,#33285,#33286,#33287,#33288,#33289,#33290,#33291,#33292,
#33293,#33294,#33295,#33296,#33297,#33298,#33299),(#33300,#33301,#33302,
#33303,#33304,#33305,#33306,#33307,#33308,#33309,#33310,#33311,#33312,#33313,
#33314,#33315,#33316),(#33317,#33318,#33319,#33320,#33321,#33322,#33323,
#33324,#33325,#33326,#33327,#33328,#33329,#33330,#33331,#33332,#33333),
(#33334,#33335,#33336,#33337,#33338,#33339,#33340,#33341,#33342,#33343,
#33344,#33345,#33346,#33347,#33348,#33349,#33350)),.UNSPECIFIED.,.F.,.F.,
 .F.,(4,2,1,1,1,1,1,1,1,1,1,2,4),(4,2,1,1,1,1,1,1,1,1,1,2,4),(-0.0353050121574204,
0.,0.0909090909090909,0.181818181818182,0.272727272727273,0.409090909090909,
0.5,0.590909090909091,0.727272727272727,0.818181818181818,0.909090909090909,
1.,1.03479194496591),(-0.021689269548343,0.,0.0708639855735204,0.141727971147041,
0.212591956720561,0.318887935080842,0.389751920654362,0.460615906227882,
0.566911884588163,0.637775870161683,0.708639855735204,0.779503841308724,
0.801875267322681),.UNSPECIFIED.);
#246=B_SPLINE_SURFACE_WITH_KNOTS('',3,3,((#33361,#33362,#33363,#33364,#33365,
#33366,#33367,#33368,#33369,#33370,#33371,#33372,#33373,#33374,#33375,#33376,
#33377),(#33378,#33379,#33380,#33381,#33382,#33383,#33384,#33385,#33386,
#33387,#33388,#33389,#33390,#33391,#33392,#33393,#33394),(#33395,#33396,
#33397,#33398,#33399,#33400,#33401,#33402,#33403,#33404,#33405,#33406,#33407,
#33408,#33409,#33410,#33411),(#33412,#33413,#33414,#33415,#33416,#33417,
#33418,#33419,#33420,#33421,#33422,#33423,#33424,#33425,#33426,#33427,#33428),
(#33429,#33430,#33431,#33432,#33433,#33434,#33435,#33436,#33437,#33438,
#33439,#33440,#33441,#33442,#33443,#33444,#33445),(#33446,#33447,#33448,
#33449,#33450,#33451,#33452,#33453,#33454,#33455,#33456,#33457,#33458,#33459,
#33460,#33461,#33462),(#33463,#33464,#33465,#33466,#33467,#33468,#33469,
#33470,#33471,#33472,#33473,#33474,#33475,#33476,#33477,#33478,#33479),
(#33480,#33481,#33482,#33483,#33484,#33485,#33486,#33487,#33488,#33489,
#33490,#33491,#33492,#33493,#33494,#33495,#33496),(#33497,#33498,#33499,
#33500,#33501,#33502,#33503,#33504,#33505,#33506,#33507,#33508,#33509,#33510,
#33511,#33512,#33513),(#33514,#33515,#33516,#33517,#33518,#33519,#33520,
#33521,#33522,#33523,#33524,#33525,#33526,#33527,#33528,#33529,#33530),
(#33531,#33532,#33533,#33534,#33535,#33536,#33537,#33538,#33539,#33540,
#33541,#33542,#33543,#33544,#33545,#33546,#33547),(#33548,#33549,#33550,
#33551,#33552,#33553,#33554,#33555,#33556,#33557,#33558,#33559,#33560,#33561,
#33562,#33563,#33564),(#33565,#33566,#33567,#33568,#33569,#33570,#33571,
#33572,#33573,#33574,#33575,#33576,#33577,#33578,#33579,#33580,#33581),
(#33582,#33583,#33584,#33585,#33586,#33587,#33588,#33589,#33590,#33591,
#33592,#33593,#33594,#33595,#33596,#33597,#33598),(#33599,#33600,#33601,
#33602,#33603,#33604,#33605,#33606,#33607,#33608,#33609,#33610,#33611,#33612,
#33613,#33614,#33615),(#33616,#33617,#33618,#33619,#33620,#33621,#33622,
#33623,#33624,#33625,#33626,#33627,#33628,#33629,#33630,#33631,#33632),
(#33633,#33634,#33635,#33636,#33637,#33638,#33639,#33640,#33641,#33642,
#33643,#33644,#33645,#33646,#33647,#33648,#33649)),.UNSPECIFIED.,.F.,.F.,
 .F.,(4,2,1,1,1,1,1,1,1,1,1,2,4),(4,2,1,1,1,1,1,1,1,1,1,2,4),(-0.0353050121574204,
0.,0.0909090909090909,0.181818181818182,0.272727272727273,0.409090909090909,
0.5,0.590909090909091,0.727272727272727,0.818181818181818,0.909090909090909,
1.,1.03479194496591),(-0.021689269548343,0.,0.0708639855735204,0.141727971147041,
0.212591956720561,0.318887935080842,0.389751920654362,0.460615906227882,
0.566911884588163,0.637775870161683,0.708639855735204,0.779503841308724,
0.801875267322681),.UNSPECIFIED.);
#247=B_SPLINE_SURFACE_WITH_KNOTS('',3,3,((#33693,#33694,#33695,#33696,#33697,
#33698,#33699,#33700,#33701,#33702,#33703,#33704,#33705,#33706,#33707,#33708,
#33709),(#33710,#33711,#33712,#33713,#33714,#33715,#33716,#33717,#33718,
#33719,#33720,#33721,#33722,#33723,#33724,#33725,#33726),(#33727,#33728,
#33729,#33730,#33731,#33732,#33733,#33734,#33735,#33736,#33737,#33738,#33739,
#33740,#33741,#33742,#33743),(#33744,#33745,#33746,#33747,#33748,#33749,
#33750,#33751,#33752,#33753,#33754,#33755,#33756,#33757,#33758,#33759,#33760),
(#33761,#33762,#33763,#33764,#33765,#33766,#33767,#33768,#33769,#33770,
#33771,#33772,#33773,#33774,#33775,#33776,#33777),(#33778,#33779,#33780,
#33781,#33782,#33783,#33784,#33785,#33786,#33787,#33788,#33789,#33790,#33791,
#33792,#33793,#33794),(#33795,#33796,#33797,#33798,#33799,#33800,#33801,
#33802,#33803,#33804,#33805,#33806,#33807,#33808,#33809,#33810,#33811),
(#33812,#33813,#33814,#33815,#33816,#33817,#33818,#33819,#33820,#33821,
#33822,#33823,#33824,#33825,#33826,#33827,#33828),(#33829,#33830,#33831,
#33832,#33833,#33834,#33835,#33836,#33837,#33838,#33839,#33840,#33841,#33842,
#33843,#33844,#33845),(#33846,#33847,#33848,#33849,#33850,#33851,#33852,
#33853,#33854,#33855,#33856,#33857,#33858,#33859,#33860,#33861,#33862),
(#33863,#33864,#33865,#33866,#33867,#33868,#33869,#33870,#33871,#33872,
#33873,#33874,#33875,#33876,#33877,#33878,#33879),(#33880,#33881,#33882,
#33883,#33884,#33885,#33886,#33887,#33888,#33889,#33890,#33891,#33892,#33893,
#33894,#33895,#33896),(#33897,#33898,#33899,#33900,#33901,#33902,#33903,
#33904,#33905,#33906,#33907,#33908,#33909,#33910,#33911,#33912,#33913),
(#33914,#33915,#33916,#33917,#33918,#33919,#33920,#33921,#33922,#33923,
#33924,#33925,#33926,#33927,#33928,#33929,#33930),(#33931,#33932,#33933,
#33934,#33935,#33936,#33937,#33938,#33939,#33940,#33941,#33942,#33943,#33944,
#33945,#33946,#33947),(#33948,#33949,#33950,#33951,#33952,#33953,#33954,
#33955,#33956,#33957,#33958,#33959,#33960,#33961,#33962,#33963,#33964)),
 .UNSPECIFIED.,.F.,.F.,.F.,(4,2,1,1,1,1,1,1,1,1,2,4),(4,2,1,1,1,1,1,1,1,
1,1,2,4),(-0.035701835836904,0.,0.090219017653024,0.22554754413256,0.315766561785584,
0.45109508826512,0.541314105918144,0.67664263239768,0.766861650050704,0.90219017653024,
0.992409194183265,1.02810227746674),(-0.0217729438654334,0.,0.0708639855735204,
0.141727971147041,0.212591956720561,0.318887935080842,0.389751920654362,
0.460615906227882,0.566911884588163,0.637775870161683,0.708639855735204,
0.779503841308724,0.801994948010107),.UNSPECIFIED.);
#248=B_SPLINE_SURFACE_WITH_KNOTS('',3,3,((#33980,#33981,#33982,#33983,#33984,
#33985,#33986),(#33987,#33988,#33989,#33990,#33991,#33992,#33993),(#33994,
#33995,#33996,#33997,#33998,#33999,#34000),(#34001,#34002,#34003,#34004,
#34005,#34006,#34007),(#34008,#34009,#34010,#34011,#34012,#34013,#34014),
(#34015,#34016,#34017,#34018,#34019,#34020,#34021),(#34022,#34023,#34024,
#34025,#34026,#34027,#34028),(#34029,#34030,#34031,#34032,#34033,#34034,
#34035),(#34036,#34037,#34038,#34039,#34040,#34041,#34042),(#34043,#34044,
#34045,#34046,#34047,#34048,#34049),(#34050,#34051,#34052,#34053,#34054,
#34055,#34056),(#34057,#34058,#34059,#34060,#34061,#34062,#34063),(#34064,
#34065,#34066,#34067,#34068,#34069,#34070)),.UNSPECIFIED.,.F.,.F.,.F.,(4,
3,1,1,1,3,4),(4,3,4),(0.991784279387784,0.992409194183265,0.994306895637448,
0.996204597091632,0.998102298545816,1.,1.0001828629104),(-0.00779503841308724,
0.,0.779503841308724),.UNSPECIFIED.);
#249=B_SPLINE_SURFACE_WITH_KNOTS('',3,3,((#34072,#34073,#34074,#34075,#34076,
#34077,#34078,#34079,#34080,#34081,#34082,#34083,#34084,#34085,#34086,#34087,
#34088),(#34089,#34090,#34091,#34092,#34093,#34094,#34095,#34096,#34097,
#34098,#34099,#34100,#34101,#34102,#34103,#34104,#34105),(#34106,#34107,
#34108,#34109,#34110,#34111,#34112,#34113,#34114,#34115,#34116,#34117,#34118,
#34119,#34120,#34121,#34122),(#34123,#34124,#34125,#34126,#34127,#34128,
#34129,#34130,#34131,#34132,#34133,#34134,#34135,#34136,#34137,#34138,#34139),
(#34140,#34141,#34142,#34143,#34144,#34145,#34146,#34147,#34148,#34149,
#34150,#34151,#34152,#34153,#34154,#34155,#34156),(#34157,#34158,#34159,
#34160,#34161,#34162,#34163,#34164,#34165,#34166,#34167,#34168,#34169,#34170,
#34171,#34172,#34173),(#34174,#34175,#34176,#34177,#34178,#34179,#34180,
#34181,#34182,#34183,#34184,#34185,#34186,#34187,#34188,#34189,#34190),
(#34191,#34192,#34193,#34194,#34195,#34196,#34197,#34198,#34199,#34200,
#34201,#34202,#34203,#34204,#34205,#34206,#34207),(#34208,#34209,#34210,
#34211,#34212,#34213,#34214,#34215,#34216,#34217,#34218,#34219,#34220,#34221,
#34222,#34223,#34224),(#34225,#34226,#34227,#34228,#34229,#34230,#34231,
#34232,#34233,#34234,#34235,#34236,#34237,#34238,#34239,#34240,#34241),
(#34242,#34243,#34244,#34245,#34246,#34247,#34248,#34249,#34250,#34251,
#34252,#34253,#34254,#34255,#34256,#34257,#34258),(#34259,#34260,#34261,
#34262,#34263,#34264,#34265,#34266,#34267,#34268,#34269,#34270,#34271,#34272,
#34273,#34274,#34275),(#34276,#34277,#34278,#34279,#34280,#34281,#34282,
#34283,#34284,#34285,#34286,#34287,#34288,#34289,#34290,#34291,#34292),
(#34293,#34294,#34295,#34296,#34297,#34298,#34299,#34300,#34301,#34302,
#34303,#34304,#34305,#34306,#34307,#34308,#34309),(#34310,#34311,#34312,
#34313,#34314,#34315,#34316,#34317,#34318,#34319,#34320,#34321,#34322,#34323,
#34324,#34325,#34326),(#34327,#34328,#34329,#34330,#34331,#34332,#34333,
#34334,#34335,#34336,#34337,#34338,#34339,#34340,#34341,#34342,#34343),
(#34344,#34345,#34346,#34347,#34348,#34349,#34350,#34351,#34352,#34353,
#34354,#34355,#34356,#34357,#34358,#34359,#34360)),.UNSPECIFIED.,.F.,.F.,
 .F.,(4,2,1,1,1,1,1,1,1,1,1,2,4),(4,2,1,1,1,1,1,1,1,1,1,2,4),(-0.0353050121574204,
0.,0.0909090909090909,0.181818181818182,0.272727272727273,0.409090909090909,
0.5,0.590909090909091,0.727272727272727,0.818181818181818,0.909090909090909,
1.,1.03479194496591),(-0.021689269548343,0.,0.0708639855735204,0.141727971147041,
0.212591956720561,0.318887935080842,0.389751920654362,0.460615906227882,
0.566911884588163,0.637775870161683,0.708639855735204,0.779503841308724,
0.801875267322681),.UNSPECIFIED.);
#250=B_SPLINE_SURFACE_WITH_KNOTS('',3,3,((#34404,#34405,#34406,#34407,#34408,
#34409,#34410,#34411,#34412,#34413,#34414,#34415,#34416,#34417,#34418,#34419,
#34420),(#34421,#34422,#34423,#34424,#34425,#34426,#34427,#34428,#34429,
#34430,#34431,#34432,#34433,#34434,#34435,#34436,#34437),(#34438,#34439,
#34440,#34441,#34442,#34443,#34444,#34445,#34446,#34447,#34448,#34449,#34450,
#34451,#34452,#34453,#34454),(#34455,#34456,#34457,#34458,#34459,#34460,
#34461,#34462,#34463,#34464,#34465,#34466,#34467,#34468,#34469,#34470,#34471),
(#34472,#34473,#34474,#34475,#34476,#34477,#34478,#34479,#34480,#34481,
#34482,#34483,#34484,#34485,#34486,#34487,#34488),(#34489,#34490,#34491,
#34492,#34493,#34494,#34495,#34496,#34497,#34498,#34499,#34500,#34501,#34502,
#34503,#34504,#34505),(#34506,#34507,#34508,#34509,#34510,#34511,#34512,
#34513,#34514,#34515,#34516,#34517,#34518,#34519,#34520,#34521,#34522),
(#34523,#34524,#34525,#34526,#34527,#34528,#34529,#34530,#34531,#34532,
#34533,#34534,#34535,#34536,#34537,#34538,#34539),(#34540,#34541,#34542,
#34543,#34544,#34545,#34546,#34547,#34548,#34549,#34550,#34551,#34552,#34553,
#34554,#34555,#34556),(#34557,#34558,#34559,#34560,#34561,#34562,#34563,
#34564,#34565,#34566,#34567,#34568,#34569,#34570,#34571,#34572,#34573),
(#34574,#34575,#34576,#34577,#34578,#34579,#34580,#34581,#34582,#34583,
#34584,#34585,#34586,#34587,#34588,#34589,#34590),(#34591,#34592,#34593,
#34594,#34595,#34596,#34597,#34598,#34599,#34600,#34601,#34602,#34603,#34604,
#34605,#34606,#34607),(#34608,#34609,#34610,#34611,#34612,#34613,#34614,
#34615,#34616,#34617,#34618,#34619,#34620,#34621,#34622,#34623,#34624),
(#34625,#34626,#34627,#34628,#34629,#34630,#34631,#34632,#34633,#34634,
#34635,#34636,#34637,#34638,#34639,#34640,#34641),(#34642,#34643,#34644,
#34645,#34646,#34647,#34648,#34649,#34650,#34651,#34652,#34653,#34654,#34655,
#34656,#34657,#34658),(#34659,#34660,#34661,#34662,#34663,#34664,#34665,
#34666,#34667,#34668,#34669,#34670,#34671,#34672,#34673,#34674,#34675)),
 .UNSPECIFIED.,.F.,.F.,.F.,(4,2,1,1,1,1,1,1,1,1,2,4),(4,2,1,1,1,1,1,1,1,
1,1,2,4),(-0.035701835836904,0.,0.090219017653024,0.22554754413256,0.315766561785584,
0.45109508826512,0.541314105918144,0.67664263239768,0.766861650050704,0.90219017653024,
0.992409194183265,1.02810227746674),(-0.0217729438654334,0.,0.0708639855735204,
0.141727971147041,0.212591956720561,0.318887935080842,0.389751920654362,
0.460615906227882,0.566911884588163,0.637775870161683,0.708639855735204,
0.779503841308724,0.801994948010107),.UNSPECIFIED.);
#251=B_SPLINE_SURFACE_WITH_KNOTS('',3,3,((#34691,#34692,#34693,#34694,#34695,
#34696,#34697),(#34698,#34699,#34700,#34701,#34702,#34703,#34704),(#34705,
#34706,#34707,#34708,#34709,#34710,#34711),(#34712,#34713,#34714,#34715,
#34716,#34717,#34718),(#34719,#34720,#34721,#34722,#34723,#34724,#34725),
(#34726,#34727,#34728,#34729,#34730,#34731,#34732),(#34733,#34734,#34735,
#34736,#34737,#34738,#34739),(#34740,#34741,#34742,#34743,#34744,#34745,
#34746),(#34747,#34748,#34749,#34750,#34751,#34752,#34753),(#34754,#34755,
#34756,#34757,#34758,#34759,#34760),(#34761,#34762,#34763,#34764,#34765,
#34766,#34767),(#34768,#34769,#34770,#34771,#34772,#34773,#34774),(#34775,
#34776,#34777,#34778,#34779,#34780,#34781)),.UNSPECIFIED.,.F.,.F.,.F.,(4,
3,1,1,1,3,4),(4,3,4),(0.991784279387784,0.992409194183265,0.994306895637448,
0.996204597091632,0.998102298545816,1.,1.0001828629104),(-0.00779503841308724,
0.,0.779503841308724),.UNSPECIFIED.);
#252=B_SPLINE_SURFACE_WITH_KNOTS('',3,3,((#34783,#34784,#34785,#34786,#34787,
#34788,#34789,#34790,#34791,#34792,#34793,#34794,#34795,#34796,#34797,#34798,
#34799),(#34800,#34801,#34802,#34803,#34804,#34805,#34806,#34807,#34808,
#34809,#34810,#34811,#34812,#34813,#34814,#34815,#34816),(#34817,#34818,
#34819,#34820,#34821,#34822,#34823,#34824,#34825,#34826,#34827,#34828,#34829,
#34830,#34831,#34832,#34833),(#34834,#34835,#34836,#34837,#34838,#34839,
#34840,#34841,#34842,#34843,#34844,#34845,#34846,#34847,#34848,#34849,#34850),
(#34851,#34852,#34853,#34854,#34855,#34856,#34857,#34858,#34859,#34860,
#34861,#34862,#34863,#34864,#34865,#34866,#34867),(#34868,#34869,#34870,
#34871,#34872,#34873,#34874,#34875,#34876,#34877,#34878,#34879,#34880,#34881,
#34882,#34883,#34884),(#34885,#34886,#34887,#34888,#34889,#34890,#34891,
#34892,#34893,#34894,#34895,#34896,#34897,#34898,#34899,#34900,#34901),
(#34902,#34903,#34904,#34905,#34906,#34907,#34908,#34909,#34910,#34911,
#34912,#34913,#34914,#34915,#34916,#34917,#34918),(#34919,#34920,#34921,
#34922,#34923,#34924,#34925,#34926,#34927,#34928,#34929,#34930,#34931,#34932,
#34933,#34934,#34935),(#34936,#34937,#34938,#34939,#34940,#34941,#34942,
#34943,#34944,#34945,#34946,#34947,#34948,#34949,#34950,#34951,#34952),
(#34953,#34954,#34955,#34956,#34957,#34958,#34959,#34960,#34961,#34962,
#34963,#34964,#34965,#34966,#34967,#34968,#34969),(#34970,#34971,#34972,
#34973,#34974,#34975,#34976,#34977,#34978,#34979,#34980,#34981,#34982,#34983,
#34984,#34985,#34986),(#34987,#34988,#34989,#34990,#34991,#34992,#34993,
#34994,#34995,#34996,#34997,#34998,#34999,#35000,#35001,#35002,#35003),
(#35004,#35005,#35006,#35007,#35008,#35009,#35010,#35011,#35012,#35013,
#35014,#35015,#35016,#35017,#35018,#35019,#35020),(#35021,#35022,#35023,
#35024,#35025,#35026,#35027,#35028,#35029,#35030,#35031,#35032,#35033,#35034,
#35035,#35036,#35037),(#35038,#35039,#35040,#35041,#35042,#35043,#35044,
#35045,#35046,#35047,#35048,#35049,#35050,#35051,#35052,#35053,#35054),
(#35055,#35056,#35057,#35058,#35059,#35060,#35061,#35062,#35063,#35064,
#35065,#35066,#35067,#35068,#35069,#35070,#35071)),.UNSPECIFIED.,.F.,.F.,
 .F.,(4,2,1,1,1,1,1,1,1,1,1,2,4),(4,2,1,1,1,1,1,1,1,1,1,2,4),(-0.0353050121574204,
0.,0.0909090909090909,0.181818181818182,0.272727272727273,0.409090909090909,
0.5,0.590909090909091,0.727272727272727,0.818181818181818,0.909090909090909,
1.,1.03479194496591),(-0.021689269548343,0.,0.0708639855735204,0.141727971147041,
0.212591956720561,0.318887935080842,0.389751920654362,0.460615906227882,
0.566911884588163,0.637775870161683,0.708639855735204,0.779503841308724,
0.801875267322681),.UNSPECIFIED.);
#253=B_SPLINE_SURFACE_WITH_KNOTS('',3,3,((#35115,#35116,#35117,#35118,#35119,
#35120,#35121,#35122,#35123,#35124,#35125,#35126,#35127,#35128,#35129,#35130,
#35131),(#35132,#35133,#35134,#35135,#35136,#35137,#35138,#35139,#35140,
#35141,#35142,#35143,#35144,#35145,#35146,#35147,#35148),(#35149,#35150,
#35151,#35152,#35153,#35154,#35155,#35156,#35157,#35158,#35159,#35160,#35161,
#35162,#35163,#35164,#35165),(#35166,#35167,#35168,#35169,#35170,#35171,
#35172,#35173,#35174,#35175,#35176,#35177,#35178,#35179,#35180,#35181,#35182),
(#35183,#35184,#35185,#35186,#35187,#35188,#35189,#35190,#35191,#35192,
#35193,#35194,#35195,#35196,#35197,#35198,#35199),(#35200,#35201,#35202,
#35203,#35204,#35205,#35206,#35207,#35208,#35209,#35210,#35211,#35212,#35213,
#35214,#35215,#35216),(#35217,#35218,#35219,#35220,#35221,#35222,#35223,
#35224,#35225,#35226,#35227,#35228,#35229,#35230,#35231,#35232,#35233),
(#35234,#35235,#35236,#35237,#35238,#35239,#35240,#35241,#35242,#35243,
#35244,#35245,#35246,#35247,#35248,#35249,#35250),(#35251,#35252,#35253,
#35254,#35255,#35256,#35257,#35258,#35259,#35260,#35261,#35262,#35263,#35264,
#35265,#35266,#35267),(#35268,#35269,#35270,#35271,#35272,#35273,#35274,
#35275,#35276,#35277,#35278,#35279,#35280,#35281,#35282,#35283,#35284),
(#35285,#35286,#35287,#35288,#35289,#35290,#35291,#35292,#35293,#35294,
#35295,#35296,#35297,#35298,#35299,#35300,#35301),(#35302,#35303,#35304,
#35305,#35306,#35307,#35308,#35309,#35310,#35311,#35312,#35313,#35314,#35315,
#35316,#35317,#35318),(#35319,#35320,#35321,#35322,#35323,#35324,#35325,
#35326,#35327,#35328,#35329,#35330,#35331,#35332,#35333,#35334,#35335),
(#35336,#35337,#35338,#35339,#35340,#35341,#35342,#35343,#35344,#35345,
#35346,#35347,#35348,#35349,#35350,#35351,#35352),(#35353,#35354,#35355,
#35356,#35357,#35358,#35359,#35360,#35361,#35362,#35363,#35364,#35365,#35366,
#35367,#35368,#35369),(#35370,#35371,#35372,#35373,#35374,#35375,#35376,
#35377,#35378,#35379,#35380,#35381,#35382,#35383,#35384,#35385,#35386)),
 .UNSPECIFIED.,.F.,.F.,.F.,(4,2,1,1,1,1,1,1,1,1,2,4),(4,2,1,1,1,1,1,1,1,
1,1,2,4),(-0.035701835836904,0.,0.090219017653024,0.22554754413256,0.315766561785584,
0.45109508826512,0.541314105918144,0.67664263239768,0.766861650050704,0.90219017653024,
0.992409194183265,1.02810227746674),(-0.0217729438654334,0.,0.0708639855735204,
0.141727971147041,0.212591956720561,0.318887935080842,0.389751920654362,
0.460615906227882,0.566911884588163,0.637775870161683,0.708639855735204,
0.779503841308724,0.801994948010107),.UNSPECIFIED.);
#254=B_SPLINE_SURFACE_WITH_KNOTS('',3,3,((#35402,#35403,#35404,#35405,#35406,
#35407,#35408),(#35409,#35410,#35411,#35412,#35413,#35414,#35415),(#35416,
#35417,#35418,#35419,#35420,#35421,#35422),(#35423,#35424,#35425,#35426,
#35427,#35428,#35429),(#35430,#35431,#35432,#35433,#35434,#35435,#35436),
(#35437,#35438,#35439,#35440,#35441,#35442,#35443),(#35444,#35445,#35446,
#35447,#35448,#35449,#35450),(#35451,#35452,#35453,#35454,#35455,#35456,
#35457),(#35458,#35459,#35460,#35461,#35462,#35463,#35464),(#35465,#35466,
#35467,#35468,#35469,#35470,#35471),(#35472,#35473,#35474,#35475,#35476,
#35477,#35478),(#35479,#35480,#35481,#35482,#35483,#35484,#35485),(#35486,
#35487,#35488,#35489,#35490,#35491,#35492)),.UNSPECIFIED.,.F.,.F.,.F.,(4,
3,1,1,1,3,4),(4,3,4),(0.991784279387784,0.992409194183265,0.994306895637448,
0.996204597091632,0.998102298545816,1.,1.0001828629104),(-0.00779503841308724,
0.,0.779503841308724),.UNSPECIFIED.);
#255=B_SPLINE_SURFACE_WITH_KNOTS('',3,3,((#35494,#35495,#35496,#35497,#35498,
#35499,#35500,#35501,#35502,#35503,#35504,#35505,#35506,#35507,#35508,#35509,
#35510),(#35511,#35512,#35513,#35514,#35515,#35516,#35517,#35518,#35519,
#35520,#35521,#35522,#35523,#35524,#35525,#35526,#35527),(#35528,#35529,
#35530,#35531,#35532,#35533,#35534,#35535,#35536,#35537,#35538,#35539,#35540,
#35541,#35542,#35543,#35544),(#35545,#35546,#35547,#35548,#35549,#35550,
#35551,#35552,#35553,#35554,#35555,#35556,#35557,#35558,#35559,#35560,#35561),
(#35562,#35563,#35564,#35565,#35566,#35567,#35568,#35569,#35570,#35571,
#35572,#35573,#35574,#35575,#35576,#35577,#35578),(#35579,#35580,#35581,
#35582,#35583,#35584,#35585,#35586,#35587,#35588,#35589,#35590,#35591,#35592,
#35593,#35594,#35595),(#35596,#35597,#35598,#35599,#35600,#35601,#35602,
#35603,#35604,#35605,#35606,#35607,#35608,#35609,#35610,#35611,#35612),
(#35613,#35614,#35615,#35616,#35617,#35618,#35619,#35620,#35621,#35622,
#35623,#35624,#35625,#35626,#35627,#35628,#35629),(#35630,#35631,#35632,
#35633,#35634,#35635,#35636,#35637,#35638,#35639,#35640,#35641,#35642,#35643,
#35644,#35645,#35646),(#35647,#35648,#35649,#35650,#35651,#35652,#35653,
#35654,#35655,#35656,#35657,#35658,#35659,#35660,#35661,#35662,#35663),
(#35664,#35665,#35666,#35667,#35668,#35669,#35670,#35671,#35672,#35673,
#35674,#35675,#35676,#35677,#35678,#35679,#35680),(#35681,#35682,#35683,
#35684,#35685,#35686,#35687,#35688,#35689,#35690,#35691,#35692,#35693,#35694,
#35695,#35696,#35697),(#35698,#35699,#35700,#35701,#35702,#35703,#35704,
#35705,#35706,#35707,#35708,#35709,#35710,#35711,#35712,#35713,#35714),
(#35715,#35716,#35717,#35718,#35719,#35720,#35721,#35722,#35723,#35724,
#35725,#35726,#35727,#35728,#35729,#35730,#35731),(#35732,#35733,#35734,
#35735,#35736,#35737,#35738,#35739,#35740,#35741,#35742,#35743,#35744,#35745,
#35746,#35747,#35748),(#35749,#35750,#35751,#35752,#35753,#35754,#35755,
#35756,#35757,#35758,#35759,#35760,#35761,#35762,#35763,#35764,#35765),
(#35766,#35767,#35768,#35769,#35770,#35771,#35772,#35773,#35774,#35775,
#35776,#35777,#35778,#35779,#35780,#35781,#35782)),.UNSPECIFIED.,.F.,.F.,
 .F.,(4,2,1,1,1,1,1,1,1,1,1,2,4),(4,2,1,1,1,1,1,1,1,1,1,2,4),(-0.0353050121574204,
0.,0.0909090909090909,0.181818181818182,0.272727272727273,0.409090909090909,
0.5,0.590909090909091,0.727272727272727,0.818181818181818,0.909090909090909,
1.,1.03479194496591),(-0.021689269548343,0.,0.0708639855735204,0.141727971147041,
0.212591956720561,0.318887935080842,0.389751920654362,0.460615906227882,
0.566911884588163,0.637775870161683,0.708639855735204,0.779503841308724,
0.801875267322681),.UNSPECIFIED.);
#256=B_SPLINE_SURFACE_WITH_KNOTS('',3,3,((#35814,#35815,#35816,#35817,#35818,
#35819,#35820,#35821,#35822,#35823,#35824,#35825,#35826,#35827,#35828,#35829,
#35830),(#35831,#35832,#35833,#35834,#35835,#35836,#35837,#35838,#35839,
#35840,#35841,#35842,#35843,#35844,#35845,#35846,#35847),(#35848,#35849,
#35850,#35851,#35852,#35853,#35854,#35855,#35856,#35857,#35858,#35859,#35860,
#35861,#35862,#35863,#35864),(#35865,#35866,#35867,#35868,#35869,#35870,
#35871,#35872,#35873,#35874,#35875,#35876,#35877,#35878,#35879,#35880,#35881),
(#35882,#35883,#35884,#35885,#35886,#35887,#35888,#35889,#35890,#35891,
#35892,#35893,#35894,#35895,#35896,#35897,#35898),(#35899,#35900,#35901,
#35902,#35903,#35904,#35905,#35906,#35907,#35908,#35909,#35910,#35911,#35912,
#35913,#35914,#35915),(#35916,#35917,#35918,#35919,#35920,#35921,#35922,
#35923,#35924,#35925,#35926,#35927,#35928,#35929,#35930,#35931,#35932),
(#35933,#35934,#35935,#35936,#35937,#35938,#35939,#35940,#35941,#35942,
#35943,#35944,#35945,#35946,#35947,#35948,#35949),(#35950,#35951,#35952,
#35953,#35954,#35955,#35956,#35957,#35958,#35959,#35960,#35961,#35962,#35963,
#35964,#35965,#35966),(#35967,#35968,#35969,#35970,#35971,#35972,#35973,
#35974,#35975,#35976,#35977,#35978,#35979,#35980,#35981,#35982,#35983),
(#35984,#35985,#35986,#35987,#35988,#35989,#35990,#35991,#35992,#35993,
#35994,#35995,#35996,#35997,#35998,#35999,#36000),(#36001,#36002,#36003,
#36004,#36005,#36006,#36007,#36008,#36009,#36010,#36011,#36012,#36013,#36014,
#36015,#36016,#36017),(#36018,#36019,#36020,#36021,#36022,#36023,#36024,
#36025,#36026,#36027,#36028,#36029,#36030,#36031,#36032,#36033,#36034),
(#36035,#36036,#36037,#36038,#36039,#36040,#36041,#36042,#36043,#36044,
#36045,#36046,#36047,#36048,#36049,#36050,#36051),(#36052,#36053,#36054,
#36055,#36056,#36057,#36058,#36059,#36060,#36061,#36062,#36063,#36064,#36065,
#36066,#36067,#36068),(#36069,#36070,#36071,#36072,#36073,#36074,#36075,
#36076,#36077,#36078,#36079,#36080,#36081,#36082,#36083,#36084,#36085)),
 .UNSPECIFIED.,.F.,.F.,.F.,(4,2,1,1,1,1,1,1,1,1,2,4),(4,2,1,1,1,1,1,1,1,
1,1,2,4),(-0.035701835836904,0.,0.090219017653024,0.22554754413256,0.315766561785584,
0.45109508826512,0.541314105918144,0.67664263239768,0.766861650050704,0.90219017653024,
0.992409194183265,1.02810227746674),(-0.0217729438654334,0.,0.0708639855735204,
0.141727971147041,0.212591956720561,0.318887935080842,0.389751920654362,
0.460615906227882,0.566911884588163,0.637775870161683,0.708639855735204,
0.779503841308724,0.801994948010107),.UNSPECIFIED.);
#257=B_SPLINE_SURFACE_WITH_KNOTS('',3,3,((#36092,#36093,#36094,#36095,#36096,
#36097,#36098),(#36099,#36100,#36101,#36102,#36103,#36104,#36105),(#36106,
#36107,#36108,#36109,#36110,#36111,#36112),(#36113,#36114,#36115,#36116,
#36117,#36118,#36119),(#36120,#36121,#36122,#36123,#36124,#36125,#36126),
(#36127,#36128,#36129,#36130,#36131,#36132,#36133),(#36134,#36135,#36136,
#36137,#36138,#36139,#36140),(#36141,#36142,#36143,#36144,#36145,#36146,
#36147),(#36148,#36149,#36150,#36151,#36152,#36153,#36154),(#36155,#36156,
#36157,#36158,#36159,#36160,#36161),(#36162,#36163,#36164,#36165,#36166,
#36167,#36168),(#36169,#36170,#36171,#36172,#36173,#36174,#36175),(#36176,
#36177,#36178,#36179,#36180,#36181,#36182)),.UNSPECIFIED.,.F.,.F.,.F.,(4,
3,1,1,1,3,4),(4,3,4),(0.991784279387784,0.992409194183265,0.994306895637448,
0.996204597091632,0.998102298545816,1.,1.0001828629104),(-0.00779503841308724,
0.,0.779503841308724),.UNSPECIFIED.);
#258=B_SPLINE_SURFACE_WITH_KNOTS('',3,3,((#36183,#36184,#36185,#36186,#36187,
#36188,#36189,#36190,#36191,#36192,#36193,#36194,#36195,#36196,#36197,#36198,
#36199),(#36200,#36201,#36202,#36203,#36204,#36205,#36206,#36207,#36208,
#36209,#36210,#36211,#36212,#36213,#36214,#36215,#36216),(#36217,#36218,
#36219,#36220,#36221,#36222,#36223,#36224,#36225,#36226,#36227,#36228,#36229,
#36230,#36231,#36232,#36233),(#36234,#36235,#36236,#36237,#36238,#36239,
#36240,#36241,#36242,#36243,#36244,#36245,#36246,#36247,#36248,#36249,#36250),
(#36251,#36252,#36253,#36254,#36255,#36256,#36257,#36258,#36259,#36260,
#36261,#36262,#36263,#36264,#36265,#36266,#36267),(#36268,#36269,#36270,
#36271,#36272,#36273,#36274,#36275,#36276,#36277,#36278,#36279,#36280,#36281,
#36282,#36283,#36284),(#36285,#36286,#36287,#36288,#36289,#36290,#36291,
#36292,#36293,#36294,#36295,#36296,#36297,#36298,#36299,#36300,#36301),
(#36302,#36303,#36304,#36305,#36306,#36307,#36308,#36309,#36310,#36311,
#36312,#36313,#36314,#36315,#36316,#36317,#36318),(#36319,#36320,#36321,
#36322,#36323,#36324,#36325,#36326,#36327,#36328,#36329,#36330,#36331,#36332,
#36333,#36334,#36335),(#36336,#36337,#36338,#36339,#36340,#36341,#36342,
#36343,#36344,#36345,#36346,#36347,#36348,#36349,#36350,#36351,#36352),
(#36353,#36354,#36355,#36356,#36357,#36358,#36359,#36360,#36361,#36362,
#36363,#36364,#36365,#36366,#36367,#36368,#36369),(#36370,#36371,#36372,
#36373,#36374,#36375,#36376,#36377,#36378,#36379,#36380,#36381,#36382,#36383,
#36384,#36385,#36386),(#36387,#36388,#36389,#36390,#36391,#36392,#36393,
#36394,#36395,#36396,#36397,#36398,#36399,#36400,#36401,#36402,#36403),
(#36404,#36405,#36406,#36407,#36408,#36409,#36410,#36411,#36412,#36413,
#36414,#36415,#36416,#36417,#36418,#36419,#36420),(#36421,#36422,#36423,
#36424,#36425,#36426,#36427,#36428,#36429,#36430,#36431,#36432,#36433,#36434,
#36435,#36436,#36437),(#36438,#36439,#36440,#36441,#36442,#36443,#36444,
#36445,#36446,#36447,#36448,#36449,#36450,#36451,#36452,#36453,#36454),
(#36455,#36456,#36457,#36458,#36459,#36460,#36461,#36462,#36463,#36464,
#36465,#36466,#36467,#36468,#36469,#36470,#36471)),.UNSPECIFIED.,.F.,.F.,
 .F.,(4,2,1,1,1,1,1,1,1,1,1,2,4),(4,2,1,1,1,1,1,1,1,1,1,2,4),(-0.0353050121574204,
0.,0.0909090909090909,0.181818181818182,0.272727272727273,0.409090909090909,
0.5,0.590909090909091,0.727272727272727,0.818181818181818,0.909090909090909,
1.,1.03479194496591),(-0.021689269548343,0.,0.0708639855735204,0.141727971147041,
0.212591956720561,0.318887935080842,0.389751920654362,0.460615906227882,
0.566911884588163,0.637775870161683,0.708639855735204,0.779503841308724,
0.801875267322681),.UNSPECIFIED.);
#259=B_SPLINE_SURFACE_WITH_KNOTS('',3,3,((#36515,#36516,#36517,#36518,#36519,
#36520,#36521,#36522,#36523,#36524,#36525,#36526,#36527,#36528,#36529,#36530,
#36531),(#36532,#36533,#36534,#36535,#36536,#36537,#36538,#36539,#36540,
#36541,#36542,#36543,#36544,#36545,#36546,#36547,#36548),(#36549,#36550,
#36551,#36552,#36553,#36554,#36555,#36556,#36557,#36558,#36559,#36560,#36561,
#36562,#36563,#36564,#36565),(#36566,#36567,#36568,#36569,#36570,#36571,
#36572,#36573,#36574,#36575,#36576,#36577,#36578,#36579,#36580,#36581,#36582),
(#36583,#36584,#36585,#36586,#36587,#36588,#36589,#36590,#36591,#36592,
#36593,#36594,#36595,#36596,#36597,#36598,#36599),(#36600,#36601,#36602,
#36603,#36604,#36605,#36606,#36607,#36608,#36609,#36610,#36611,#36612,#36613,
#36614,#36615,#36616),(#36617,#36618,#36619,#36620,#36621,#36622,#36623,
#36624,#36625,#36626,#36627,#36628,#36629,#36630,#36631,#36632,#36633),
(#36634,#36635,#36636,#36637,#36638,#36639,#36640,#36641,#36642,#36643,
#36644,#36645,#36646,#36647,#36648,#36649,#36650),(#36651,#36652,#36653,
#36654,#36655,#36656,#36657,#36658,#36659,#36660,#36661,#36662,#36663,#36664,
#36665,#36666,#36667),(#36668,#36669,#36670,#36671,#36672,#36673,#36674,
#36675,#36676,#36677,#36678,#36679,#36680,#36681,#36682,#36683,#36684),
(#36685,#36686,#36687,#36688,#36689,#36690,#36691,#36692,#36693,#36694,
#36695,#36696,#36697,#36698,#36699,#36700,#36701),(#36702,#36703,#36704,
#36705,#36706,#36707,#36708,#36709,#36710,#36711,#36712,#36713,#36714,#36715,
#36716,#36717,#36718),(#36719,#36720,#36721,#36722,#36723,#36724,#36725,
#36726,#36727,#36728,#36729,#36730,#36731,#36732,#36733,#36734,#36735),
(#36736,#36737,#36738,#36739,#36740,#36741,#36742,#36743,#36744,#36745,
#36746,#36747,#36748,#36749,#36750,#36751,#36752),(#36753,#36754,#36755,
#36756,#36757,#36758,#36759,#36760,#36761,#36762,#36763,#36764,#36765,#36766,
#36767,#36768,#36769),(#36770,#36771,#36772,#36773,#36774,#36775,#36776,
#36777,#36778,#36779,#36780,#36781,#36782,#36783,#36784,#36785,#36786)),
 .UNSPECIFIED.,.F.,.F.,.F.,(4,2,1,1,1,1,1,1,1,1,2,4),(4,2,1,1,1,1,1,1,1,
1,1,2,4),(-0.035701835836904,0.,0.090219017653024,0.22554754413256,0.315766561785584,
0.45109508826512,0.541314105918144,0.67664263239768,0.766861650050704,0.90219017653024,
0.992409194183265,1.02810227746674),(-0.0217729438654334,0.,0.0708639855735204,
0.141727971147041,0.212591956720561,0.318887935080842,0.389751920654362,
0.460615906227882,0.566911884588163,0.637775870161683,0.708639855735204,
0.779503841308724,0.801994948010107),.UNSPECIFIED.);
#260=B_SPLINE_SURFACE_WITH_KNOTS('',3,3,((#36802,#36803,#36804,#36805,#36806,
#36807,#36808),(#36809,#36810,#36811,#36812,#36813,#36814,#36815),(#36816,
#36817,#36818,#36819,#36820,#36821,#36822),(#36823,#36824,#36825,#36826,
#36827,#36828,#36829),(#36830,#36831,#36832,#36833,#36834,#36835,#36836),
(#36837,#36838,#36839,#36840,#36841,#36842,#36843),(#36844,#36845,#36846,
#36847,#36848,#36849,#36850),(#36851,#36852,#36853,#36854,#36855,#36856,
#36857),(#36858,#36859,#36860,#36861,#36862,#36863,#36864),(#36865,#36866,
#36867,#36868,#36869,#36870,#36871),(#36872,#36873,#36874,#36875,#36876,
#36877,#36878),(#36879,#36880,#36881,#36882,#36883,#36884,#36885),(#36886,
#36887,#36888,#36889,#36890,#36891,#36892)),.UNSPECIFIED.,.F.,.F.,.F.,(4,
3,1,1,1,3,4),(4,3,4),(0.991784279387784,0.992409194183265,0.994306895637448,
0.996204597091632,0.998102298545816,1.,1.0001828629104),(-0.00779503841308724,
0.,0.779503841308724),.UNSPECIFIED.);
#261=B_SPLINE_SURFACE_WITH_KNOTS('',3,3,((#36894,#36895,#36896,#36897,#36898,
#36899,#36900,#36901,#36902,#36903,#36904,#36905,#36906,#36907,#36908,#36909,
#36910),(#36911,#36912,#36913,#36914,#36915,#36916,#36917,#36918,#36919,
#36920,#36921,#36922,#36923,#36924,#36925,#36926,#36927),(#36928,#36929,
#36930,#36931,#36932,#36933,#36934,#36935,#36936,#36937,#36938,#36939,#36940,
#36941,#36942,#36943,#36944),(#36945,#36946,#36947,#36948,#36949,#36950,
#36951,#36952,#36953,#36954,#36955,#36956,#36957,#36958,#36959,#36960,#36961),
(#36962,#36963,#36964,#36965,#36966,#36967,#36968,#36969,#36970,#36971,
#36972,#36973,#36974,#36975,#36976,#36977,#36978),(#36979,#36980,#36981,
#36982,#36983,#36984,#36985,#36986,#36987,#36988,#36989,#36990,#36991,#36992,
#36993,#36994,#36995),(#36996,#36997,#36998,#36999,#37000,#37001,#37002,
#37003,#37004,#37005,#37006,#37007,#37008,#37009,#37010,#37011,#37012),
(#37013,#37014,#37015,#37016,#37017,#37018,#37019,#37020,#37021,#37022,
#37023,#37024,#37025,#37026,#37027,#37028,#37029),(#37030,#37031,#37032,
#37033,#37034,#37035,#37036,#37037,#37038,#37039,#37040,#37041,#37042,#37043,
#37044,#37045,#37046),(#37047,#37048,#37049,#37050,#37051,#37052,#37053,
#37054,#37055,#37056,#37057,#37058,#37059,#37060,#37061,#37062,#37063),
(#37064,#37065,#37066,#37067,#37068,#37069,#37070,#37071,#37072,#37073,
#37074,#37075,#37076,#37077,#37078,#37079,#37080),(#37081,#37082,#37083,
#37084,#37085,#37086,#37087,#37088,#37089,#37090,#37091,#37092,#37093,#37094,
#37095,#37096,#37097),(#37098,#37099,#37100,#37101,#37102,#37103,#37104,
#37105,#37106,#37107,#37108,#37109,#37110,#37111,#37112,#37113,#37114),
(#37115,#37116,#37117,#37118,#37119,#37120,#37121,#37122,#37123,#37124,
#37125,#37126,#37127,#37128,#37129,#37130,#37131),(#37132,#37133,#37134,
#37135,#37136,#37137,#37138,#37139,#37140,#37141,#37142,#37143,#37144,#37145,
#37146,#37147,#37148),(#37149,#37150,#37151,#37152,#37153,#37154,#37155,
#37156,#37157,#37158,#37159,#37160,#37161,#37162,#37163,#37164,#37165),
(#37166,#37167,#37168,#37169,#37170,#37171,#37172,#37173,#37174,#37175,
#37176,#37177,#37178,#37179,#37180,#37181,#37182)),.UNSPECIFIED.,.F.,.F.,
 .F.,(4,2,1,1,1,1,1,1,1,1,1,2,4),(4,2,1,1,1,1,1,1,1,1,1,2,4),(-0.0353050121574204,
0.,0.0909090909090909,0.181818181818182,0.272727272727273,0.409090909090909,
0.5,0.590909090909091,0.727272727272727,0.818181818181818,0.909090909090909,
1.,1.03479194496591),(-0.021689269548343,0.,0.0708639855735204,0.141727971147041,
0.212591956720561,0.318887935080842,0.389751920654362,0.460615906227882,
0.566911884588163,0.637775870161683,0.708639855735204,0.779503841308724,
0.801875267322681),.UNSPECIFIED.);
#262=B_SPLINE_SURFACE_WITH_KNOTS('',3,3,((#37226,#37227,#37228,#37229,#37230,
#37231,#37232,#37233,#37234,#37235,#37236,#37237,#37238,#37239,#37240,#37241,
#37242),(#37243,#37244,#37245,#37246,#37247,#37248,#37249,#37250,#37251,
#37252,#37253,#37254,#37255,#37256,#37257,#37258,#37259),(#37260,#37261,
#37262,#37263,#37264,#37265,#37266,#37267,#37268,#37269,#37270,#37271,#37272,
#37273,#37274,#37275,#37276),(#37277,#37278,#37279,#37280,#37281,#37282,
#37283,#37284,#37285,#37286,#37287,#37288,#37289,#37290,#37291,#37292,#37293),
(#37294,#37295,#37296,#37297,#37298,#37299,#37300,#37301,#37302,#37303,
#37304,#37305,#37306,#37307,#37308,#37309,#37310),(#37311,#37312,#37313,
#37314,#37315,#37316,#37317,#37318,#37319,#37320,#37321,#37322,#37323,#37324,
#37325,#37326,#37327),(#37328,#37329,#37330,#37331,#37332,#37333,#37334,
#37335,#37336,#37337,#37338,#37339,#37340,#37341,#37342,#37343,#37344),
(#37345,#37346,#37347,#37348,#37349,#37350,#37351,#37352,#37353,#37354,
#37355,#37356,#37357,#37358,#37359,#37360,#37361),(#37362,#37363,#37364,
#37365,#37366,#37367,#37368,#37369,#37370,#37371,#37372,#37373,#37374,#37375,
#37376,#37377,#37378),(#37379,#37380,#37381,#37382,#37383,#37384,#37385,
#37386,#37387,#37388,#37389,#37390,#37391,#37392,#37393,#37394,#37395),
(#37396,#37397,#37398,#37399,#37400,#37401,#37402,#37403,#37404,#37405,
#37406,#37407,#37408,#37409,#37410,#37411,#37412),(#37413,#37414,#37415,
#37416,#37417,#37418,#37419,#37420,#37421,#37422,#37423,#37424,#37425,#37426,
#37427,#37428,#37429),(#37430,#37431,#37432,#37433,#37434,#37435,#37436,
#37437,#37438,#37439,#37440,#37441,#37442,#37443,#37444,#37445,#37446),
(#37447,#37448,#37449,#37450,#37451,#37452,#37453,#37454,#37455,#37456,
#37457,#37458,#37459,#37460,#37461,#37462,#37463),(#37464,#37465,#37466,
#37467,#37468,#37469,#37470,#37471,#37472,#37473,#37474,#37475,#37476,#37477,
#37478,#37479,#37480),(#37481,#37482,#37483,#37484,#37485,#37486,#37487,
#37488,#37489,#37490,#37491,#37492,#37493,#37494,#37495,#37496,#37497)),
 .UNSPECIFIED.,.F.,.F.,.F.,(4,2,1,1,1,1,1,1,1,1,2,4),(4,2,1,1,1,1,1,1,1,
1,1,2,4),(-0.035701835836904,0.,0.090219017653024,0.22554754413256,0.315766561785584,
0.45109508826512,0.541314105918144,0.67664263239768,0.766861650050704,0.90219017653024,
0.992409194183265,1.02810227746674),(-0.0217729438654334,0.,0.0708639855735204,
0.141727971147041,0.212591956720561,0.318887935080842,0.389751920654362,
0.460615906227882,0.566911884588163,0.637775870161683,0.708639855735204,
0.779503841308724,0.801994948010107),.UNSPECIFIED.);
#263=B_SPLINE_SURFACE_WITH_KNOTS('',3,3,((#37513,#37514,#37515,#37516,#37517,
#37518,#37519),(#37520,#37521,#37522,#37523,#37524,#37525,#37526),(#37527,
#37528,#37529,#37530,#37531,#37532,#37533),(#37534,#37535,#37536,#37537,
#37538,#37539,#37540),(#37541,#37542,#37543,#37544,#37545,#37546,#37547),
(#37548,#37549,#37550,#37551,#37552,#37553,#37554),(#37555,#37556,#37557,
#37558,#37559,#37560,#37561),(#37562,#37563,#37564,#37565,#37566,#37567,
#37568),(#37569,#37570,#37571,#37572,#37573,#37574,#37575),(#37576,#37577,
#37578,#37579,#37580,#37581,#37582),(#37583,#37584,#37585,#37586,#37587,
#37588,#37589),(#37590,#37591,#37592,#37593,#37594,#37595,#37596),(#37597,
#37598,#37599,#37600,#37601,#37602,#37603)),.UNSPECIFIED.,.F.,.F.,.F.,(4,
3,1,1,1,3,4),(4,3,4),(0.991784279387784,0.992409194183265,0.994306895637448,
0.996204597091632,0.998102298545816,1.,1.0001828629104),(-0.00779503841308724,
0.,0.779503841308724),.UNSPECIFIED.);
#264=ELLIPSE('',#11887,72.7371534489403,59.3518142583655);
#265=ELLIPSE('',#11888,72.7371534278831,59.3518142500034);
#266=ELLIPSE('',#11890,72.7371534418997,59.3518142555308);
#267=ELLIPSE('',#11891,72.7371534042391,59.3518142403299);
#268=ELLIPSE('',#11893,72.7371534315122,59.3518142517928);
#269=ELLIPSE('',#11894,72.7371534760386,59.3518142697471);
#270=ELLIPSE('',#11896,72.7371534484564,59.3518142581681);
#271=ELLIPSE('',#11897,72.7371534338909,59.351814252458);
#272=ELLIPSE('',#11900,267.033279968916,3.97556846403247);
#273=ELLIPSE('',#11988,72.7371534233152,59.3518142481207);
#274=ELLIPSE('',#11989,72.7371534254535,59.3518142493252);
#275=ELLIPSE('',#11991,72.7371534314927,59.3518142515694);
#276=ELLIPSE('',#11992,72.7371534149343,59.351814244469);
#277=ELLIPSE('',#12027,267.033273104505,3.97556839267334);
#278=ELLIPSE('',#12068,72.7371534238836,59.3518142483897);
#279=ELLIPSE('',#12069,72.737153424688,59.3518142489889);
#280=ELLIPSE('',#12102,267.033281117203,3.97556847604632);
#281=ELLIPSE('',#12131,72.7371533930096,59.3518142357707);
#282=ELLIPSE('',#12132,72.7371534556984,59.3518142616426);
#283=ELLIPSE('',#12166,267.033271548161,3.97556837688584);
#284=FACE_BOUND('',#1832,.T.);
#285=FACE_BOUND('',#1833,.T.);
#286=FACE_BOUND('',#1834,.T.);
#287=FACE_BOUND('',#1835,.T.);
#288=FACE_BOUND('',#1836,.T.);
#289=FACE_BOUND('',#1837,.T.);
#290=FACE_BOUND('',#1838,.T.);
#291=FACE_BOUND('',#1839,.T.);
#292=FACE_BOUND('',#1843,.T.);
#293=FACE_BOUND('',#1845,.T.);
#294=FACE_BOUND('',#1857,.T.);
#295=FACE_BOUND('',#1873,.T.);
#296=FACE_BOUND('',#1875,.T.);
#297=FACE_BOUND('',#1882,.T.);
#298=FACE_BOUND('',#1883,.T.);
#299=FACE_BOUND('',#1884,.T.);
#300=FACE_BOUND('',#1885,.T.);
#301=FACE_BOUND('',#1886,.T.);
#302=FACE_BOUND('',#1887,.T.);
#303=FACE_BOUND('',#1888,.T.);
#304=FACE_BOUND('',#1889,.T.);
#305=FACE_BOUND('',#1915,.T.);
#306=FACE_BOUND('',#1917,.T.);
#307=FACE_BOUND('',#1969,.T.);
#308=FACE_BOUND('',#1971,.T.);
#309=FACE_BOUND('',#2471,.T.);
#310=FACE_BOUND('',#2473,.T.);
#311=FACE_BOUND('',#2475,.T.);
#312=FACE_BOUND('',#2525,.T.);
#313=FACE_BOUND('',#2533,.T.);
#314=FACE_BOUND('',#2535,.T.);
#315=PLANE('',#11821);
#316=PLANE('',#11848);
#317=PLANE('',#11849);
#318=PLANE('',#11850);
#319=PLANE('',#11855);
#320=PLANE('',#11859);
#321=PLANE('',#11876);
#322=PLANE('',#11883);
#323=PLANE('',#11886);
#324=PLANE('',#11889);
#325=PLANE('',#11892);
#326=PLANE('',#11895);
#327=PLANE('',#11904);
#328=PLANE('',#11918);
#329=PLANE('',#11920);
#330=PLANE('',#11945);
#331=PLANE('',#11949);
#332=PLANE('',#11954);
#333=PLANE('',#11955);
#334=PLANE('',#11959);
#335=PLANE('',#11960);
#336=PLANE('',#11961);
#337=PLANE('',#11987);
#338=PLANE('',#11990);
#339=PLANE('',#11993);
#340=PLANE('',#11994);
#341=PLANE('',#11998);
#342=PLANE('',#12001);
#343=PLANE('',#12002);
#344=PLANE('',#12005);
#345=PLANE('',#12009);
#346=PLANE('',#12010);
#347=PLANE('',#12011);
#348=PLANE('',#12031);
#349=PLANE('',#12033);
#350=PLANE('',#12047);
#351=PLANE('',#12051);
#352=PLANE('',#12056);
#353=PLANE('',#12060);
#354=PLANE('',#12067);
#355=PLANE('',#12070);
#356=PLANE('',#12071);
#357=PLANE('',#12075);
#358=PLANE('',#12078);
#359=PLANE('',#12079);
#360=PLANE('',#12082);
#361=PLANE('',#12086);
#362=PLANE('',#12087);
#363=PLANE('',#12088);
#364=PLANE('',#12106);
#365=PLANE('',#12108);
#366=PLANE('',#12119);
#367=PLANE('',#12123);
#368=PLANE('',#12130);
#369=PLANE('',#12133);
#370=PLANE('',#12134);
#371=PLANE('',#12138);
#372=PLANE('',#12141);
#373=PLANE('',#12142);
#374=PLANE('',#12145);
#375=PLANE('',#12149);
#376=PLANE('',#12150);
#377=PLANE('',#12151);
#378=PLANE('',#12170);
#379=PLANE('',#12172);
#380=PLANE('',#12179);
#381=PLANE('',#12184);
#382=PLANE('',#12197);
#383=PLANE('',#12198);
#384=PLANE('',#12202);
#385=PLANE('',#12205);
#386=PLANE('',#12206);
#387=PLANE('',#12209);
#388=PLANE('',#12213);
#389=PLANE('',#12214);
#390=PLANE('',#12215);
#391=PLANE('',#12926);
#392=PLANE('',#12927);
#393=PLANE('',#12929);
#394=PLANE('',#12930);
#395=PLANE('',#12931);
#396=PLANE('',#12932);
#397=PLANE('',#12933);
#398=PLANE('',#12934);
#399=PLANE('',#12935);
#400=PLANE('',#12936);
#401=PLANE('',#12937);
#402=PLANE('',#12938);
#403=PLANE('',#12939);
#404=PLANE('',#12940);
#405=PLANE('',#12941);
#406=PLANE('',#12942);
#407=PLANE('',#12943);
#408=PLANE('',#12944);
#409=PLANE('',#12945);
#410=PLANE('',#12946);
#411=PLANE('',#12947);
#412=PLANE('',#12948);
#413=PLANE('',#12949);
#414=PLANE('',#12980);
#415=PLANE('',#12981);
#416=PLANE('',#12988);
#417=PLANE('',#12989);
#418=PLANE('',#12990);
#419=B_SPLINE_CURVE_WITH_KNOTS('',3,(#16807,#16808,#16809,#16810,#16811,
#16812,#16813,#16814),.UNSPECIFIED.,.F.,.F.,(4,2,2,4),(0.,0.000625000000000717,
0.00312500000008064,0.00654794813346023),.UNSPECIFIED.);
#420=B_SPLINE_CURVE_WITH_KNOTS('',3,(#16818,#16819,#16820,#16821,#16822,
#16823,#16824,#16825,#16826,#16827),.UNSPECIFIED.,.F.,.F.,(4,2,2,2,4),(0.,
0.0110943326857293,0.016641499028594,0.0194150822000263,0.0221886653714586),
 .UNSPECIFIED.);
#421=B_SPLINE_CURVE_WITH_KNOTS('',3,(#16829,#16830,#16831,#16832,#16833,
#16834,#16835,#16836,#16837,#16838),.UNSPECIFIED.,.F.,.F.,(4,2,2,2,4),(0.0221886653714586,
0.0332305757457702,0.0359910533393481,0.038751530932926,0.0442724861200818),
 .UNSPECIFIED.);
#422=B_SPLINE_CURVE_WITH_KNOTS('',3,(#16841,#16842,#16843,#16844,#16845,
#16846,#16847,#16848),.UNSPECIFIED.,.F.,.F.,(4,2,2,4),(1.30968750346023E-17,
0.000625000000000436,0.00312500000006035,0.0065479481334553),
 .UNSPECIFIED.);
#423=B_SPLINE_CURVE_WITH_KNOTS('',3,(#16876,#16877,#16878,#16879,#16880,
#16881,#16882,#16883),.UNSPECIFIED.,.F.,.F.,(4,2,2,4),(0.,0.000625000000000718,
0.00312500000008064,0.00654794813346023),.UNSPECIFIED.);
#424=B_SPLINE_CURVE_WITH_KNOTS('',3,(#16887,#16888,#16889,#16890,#16891,
#16892,#16893,#16894,#16895,#16896),.UNSPECIFIED.,.F.,.F.,(4,2,2,2,4),(0.,
0.0110943326857293,0.016641499028594,0.0194150822000263,0.0221886653714587),
 .UNSPECIFIED.);
#425=B_SPLINE_CURVE_WITH_KNOTS('',3,(#16898,#16899,#16900,#16901,#16902,
#16903,#16904,#16905,#16906,#16907),.UNSPECIFIED.,.F.,.F.,(4,2,2,2,4),(0.0221886653714587,
0.0332305757457703,0.0359910533393482,0.0387515309329261,0.0442724861200819),
 .UNSPECIFIED.);
#426=B_SPLINE_CURVE_WITH_KNOTS('',3,(#16910,#16911,#16912,#16913,#16914,
#16915,#16916,#16917),.UNSPECIFIED.,.F.,.F.,(4,2,2,4),(1.7347234759768E-18,
0.000625000000000437,0.00312500000006035,0.00654794813345528),
 .UNSPECIFIED.);
#427=B_SPLINE_CURVE_WITH_KNOTS('',3,(#16951,#16952,#16953,#16954,#16955,
#16956,#16957,#16958,#16959,#16960,#16961,#16962,#16963,#16964,#16965,#16966,
#16967,#16968,#16969,#16970,#16971,#16972,#16973,#16974,#16975,#16976,#16977,
#16978,#16979,#16980,#16981,#16982,#16983,#16984,#16985,#16986,#16987,#16988,
#16989,#16990,#16991,#16992,#16993,#16994,#16995,#16996),.UNSPECIFIED.,
 .F.,.F.,(4,3,3,3,3,3,3,3,3,3,3,3,3,3,3,4),(0.,6.08280066317253E-5,0.000143504025129764,
0.000222132236425273,0.000243312026526901,0.000273726029842764,0.000390756960305233,
0.000486624053053802,0.000487092885051584,0.000652104140181452,0.000729936079580703,
0.000730491914653075,0.000807330947238038,0.000884197975618414,0.000957724799089441,
0.000973248106107605),.UNSPECIFIED.);
#428=B_SPLINE_CURVE_WITH_KNOTS('',3,(#17004,#17005,#17006,#17007,#17008,
#17009,#17010,#17011,#17012,#17013,#17014,#17015,#17016,#17017,#17018,#17019,
#17020,#17021,#17022,#17023,#17024,#17025,#17026,#17027,#17028,#17029,#17030,
#17031,#17032,#17033,#17034),.UNSPECIFIED.,.F.,.F.,(4,3,3,3,3,3,3,3,3,3,
4),(0.,0.000110044300705118,0.000227537679381867,0.000345953766308564,0.000459500393964181,
0.000506968361890626,0.000507607986069998,0.000621724537891899,0.000763599672892467,
0.000889140904463126,0.00101393672378125),.UNSPECIFIED.);
#429=B_SPLINE_CURVE_WITH_KNOTS('',3,(#17038,#17039,#17040,#17041,#17042,
#17043,#17044,#17045,#17046,#17047,#17048,#17049,#17050,#17051,#17052,#17053,
#17054,#17055,#17056,#17057,#17058,#17059,#17060,#17061,#17062,#17063,#17064,
#17065,#17066,#17067,#17068,#17069,#17070,#17071),.UNSPECIFIED.,.F.,.F.,
(4,3,3,3,3,3,3,3,3,3,3,4),(0.,9.75727287245357E-5,0.000197558568026697,
0.000263369830764718,0.000264501976385977,0.000410751214877331,0.000527720220099539,
0.000529003952771953,0.000711275183632117,0.000792685220207556,0.000986383339260414,
0.0010580079055439),.UNSPECIFIED.);
#430=B_SPLINE_CURVE_WITH_KNOTS('',3,(#17076,#17077,#17078,#17079,#17080,
#17081,#17082,#17083,#17084,#17085,#17086,#17087,#17088,#17089,#17090,#17091,
#17092,#17093,#17094,#17095,#17096,#17097,#17098,#17099,#17100,#17101,#17102,
#17103,#17104,#17105,#17106,#17107,#17108,#17109,#17110,#17111,#17112,#17113,
#17114,#17115,#17116,#17117,#17118),.UNSPECIFIED.,.F.,.F.,(4,3,3,3,3,3,
3,3,3,3,3,3,3,3,4),(0.,0.000122774773559688,0.000252172289553419,0.000391124229753653,
0.000417443869709968,0.000418563871648259,0.000739329890793104,0.000834887739419937,
0.000836592389993165,0.00109817436603959,0.0012523316091299,0.00125385075554294,
0.0014203606660688,0.0015569180076674,0.00166977547883987),
 .UNSPECIFIED.);
#431=B_SPLINE_CURVE_WITH_KNOTS('',3,(#17128,#17129,#17130,#17131,#17132,
#17133,#17134,#17135,#17136,#17137,#17138,#17139,#17140,#17141,#17142,#17143,
#17144,#17145,#17146,#17147,#17148,#17149,#17150,#17151,#17152,#17153,#17154,
#17155,#17156,#17157,#17158,#17159,#17160,#17161,#17162,#17163,#17164,#17165,
#17166,#17167,#17168,#17169,#17170,#17171,#17172,#17173),.UNSPECIFIED.,
 .F.,.F.,(4,3,3,3,3,3,3,3,3,3,3,3,3,3,3,4),(0.,6.0828006631726E-5,0.000143504025135297,
0.000222132236434781,0.000243312026526904,0.000273726029842767,0.000390756960268089,
0.000486624053053808,0.000487092885051566,0.000652104140206423,0.000729936079580712,
0.000730491914653054,0.000807330947229213,0.000884197975603245,0.000957724799069373,
0.000973248106107616),.UNSPECIFIED.);
#432=B_SPLINE_CURVE_WITH_KNOTS('',3,(#17178,#17179,#17180,#17181,#17182,
#17183,#17184,#17185,#17186,#17187,#17188,#17189,#17190,#17191,#17192,#17193,
#17194,#17195,#17196,#17197,#17198,#17199,#17200,#17201,#17202,#17203,#17204,
#17205,#17206,#17207,#17208),.UNSPECIFIED.,.F.,.F.,(4,3,3,3,3,3,3,3,3,3,
4),(0.,0.000110044300698099,0.000227537679367299,0.00034595376628619,0.000459500393933875,
0.000506968361890626,0.000507607986070002,0.000621724537891888,0.00076359967287861,
0.000889140904441178,0.00101393672378125),.UNSPECIFIED.);
#433=B_SPLINE_CURVE_WITH_KNOTS('',3,(#17212,#17213,#17214,#17215,#17216,
#17217,#17218,#17219,#17220,#17221,#17222,#17223,#17224,#17225,#17226,#17227,
#17228,#17229,#17230,#17231,#17232,#17233,#17234,#17235,#17236,#17237,#17238,
#17239,#17240,#17241,#17242,#17243,#17244,#17245),.UNSPECIFIED.,.F.,.F.,
(4,3,3,3,3,3,3,3,3,3,3,4),(0.,9.7572728723403E-5,0.000197558568027757,0.000263369830764721,
0.000264501976385979,0.000410751214966632,0.000527720220099549,0.000529003952771959,
0.000711275183702182,0.000792685220207923,0.000986383339293457,0.00105800790554391),
 .UNSPECIFIED.);
#434=B_SPLINE_CURVE_WITH_KNOTS('',3,(#17253,#17254,#17255,#17256,#17257,
#17258,#17259,#17260,#17261,#17262,#17263,#17264,#17265,#17266,#17267,#17268,
#17269,#17270,#17271,#17272,#17273,#17274,#17275,#17276,#17277,#17278,#17279,
#17280,#17281,#17282,#17283,#17284,#17285,#17286,#17287,#17288,#17289,#17290,
#17291,#17292,#17293,#17294,#17295),.UNSPECIFIED.,.F.,.F.,(4,3,3,3,3,3,
3,3,3,3,3,3,3,3,4),(0.,0.000122774773565863,0.000252172289565749,0.000391124229768784,
0.000417443869709969,0.000418563871648259,0.000739329889542507,0.000834887739419938,
0.000836592389993165,0.00109817436553555,0.00125233160912991,0.00125385075554295,
0.00142036066599669,0.00155691800753188,0.00166977547883988),
 .UNSPECIFIED.);
#435=B_SPLINE_CURVE_WITH_KNOTS('',3,(#17305,#17306,#17307,#17308,#17309,
#17310,#17311,#17312,#17313,#17314,#17315,#17316,#17317,#17318,#17319,#17320,
#17321,#17322,#17323,#17324,#17325,#17326,#17327,#17328,#17329,#17330,#17331,
#17332,#17333,#17334,#17335,#17336,#17337,#17338,#17339,#17340,#17341,#17342,
#17343,#17344,#17345,#17346,#17347,#17348,#17349,#17350),.UNSPECIFIED.,
 .F.,.F.,(4,3,3,3,3,3,3,3,3,3,3,3,3,3,3,4),(0.,6.08280066317263E-5,0.000143504025126593,
0.000222132236418946,0.000243312026526905,0.000273726029842769,0.000390756960322061,
0.000486624053053811,0.000487092885051591,0.000652104140237346,0.000729936079580716,
0.000730491914653081,0.000807330947238143,0.000884197975617686,0.000957724799086867,
0.000973248106107622),.UNSPECIFIED.);
#436=B_SPLINE_CURVE_WITH_KNOTS('',3,(#17358,#17359,#17360,#17361,#17362,
#17363,#17364,#17365,#17366,#17367,#17368,#17369,#17370,#17371,#17372,#17373,
#17374,#17375,#17376,#17377,#17378,#17379,#17380,#17381,#17382,#17383,#17384,
#17385,#17386,#17387,#17388),.UNSPECIFIED.,.F.,.F.,(4,3,3,3,3,3,3,3,3,3,
4),(0.,0.000110044300710652,0.00022753767939358,0.000345953766326745,0.000459500393988843,
0.000506968361890628,0.000507607986070015,0.000621724537891887,0.000763599672912397,
0.000889140904505298,0.00101393672378126),.UNSPECIFIED.);
#437=B_SPLINE_CURVE_WITH_KNOTS('',3,(#17391,#17392,#17393,#17394,#17395,
#17396,#17397,#17398,#17399,#17400,#17401,#17402,#17403,#17404,#17405,#17406,
#17407,#17408,#17409,#17410,#17411,#17412,#17413,#17414,#17415,#17416,#17417,
#17418,#17419,#17420,#17421,#17422,#17423,#17424),.UNSPECIFIED.,.F.,.F.,
(4,3,3,3,3,3,3,3,3,3,3,4),(0.,9.75727287165792E-5,0.000197558568020339,
0.000263369830764727,0.000264501976385978,0.000410751214991148,0.000527720220099542,
0.000529003952771956,0.000711275183778258,0.000792685220207718,0.000986383339389978,
0.0010580079055439),.UNSPECIFIED.);
#438=B_SPLINE_CURVE_WITH_KNOTS('',3,(#17430,#17431,#17432,#17433,#17434,
#17435,#17436,#17437,#17438,#17439,#17440,#17441,#17442,#17443,#17444,#17445,
#17446,#17447,#17448,#17449,#17450,#17451,#17452,#17453,#17454,#17455,#17456,
#17457,#17458,#17459,#17460,#17461,#17462,#17463,#17464,#17465,#17466,#17467,
#17468,#17469,#17470,#17471,#17472),.UNSPECIFIED.,.F.,.F.,(4,3,3,3,3,3,
3,3,3,3,3,3,3,3,4),(0.,0.000122774773560884,0.000252172289555377,0.000391124229755383,
0.000417443869709971,0.000418563871648265,0.000739329890771365,0.000834887739419941,
0.000836592389993166,0.00109817436572929,0.00125233160912991,0.00125385075554294,
0.00142036066608084,0.00155691800768044,0.00166977547883988),
 .UNSPECIFIED.);
#439=B_SPLINE_CURVE_WITH_KNOTS('',3,(#17481,#17482,#17483,#17484,#17485,
#17486,#17487,#17488,#17489,#17490,#17491,#17492,#17493,#17494,#17495,#17496,
#17497,#17498,#17499,#17500,#17501,#17502,#17503,#17504,#17505,#17506,#17507,
#17508,#17509,#17510,#17511,#17512,#17513,#17514,#17515,#17516,#17517,#17518,
#17519,#17520,#17521,#17522,#17523,#17524,#17525,#17526),.UNSPECIFIED.,
 .F.,.F.,(4,3,3,3,3,3,3,3,3,3,3,3,3,3,3,4),(0.,6.08280066317253E-5,0.000143504025133277,
0.000222132236430928,0.000243312026526901,0.000273726029842764,0.000390756960290358,
0.000486624053053802,0.000487092885051583,0.000652104140099763,0.000729936079580704,
0.000730491914653072,0.000807330947240576,0.000884197975626852,0.000957724799105996,
0.000973248106107605),.UNSPECIFIED.);
#440=B_SPLINE_CURVE_WITH_KNOTS('',3,(#17532,#17533,#17534,#17535,#17536,
#17537,#17538,#17539,#17540,#17541,#17542,#17543,#17544,#17545,#17546,#17547,
#17548,#17549,#17550,#17551,#17552,#17553,#17554,#17555,#17556,#17557,#17558,
#17559,#17560,#17561,#17562),.UNSPECIFIED.,.F.,.F.,(4,3,3,3,3,3,3,3,3,3,
4),(0.,0.000110044300698132,0.000227537679367395,0.000345953766286372,0.000459500393934088,
0.000506968361890626,0.000507607986070008,0.0006217245378919,0.000763599672881826,
0.000889140904448288,0.00101393672378125),.UNSPECIFIED.);
#441=B_SPLINE_CURVE_WITH_KNOTS('',3,(#17566,#17567,#17568,#17569,#17570,
#17571,#17572,#17573,#17574,#17575,#17576,#17577,#17578,#17579,#17580,#17581,
#17582,#17583,#17584,#17585,#17586,#17587,#17588,#17589,#17590,#17591,#17592,
#17593,#17594,#17595,#17596,#17597,#17598,#17599),.UNSPECIFIED.,.F.,.F.,
(4,3,3,3,3,3,3,3,3,3,3,4),(0.,9.75727287258748E-5,0.000197558568032606,
0.000263369830764718,0.000264501976385979,0.000410751215061321,0.000527720220099554,
0.000529003952771959,0.000711275183839031,0.000792685220207918,0.000986383339454815,
0.00105800790554391),.UNSPECIFIED.);
#442=B_SPLINE_CURVE_WITH_KNOTS('',3,(#17607,#17608,#17609,#17610,#17611,
#17612,#17613,#17614,#17615,#17616,#17617,#17618,#17619,#17620,#17621,#17622,
#17623,#17624,#17625,#17626,#17627,#17628,#17629,#17630,#17631,#17632,#17633,
#17634,#17635,#17636,#17637,#17638,#17639,#17640,#17641,#17642,#17643,#17644,
#17645,#17646,#17647,#17648,#17649),.UNSPECIFIED.,.F.,.F.,(4,3,3,3,3,3,
3,3,3,3,3,3,3,3,4),(0.,0.000122774773571519,0.000252172289575277,0.000391124229778881,
0.000417443869709969,0.000418563871648264,0.000739329890508021,0.000834887739419938,
0.000836592389993168,0.0010981743657467,0.00125233160912991,0.00125385075554294,
0.00142036066604611,0.00155691800761702,0.00166977547883988),
 .UNSPECIFIED.);
#443=B_SPLINE_CURVE_WITH_KNOTS('',3,(#17673,#17674,#17675,#17676,#17677,
#17678,#17679,#17680),.UNSPECIFIED.,.F.,.F.,(4,2,2,4),(0.,0.00062500000000072,
0.00312500000008065,0.00654794813346023),.UNSPECIFIED.);
#444=B_SPLINE_CURVE_WITH_KNOTS('',3,(#17684,#17685,#17686,#17687,#17688,
#17689,#17690,#17691,#17692,#17693),.UNSPECIFIED.,.F.,.F.,(4,2,2,2,4),(0.,
0.0110943326857293,0.016641499028594,0.0194150822000263,0.0221886653714587),
 .UNSPECIFIED.);
#445=B_SPLINE_CURVE_WITH_KNOTS('',3,(#17695,#17696,#17697,#17698,#17699,
#17700,#17701,#17702,#17703,#17704),.UNSPECIFIED.,.F.,.F.,(4,2,2,2,4),(0.0221886653714587,
0.0332305757457702,0.0359910533393481,0.038751530932926,0.0442724861200819),
 .UNSPECIFIED.);
#446=B_SPLINE_CURVE_WITH_KNOTS('',3,(#17707,#17708,#17709,#17710,#17711,
#17712,#17713,#17714),.UNSPECIFIED.,.F.,.F.,(4,2,2,4),(1.30968750346023E-17,
0.000625000000000436,0.00312500000006035,0.0065479481334553),
 .UNSPECIFIED.);
#447=B_SPLINE_CURVE_WITH_KNOTS('',3,(#17807,#17808,#17809,#17810,#17811,
#17812,#17813,#17814),.UNSPECIFIED.,.F.,.F.,(4,2,2,4),(0.,0.000324140863782348,
0.000648281727564695,0.00129656345512939),.UNSPECIFIED.);
#448=B_SPLINE_CURVE_WITH_KNOTS('',3,(#17818,#17819,#17820,#17821,#17822,
#17823,#17824,#17825),.UNSPECIFIED.,.F.,.F.,(4,2,2,4),(0.,0.000642153724747558,
0.000963230587121339,0.00128430744949512),.UNSPECIFIED.);
#449=B_SPLINE_CURVE_WITH_KNOTS('',3,(#17829,#17830,#17831,#17832,#17833,
#17834,#17835,#17836,#17837,#17838,#17839,#17840,#17841,#17842,#17843,#17844,
#17845,#17846,#17847),.UNSPECIFIED.,.F.,.F.,(4,3,3,3,3,3,4),(0.,0.000195874855531394,
0.000407633432445313,0.000642628402010786,0.000643366204945988,0.00124146542702823,
0.00128673240989198),.UNSPECIFIED.);
#450=B_SPLINE_CURVE_WITH_KNOTS('',3,(#17851,#17852,#17853,#17854,#17855,
#17856,#17857,#17858,#17859,#17860,#17861,#17862,#17863,#17864,#17865,#17866,
#17867,#17868,#17869),.UNSPECIFIED.,.F.,.F.,(4,3,3,3,3,3,4),(0.,0.000446723853990593,
0.000644054549895828,0.000644233932867389,0.000966350899301084,0.00120471562689313,
0.00128846786573478),.UNSPECIFIED.);
#451=B_SPLINE_CURVE_WITH_KNOTS('',3,(#17873,#17874,#17875,#17876,#17877,
#17878,#17879,#17880,#17881,#17882,#17883,#17884,#17885,#17886,#17887,#17888,
#17889,#17890,#17891),.UNSPECIFIED.,.F.,.F.,(4,3,3,3,3,3,4),(0.,0.000198161496041495,
0.000412566761351645,0.000642956139405752,0.000643725422538401,0.00123968599593009,
0.0012874508450768),.UNSPECIFIED.);
#452=B_SPLINE_CURVE_WITH_KNOTS('',3,(#17895,#17896,#17897,#17898,#17899,
#17900,#17901,#17902),.UNSPECIFIED.,.F.,.F.,(4,2,2,4),(0.,0.000642153724747562,
0.000963230587121341,0.00128430744949512),.UNSPECIFIED.);
#453=B_SPLINE_CURVE_WITH_KNOTS('',3,(#17906,#17907,#17908,#17909,#17910,
#17911,#17912,#17913,#17914,#17915,#17916,#17917,#17918,#17919,#17920,#17921,
#17922,#17923,#17924),.UNSPECIFIED.,.F.,.F.,(4,3,3,3,3,3,4),(0.,0.000195874855548819,
0.000407633432483008,0.000642628402010788,0.000643366204945996,0.00124146543005707,
0.00128673240989199),.UNSPECIFIED.);
#454=B_SPLINE_CURVE_WITH_KNOTS('',3,(#17928,#17929,#17930,#17931,#17932,
#17933,#17934,#17935,#17936,#17937,#17938,#17939,#17940,#17941,#17942,#17943,
#17944,#17945,#17946),.UNSPECIFIED.,.F.,.F.,(4,3,3,3,3,3,4),(0.,0.000501649919473043,
0.000643648102817533,0.000643900482232717,0.000965850723349075,0.00120614192088348,
0.00128780096446543),.UNSPECIFIED.);
#455=B_SPLINE_CURVE_WITH_KNOTS('',3,(#18100,#18101,#18102,#18103,#18104,
#18105,#18106,#18107,#18108,#18109,#18110,#18111,#18112,#18113,#18114,#18115,
#18116,#18117,#18118,#18119,#18120,#18121,#18122,#18123,#18124,#18125,#18126,
#18127,#18128,#18129,#18130),.UNSPECIFIED.,.F.,.F.,(4,3,3,3,3,3,3,3,3,3,
4),(0.00423087891556426,0.013713375686686,0.0177375823121115,0.0182590193856104,
0.020118220117775,0.0211142581612483,0.0218072955502234,0.0244909340103851,
0.0253408764930824,0.0282925811008705,0.0312442857086587),.UNSPECIFIED.);
#456=B_SPLINE_CURVE_WITH_KNOTS('',3,(#18133,#18134,#18135,#18136,#18137,
#18138,#18139,#18140,#18141,#18142,#18143,#18144,#18145,#18146,#18147,#18148,
#18149,#18150,#18151,#18152,#18153,#18154,#18155,#18156,#18157,#18158,#18159,
#18160,#18161,#18162,#18163,#18164,#18165,#18166,#18167,#18168,#18169),
 .UNSPECIFIED.,.F.,.F.,(4,3,3,3,3,3,3,3,3,3,3,3,4),(0.,0.00293383627619356,
0.00586767255238711,0.00671399432426571,0.00908462661832189,0.00938017817101472,
0.0100709914863986,0.0117876962259593,0.0129061418604891,0.0134279886485314,
0.0185395617742769,0.0234677093302294,0.0268559772970629),.UNSPECIFIED.);
#457=B_SPLINE_CURVE_WITH_KNOTS('',3,(#18177,#18178,#18179,#18180,#18181,
#18182,#18183,#18184,#18185,#18186,#18187,#18188,#18189,#18190,#18191,#18192,
#18193,#18194,#18195,#18196,#18197,#18198,#18199,#18200,#18201,#18202,#18203,
#18204,#18205,#18206,#18207),.UNSPECIFIED.,.F.,.F.,(4,3,3,3,3,3,3,3,3,3,
4),(0.00423087891556413,0.0137133751566899,0.0177375823121114,0.0182590193856102,
0.0201182201175346,0.0211142581612482,0.0218072955502231,0.024490934010385,
0.0253408764930823,0.0282925811008705,0.0312442857086587),.UNSPECIFIED.);
#458=B_SPLINE_CURVE_WITH_KNOTS('',3,(#18210,#18211,#18212,#18213,#18214,
#18215,#18216,#18217,#18218,#18219,#18220,#18221,#18222,#18223,#18224,#18225,
#18226,#18227,#18228,#18229,#18230,#18231,#18232,#18233,#18234,#18235,#18236,
#18237,#18238,#18239,#18240,#18241,#18242,#18243,#18244,#18245,#18246),
 .UNSPECIFIED.,.F.,.F.,(4,3,3,3,3,3,3,3,3,3,3,3,4),(0.,0.00293383627619322,
0.00586767255238644,0.00671399432426573,0.00908462661700898,0.00938017817101484,
0.0100709914863986,0.0117876962256719,0.0129061418604892,0.0134279886485315,
0.018539561770304,0.02346770932428,0.0268559772970629),.UNSPECIFIED.);
#459=B_SPLINE_CURVE_WITH_KNOTS('',3,(#18254,#18255,#18256,#18257,#18258,
#18259,#18260,#18261,#18262,#18263,#18264,#18265,#18266,#18267,#18268,#18269,
#18270,#18271,#18272,#18273,#18274,#18275,#18276,#18277,#18278,#18279,#18280,
#18281,#18282,#18283,#18284,#18285,#18286,#18287),.UNSPECIFIED.,.F.,.F.,
(4,3,3,3,3,3,3,3,3,3,3,4),(0.0041940778674379,0.00785137044488797,0.00864322402522931,
0.00888216076442238,0.0105632172613147,0.0122879239676185,0.0130923701830207,
0.0136962196480358,0.0161859644978567,0.0187205500997639,0.0213309666493633,
0.0219906624986036),.UNSPECIFIED.);
#460=B_SPLINE_CURVE_WITH_KNOTS('',3,(#18290,#18291,#18292,#18293,#18294,
#18295,#18296,#18297,#18298,#18299,#18300,#18301,#18302,#18303,#18304,#18305,
#18306,#18307,#18308,#18309,#18310,#18311,#18312,#18313,#18314,#18315,#18316,
#18317,#18318,#18319,#18320,#18321,#18322,#18323),.UNSPECIFIED.,.F.,.F.,
(4,3,3,3,3,3,3,3,3,3,3,4),(0.,0.00259497273974606,0.00513490948945618,0.00760920564936369,
0.0083165426104236,0.00892204401521707,0.0106541774038738,0.012350736986894,
0.0131434725515692,0.0133830660228256,0.0170412668483451,0.0178440880304342),
 .UNSPECIFIED.);
#461=B_SPLINE_CURVE_WITH_KNOTS('',3,(#18331,#18332,#18333,#18334,#18335,
#18336,#18337,#18338,#18339,#18340,#18341,#18342,#18343,#18344,#18345,#18346,
#18347,#18348,#18349,#18350,#18351,#18352,#18353,#18354,#18355,#18356,#18357,
#18358,#18359,#18360,#18361),.UNSPECIFIED.,.F.,.F.,(4,3,3,3,3,3,3,3,3,3,
4),(0.00423087891556429,0.0137133753564976,0.0177375823121115,0.0182590193856104,
0.0201182201184656,0.0211142581612483,0.0218072955502225,0.0244909340103851,
0.0253408764930806,0.0282925811008696,0.0312442857086587),.UNSPECIFIED.);
#462=B_SPLINE_CURVE_WITH_KNOTS('',3,(#18364,#18365,#18366,#18367,#18368,
#18369,#18370,#18371,#18372,#18373,#18374,#18375,#18376,#18377,#18378,#18379,
#18380,#18381,#18382,#18383,#18384,#18385,#18386,#18387,#18388,#18389,#18390,
#18391,#18392,#18393,#18394,#18395,#18396,#18397,#18398,#18399,#18400),
 .UNSPECIFIED.,.F.,.F.,(4,3,3,3,3,3,3,3,3,3,3,3,4),(0.,0.00293383627619317,
0.00586767255238635,0.00671399432426571,0.0090846266183258,0.00938017817101421,
0.0100709914863986,0.0117876962251359,0.012906141860489,0.0134279886485314,
0.0185395617767228,0.0234677093338155,0.0268559772970629),.UNSPECIFIED.);
#463=B_SPLINE_CURVE_WITH_KNOTS('',3,(#18406,#18407,#18408,#18409,#18410,
#18411,#18412,#18413,#18414,#18415,#18416,#18417,#18418,#18419,#18420,#18421,
#18422,#18423,#18424,#18425,#18426,#18427,#18428,#18429,#18430,#18431,#18432,
#18433,#18434,#18435,#18436,#18437,#18438,#18439,#18440,#18441,#18442,#18443,
#18444,#18445,#18446,#18447,#18448,#18449,#18450,#18451,#18452,#18453,#18454),
 .UNSPECIFIED.,.F.,.F.,(4,3,3,3,3,3,3,3,3,3,3,3,3,3,3,3,4),(0.,0.000121245606235739,
0.000242857142540301,0.000287360877759073,0.000288270017838695,0.00044340391293331,
0.000574721755518147,0.000575971165655795,0.000665917057789352,0.000718402194397684,
0.000790242413837452,0.000826162523557336,0.00086208263327722,0.000975072145641068,
0.00100576307215676,0.00111728780497372,0.00114944351103629),
 .UNSPECIFIED.);
#464=B_SPLINE_CURVE_WITH_KNOTS('',3,(#18460,#18461,#18462,#18463,#18464,
#18465,#18466,#18467),.UNSPECIFIED.,.F.,.F.,(4,2,2,4),(0.,0.0138082473482012,
0.0207123710223017,0.0276164946964023),.UNSPECIFIED.);
#465=B_SPLINE_CURVE_WITH_KNOTS('',3,(#18525,#18526,#18527,#18528,#18529,
#18530,#18531,#18532,#18533,#18534,#18535,#18536,#18537,#18538,#18539,#18540,
#18541,#18542,#18543,#18544,#18545,#18546,#18547,#18548,#18549,#18550,#18551,
#18552,#18553,#18554,#18555,#18556,#18557,#18558),.UNSPECIFIED.,.F.,.F.,
(4,3,3,3,3,3,3,3,3,3,3,4),(0.,0.000110567770978162,0.000229163742149365,
0.000349602945021368,0.000466129197479698,0.000503962612308792,0.000504370554078785,
0.000654658246769462,0.00073377218761534,0.000861351750975835,0.000986409541182947,
0.00100874110815757),.UNSPECIFIED.);
#466=B_SPLINE_CURVE_WITH_KNOTS('',3,(#18578,#18579,#18580,#18581,#18582,
#18583,#18584,#18585,#18586,#18587,#18588,#18589,#18590,#18591,#18592,#18593,
#18594,#18595,#18596,#18597,#18598,#18599,#18600,#18601,#18602,#18603,#18604,
#18605),.UNSPECIFIED.,.F.,.F.,(4,3,3,3,3,3,3,3,3,4),(0.,9.61627041774626E-5,
0.00019464312403552,0.000263598431963766,0.00026390914929366,0.000510523427512722,
0.000527611135930377,0.00052781829858732,0.000791654292983114,0.00105563659717466),
 .UNSPECIFIED.);
#467=B_SPLINE_CURVE_WITH_KNOTS('',3,(#18611,#18612,#18613,#18614,#18615,
#18616,#18617,#18618,#18619,#18620,#18621,#18622,#18623,#18624,#18625,#18626),
 .UNSPECIFIED.,.F.,.F.,(4,3,3,3,3,4),(4.52743470429961E-15,0.00201520691454984,
0.00402253547201281,0.00602595242279557,0.00802370171969772,0.00993491157965328),
 .UNSPECIFIED.);
#468=B_SPLINE_CURVE_WITH_KNOTS('',3,(#18628,#18629,#18630,#18631,#18632,
#18633,#18634,#18635,#18636,#18637,#18638,#18639,#18640,#18641,#18642,#18643,
#18644,#18645,#18646,#18647,#18648,#18649,#18650,#18651,#18652,#18653,#18654,
#18655,#18656,#18657,#18658,#18659,#18660,#18661,#18662,#18663,#18664,#18665,
#18666,#18667,#18668,#18669,#18670),.UNSPECIFIED.,.F.,.F.,(4,3,3,3,3,3,
3,3,3,3,3,3,3,3,4),(0.,0.000142261508725732,0.000306612281624613,0.000354680426257006,
0.000354839578464806,0.000671890824680844,0.000709360852514012,0.000709794319645988,
0.000798030959078264,0.000931036118924641,0.00106404127877102,0.00117707199637736,
0.00124138149189952,0.00135612593307565,0.00141872170502802),
 .UNSPECIFIED.);
#469=B_SPLINE_CURVE_WITH_KNOTS('',3,(#18677,#18678,#18679,#18680,#18681,
#18682,#18683,#18684,#18685,#18686,#18687,#18688,#18689,#18690,#18691,#18692,
#18693,#18694,#18695,#18696,#18697,#18698,#18699,#18700,#18701,#18702,#18703,
#18704,#18705,#18706,#18707,#18708,#18709,#18710,#18711,#18712,#18713,#18714,
#18715,#18716,#18717,#18718,#18719,#18720,#18721,#18722,#18723,#18724,#18725,
#18726,#18727,#18728,#18729,#18730,#18731),.UNSPECIFIED.,.F.,.F.,(4,3,3,
3,3,3,3,3,3,3,3,3,3,3,3,3,3,3,4),(0.,0.00292798214671484,0.00577262065274856,
0.0068275614526255,0.00693335737727641,0.00947217443703029,0.0103475581420102,
0.0104000360659146,0.0118697041217895,0.0132773954669506,0.0138667147545528,
0.0138781145226839,0.0166264516367541,0.017333393443191,0.0189487413424379,
0.0205003989925137,0.0210540430942383,0.0243937363013933,0.0277334295085482),
 .UNSPECIFIED.);
#470=B_SPLINE_CURVE_WITH_KNOTS('',3,(#18735,#18736,#18737,#18738,#18739,
#18740,#18741,#18742),.UNSPECIFIED.,.F.,.F.,(4,2,2,4),(1.11076499342709E-17,
0.000625000000000437,0.00312500000006035,0.00654794813345529),
 .UNSPECIFIED.);
#471=B_SPLINE_CURVE_WITH_KNOTS('',3,(#18746,#18747,#18748,#18749,#18750,
#18751,#18752,#18753),.UNSPECIFIED.,.F.,.F.,(4,2,2,4),(0.,0.000625000000000718,
0.00312500000008064,0.00654794813346023),.UNSPECIFIED.);
#472=B_SPLINE_CURVE_WITH_KNOTS('',3,(#18757,#18758,#18759,#18760,#18761,
#18762,#18763,#18764,#18765,#18766,#18767,#18768,#18769,#18770,#18771,#18772,
#18773,#18774,#18775,#18776),.UNSPECIFIED.,.F.,.F.,(4,2,2,2,2,2,2,2,2,4),
(0.,0.00559909194960567,0.0111981838992113,0.016797275848817,0.0195968218236199,
0.0223963677984227,0.033594551697634,0.0363940976724369,0.0391936436472397,
0.0447927355968454),.UNSPECIFIED.);
#473=B_SPLINE_CURVE_WITH_KNOTS('',3,(#18801,#18802,#18803,#18804,#18805,
#18806,#18807,#18808,#18809,#18810,#18811,#18812,#18813,#18814,#18815,#18816,
#18817,#18818,#18819,#18820,#18821,#18822,#18823,#18824,#18825,#18826,#18827,
#18828),.UNSPECIFIED.,.F.,.F.,(4,3,3,3,3,3,3,3,3,4),(0.,0.00303616132428222,
0.00606003537843287,0.00872529453770153,0.00872704110520405,0.0106174542445287,
0.012537763933558,0.0144774647805997,0.0164504962233993,0.0174540822104081),
 .UNSPECIFIED.);
#474=B_SPLINE_CURVE_WITH_KNOTS('',3,(#18841,#18842,#18843,#18844,#18845,
#18846,#18847,#18848,#18849,#18850,#18851,#18852,#18853,#18854,#18855,#18856,
#18857,#18858,#18859,#18860,#18861,#18862,#18863,#18864,#18865,#18866,#18867,
#18868,#18869,#18870,#18871,#18872,#18873,#18874,#18875,#18876,#18877,#18878,
#18879,#18880),.UNSPECIFIED.,.F.,.F.,(4,3,3,3,3,3,3,3,3,3,3,3,3,4),(0.,
0.0026172239816427,0.00435913346757955,0.00436870952384852,0.00564078314582411,
0.00692512632488316,0.00818670413876967,0.00873741904769704,0.00874916468941873,
0.0122136783028643,0.0131061285715456,0.0147515701824665,0.016420240909831,
0.0174748380953941),.UNSPECIFIED.);
#475=B_SPLINE_CURVE_WITH_KNOTS('',3,(#18916,#18917,#18918,#18919,#18920,
#18921,#18922,#18923,#18924,#18925,#18926,#18927,#18928,#18929,#18930,#18931,
#18932,#18933,#18934),.UNSPECIFIED.,.F.,.F.,(4,3,3,3,3,3,4),(0.,0.000209520759761111,
0.000422285836657762,0.000553215152468023,0.00055421709622049,0.000897330597716815,
0.00110843419244098),.UNSPECIFIED.);
#476=B_SPLINE_CURVE_WITH_KNOTS('',3,(#18946,#18947,#18948,#18949,#18950,
#18951,#18952,#18953,#18954,#18955,#18956,#18957,#18958),.UNSPECIFIED.,
 .F.,.F.,(4,3,3,3,4),(0.,0.000355508868027555,0.000556947538855294,0.000557267210332349,
0.0011145344206647),.UNSPECIFIED.);
#477=B_SPLINE_CURVE_WITH_KNOTS('',3,(#18959,#18960,#18961,#18962,#18963,
#18964,#18965,#18966,#18967,#18968,#18969,#18970,#18971,#18972,#18973,#18974,
#18975,#18976,#18977,#18978,#18979,#18980,#18981,#18982,#18983,#18984,#18985,
#18986,#18987,#18988,#18989,#18990,#18991,#18992,#18993,#18994,#18995,#18996,
#18997,#18998,#18999,#19000,#19001,#19002,#19003,#19004,#19005,#19006,#19007,
#19008,#19009,#19010,#19011,#19012,#19013,#19014,#19015,#19016,#19017,#19018,
#19019,#19020,#19021,#19022,#19023,#19024,#19025),.UNSPECIFIED.,.F.,.F.,
(4,3,3,3,3,3,3,3,3,3,3,3,3,3,3,3,3,3,3,3,3,3,4),(0.,0.00277040425654158,
0.00554080851308316,0.00557505688803485,0.00791560355491117,0.0083263576942907,
0.00836258533205228,0.0100018252555059,0.011122873465018,0.0111501137760697,
0.0223002275521394,0.0223209744612517,0.0250877559961568,0.025120499376563,
0.0278752844401742,0.0279173397075124,0.0311894101771566,0.0334503413282091,
0.0334957141052527,0.0369394202827424,0.0404389072898065,0.0440271687430516,
0.0446004551042788),.UNSPECIFIED.);
#478=B_SPLINE_CURVE_WITH_KNOTS('',3,(#19033,#19034,#19035,#19036,#19037,
#19038,#19039,#19040,#19041,#19042,#19043,#19044,#19045),.UNSPECIFIED.,
 .F.,.F.,(4,3,3,3,4),(0.,0.000355508867930007,0.000556947538855285,0.000557267210332339,
0.00111453442066468),.UNSPECIFIED.);
#479=B_SPLINE_CURVE_WITH_KNOTS('',3,(#19047,#19048,#19049,#19050,#19051,
#19052,#19053,#19054,#19055,#19056,#19057,#19058,#19059,#19060,#19061,#19062,
#19063,#19064,#19065,#19066,#19067,#19068,#19069,#19070,#19071,#19072,#19073,
#19074,#19075,#19076,#19077,#19078,#19079,#19080,#19081,#19082,#19083,#19084,
#19085,#19086,#19087,#19088,#19089,#19090,#19091,#19092,#19093,#19094,#19095,
#19096,#19097,#19098,#19099,#19100,#19101,#19102,#19103,#19104,#19105,#19106,
#19107,#19108,#19109,#19110,#19111,#19112,#19113,#19114,#19115,#19116,#19117,
#19118,#19119,#19120,#19121,#19122,#19123,#19124,#19125,#19126,#19127,#19128),
 .UNSPECIFIED.,.F.,.F.,(4,3,3,3,3,3,3,3,3,3,3,3,3,3,3,3,3,3,3,3,3,3,3,3,
3,3,3,4),(0.,0.00276800820692877,0.00539608564417642,0.00553601641385754,
0.00558313544569878,0.00832024774722178,0.00837470316854816,0.0100465608585699,
0.0111128364927737,0.0111662708913976,0.016725314895809,0.0220049729595792,
0.0222843589002204,0.0223325417827951,0.0244828693201949,0.0250773155042266,
0.0251241095056445,0.0278715865387033,0.0279156772284939,0.0323589146455993,
0.0334651286339482,0.0334988126741926,0.0357819208078993,0.0381532193852836,
0.0390680317130243,0.0415764658205088,0.0441988527874511,0.0446650835655902),
 .UNSPECIFIED.);
#480=B_SPLINE_CURVE_WITH_KNOTS('',3,(#19130,#19131,#19132,#19133,#19134,
#19135,#19136,#19137,#19138,#19139,#19140,#19141,#19142,#19143,#19144,#19145,
#19146,#19147,#19148),.UNSPECIFIED.,.F.,.F.,(4,3,3,3,3,3,4),(0.,0.000209520759735746,
0.000422285836606947,0.000553215152468011,0.000554217096220475,0.00089733059735611,
0.00110843419244095),.UNSPECIFIED.);
#481=B_SPLINE_CURVE_WITH_KNOTS('',3,(#19164,#19165,#19166,#19167,#19168,
#19169,#19170,#19171,#19172,#19173,#19174,#19175,#19176),.UNSPECIFIED.,
 .F.,.F.,(4,3,3,3,4),(0.,0.000732343305453042,0.00114589002873166,0.00114609016424996,
0.00229218032849993),.UNSPECIFIED.);
#482=B_SPLINE_CURVE_WITH_KNOTS('',3,(#19178,#19179,#19180,#19181,#19182,
#19183,#19184,#19185,#19186,#19187,#19188,#19189,#19190,#19191,#19192,#19193,
#19194,#19195,#19196,#19197,#19198,#19199,#19200,#19201,#19202,#19203,#19204,
#19205,#19206,#19207,#19208,#19209,#19210,#19211),.UNSPECIFIED.,.F.,.F.,
(4,3,3,3,3,3,3,3,3,3,3,4),(0.,0.00365414724118507,0.0072761561111727,0.0086843723171071,
0.00868483454405469,0.0100721107296485,0.0114668861298135,0.012827029272143,
0.0130265584756607,0.0130435595235905,0.0155867439515361,0.0173687446342142),
 .UNSPECIFIED.);
#483=B_SPLINE_CURVE_WITH_KNOTS('',3,(#19213,#19214,#19215,#19216,#19217,
#19218,#19219,#19220,#19221,#19222,#19223,#19224,#19225),.UNSPECIFIED.,
 .F.,.F.,(4,3,3,3,4),(0.,0.000722789662616506,0.00114552600039172,0.00114627200830295,
0.00229254401660589),.UNSPECIFIED.);
#484=B_SPLINE_CURVE_WITH_KNOTS('',3,(#19234,#19235,#19236,#19237,#19238,
#19239,#19240,#19241,#19242,#19243,#19244,#19245,#19246),.UNSPECIFIED.,
 .F.,.F.,(4,3,3,3,4),(0.,0.000722789662305103,0.00114552600039174,0.00114627200830296,
0.00229254401660593),.UNSPECIFIED.);
#485=B_SPLINE_CURVE_WITH_KNOTS('',3,(#19258,#19259,#19260,#19261,#19262,
#19263,#19264,#19265,#19266,#19267,#19268,#19269,#19270),.UNSPECIFIED.,
 .F.,.F.,(4,3,3,3,4),(0.,0.000732343305065348,0.00114589002873164,0.00114609016424995,
0.00229218032849991),.UNSPECIFIED.);
#486=B_SPLINE_CURVE_WITH_KNOTS('',3,(#19271,#19272,#19273,#19274,#19275,
#19276,#19277,#19278,#19279,#19280,#19281,#19282,#19283,#19284,#19285,#19286,
#19287,#19288,#19289),.UNSPECIFIED.,.F.,.F.,(4,3,3,3,3,3,4),(0.,0.00521863817648657,
0.00869843096504882,0.00870860595373375,0.0117141048141897,0.0147339377832446,
0.0173968619300976),.UNSPECIFIED.);
#487=B_SPLINE_CURVE_WITH_KNOTS('',3,(#19305,#19306,#19307,#19308,#19309,
#19310,#19311,#19312,#19313,#19314,#19315,#19316,#19317,#19318,#19319,#19320,
#19321,#19322,#19323,#19324,#19325,#19326,#19327,#19328,#19329,#19330,#19331,
#19332,#19333,#19334,#19335,#19336,#19337,#19338,#19339,#19340,#19341,#19342,
#19343,#19344,#19345,#19346,#19347,#19348,#19349,#19350,#19351,#19352,#19353,
#19354,#19355,#19356,#19357,#19358,#19359),.UNSPECIFIED.,.F.,.F.,(4,3,3,
3,3,3,3,3,3,3,3,3,3,3,3,3,3,3,4),(0.,1.698189733476E-5,8.14940608034467E-5,
0.00014434612734546,0.000176187184848135,0.000188127581411639,0.000198575428404704,
0.000271710357356161,0.000368390804286231,0.000407565536034241,0.000522428725604158,
0.000543393651925955,0.000543420714712321,0.000611348304051362,0.000713239688059922,
0.000815131072068482,0.000915281326817688,0.00101655523193233,0.00108684142942464),
 .UNSPECIFIED.);
#488=B_SPLINE_CURVE_WITH_KNOTS('',3,(#19363,#19364,#19365,#19366,#19367,
#19368,#19369,#19370,#19371,#19372,#19373,#19374,#19375,#19376,#19377,#19378,
#19379,#19380,#19381),.UNSPECIFIED.,.F.,.F.,(4,3,3,3,3,3,4),(0.,0.000386464906251142,
0.000552252634628128,0.000553922129943384,0.000781486939925102,0.000957814850417398,
0.00110784425988677),.UNSPECIFIED.);
#489=B_SPLINE_CURVE_WITH_KNOTS('',3,(#19385,#19386,#19387,#19388,#19389,
#19390,#19391,#19392),.UNSPECIFIED.,.F.,.F.,(4,2,2,4),(0.,0.000279899994294907,
0.000559799988589814,0.00111959997717964),.UNSPECIFIED.);
#490=B_SPLINE_CURVE_WITH_KNOTS('',3,(#19396,#19397,#19398,#19399,#19400,
#19401,#19402,#19403,#19404,#19405,#19406,#19407,#19408,#19409,#19410,#19411,
#19412,#19413,#19414,#19415,#19416,#19417,#19418,#19419,#19420,#19421,#19422,
#19423,#19424,#19425,#19426,#19427,#19428,#19429,#19430,#19431,#19432,#19433,
#19434,#19435,#19436,#19437,#19438,#19439,#19440,#19441,#19442,#19443,#19444,
#19445,#19446,#19447,#19448,#19449,#19450),.UNSPECIFIED.,.F.,.F.,(4,3,3,
3,3,3,3,3,3,3,3,3,3,3,3,3,3,3,4),(0.,6.41135074222687E-5,0.000127328256831397,
0.000175449478231306,0.000175455278330882,0.000350898956462612,0.000350910556668815,
0.000701797912925202,0.000701821113336483,0.000745660282483025,0.000850761974087649,
0.000899178575935408,0.0009759377226616,0.0010143172960247,0.00105269686938779,
0.00115231295106207,0.00122814634761909,0.00133756611931813,0.00140359582585038),
 .UNSPECIFIED.);
#491=B_SPLINE_CURVE_WITH_KNOTS('',3,(#19484,#19485,#19486,#19487,#19488,
#19489,#19490,#19491,#19492,#19493,#19494,#19495,#19496,#19497,#19498,#19499,
#19500,#19501,#19502,#19503,#19504,#19505,#19506,#19507,#19508,#19509,#19510,
#19511,#19512,#19513,#19514,#19515,#19516,#19517,#19518,#19519,#19520,#19521,
#19522,#19523,#19524,#19525,#19526,#19527,#19528,#19529,#19530,#19531,#19532,
#19533,#19534,#19535,#19536,#19537,#19538),.UNSPECIFIED.,.F.,.F.,(4,3,3,
3,3,3,3,3,3,3,3,3,3,3,3,3,3,3,4),(0.,6.41135074144232E-5,0.000127328256817319,
0.000175449478231299,0.000175455278330868,0.000350898956462599,0.000350910556668804,
0.000701797912925195,0.000701821113336461,0.00074566028248302,0.000850761974086255,
0.000899178575935406,0.000975937722661599,0.0010143172960247,0.00105269686938779,
0.00115231295106248,0.00122814634761909,0.00133756611931546,0.00140359582585039),
 .UNSPECIFIED.);
#492=B_SPLINE_CURVE_WITH_KNOTS('',3,(#19548,#19549,#19550,#19551,#19552,
#19553,#19554,#19555,#19556,#19557,#19558,#19559,#19560,#19561,#19562,#19563,
#19564,#19565,#19566,#19567,#19568,#19569,#19570,#19571,#19572,#19573,#19574,
#19575,#19576,#19577,#19578,#19579,#19580,#19581,#19582,#19583,#19584,#19585,
#19586,#19587,#19588,#19589,#19590,#19591,#19592,#19593,#19594,#19595,#19596,
#19597,#19598,#19599,#19600,#19601,#19602),.UNSPECIFIED.,.F.,.F.,(4,3,3,
3,3,3,3,3,3,3,3,3,3,3,3,3,3,3,4),(0.,1.69818973347599E-5,8.14940608033093E-5,
0.000144346127345459,0.000176187184848134,0.000188127581411637,0.000198575428404702,
0.000271710357356158,0.000368390804288842,0.000407565536034237,0.00052242872560825,
0.000543393651925955,0.000543420714712316,0.000611348304051356,0.000713239688059915,
0.000815131072068475,0.000915281326823676,0.00101655523194574,0.00108684142942463),
 .UNSPECIFIED.);
#493=B_SPLINE_CURVE_WITH_KNOTS('',3,(#19606,#19607,#19608,#19609,#19610,
#19611,#19612,#19613,#19614,#19615,#19616,#19617,#19618,#19619,#19620,#19621,
#19622,#19623,#19624,#19625,#19626,#19627),.UNSPECIFIED.,.F.,.F.,(4,3,3,
3,3,3,3,4),(0.,0.000386658565627056,0.000552413504322274,0.000554054021566752,
0.00077021335329488,0.000939160698214192,0.00109876969131035,0.0011081080431335),
 .UNSPECIFIED.);
#494=B_SPLINE_CURVE_WITH_KNOTS('',3,(#19630,#19631,#19632,#19633,#19634,
#19635,#19636,#19637),.UNSPECIFIED.,.F.,.F.,(4,2,2,4),(0.,0.000279899994294914,
0.000559799988589829,0.00111959997717965),.UNSPECIFIED.);
#495=B_SPLINE_CURVE_WITH_KNOTS('',3,(#19642,#19643,#19644,#19645,#19646,
#19647,#19648,#19649,#19650,#19651,#19652,#19653,#19654,#19655,#19656,#19657,
#19658,#19659,#19660,#19661,#19662,#19663,#19664,#19665,#19666,#19667,#19668,
#19669,#19670,#19671,#19672,#19673,#19674,#19675,#19676,#19677,#19678,#19679,
#19680,#19681,#19682,#19683,#19684,#19685,#19686,#19687,#19688,#19689,#19690,
#19691,#19692,#19693,#19694,#19695,#19696),.UNSPECIFIED.,.F.,.F.,(4,3,3,
3,3,3,3,3,3,3,3,3,3,3,3,3,3,3,4),(0.,6.41135074167853E-5,0.000127328256820419,
0.000175449478231291,0.000175455278330845,0.000350898956462582,0.000350910556668788,
0.000701797912925185,0.000701821113336456,0.00074566028248301,0.000850761974083129,
0.000899178575935398,0.000975937722661593,0.00101431729602469,0.00105269686938779,
0.0011523129510611,0.00122814634761909,0.00133756611931672,0.00140359582585039),
 .UNSPECIFIED.);
#496=B_SPLINE_CURVE_WITH_KNOTS('',3,(#19703,#19704,#19705,#19706,#19707,
#19708,#19709,#19710,#19711,#19712,#19713,#19714,#19715,#19716,#19717,#19718,
#19719,#19720,#19721,#19722,#19723,#19724,#19725,#19726,#19727,#19728,#19729,
#19730,#19731,#19732,#19733,#19734,#19735,#19736,#19737,#19738,#19739,#19740,
#19741,#19742,#19743,#19744,#19745,#19746,#19747,#19748,#19749,#19750,#19751,
#19752,#19753,#19754,#19755,#19756,#19757),.UNSPECIFIED.,.F.,.F.,(4,3,3,
3,3,3,3,3,3,3,3,3,3,3,3,3,3,3,4),(0.,1.69818973347599E-5,8.1494060804179E-5,
0.000144346127345459,0.000176187184848134,0.000188127581411637,0.000198575428404702,
0.000271710357356159,0.000368390804303863,0.000407565536034238,0.000522428725615084,
0.000543393651925945,0.000543420714712318,0.000611348304051357,0.000713239688059917,
0.000815131072068476,0.000915281326813642,0.00101655523192292,0.00108684142942464),
 .UNSPECIFIED.);
#497=B_SPLINE_CURVE_WITH_KNOTS('',3,(#19761,#19762,#19763,#19764,#19765,
#19766,#19767,#19768,#19769,#19770,#19771,#19772,#19773,#19774,#19775,#19776,
#19777,#19778,#19779,#19780,#19781,#19782),.UNSPECIFIED.,.F.,.F.,(4,3,3,
3,3,3,3,4),(0.,0.000387102023918642,0.00055263573178344,0.000554236032887,
0.000759142685557146,0.000933807375665573,0.00108627346338914,0.001108472065774),
 .UNSPECIFIED.);
#498=B_SPLINE_CURVE_WITH_KNOTS('',3,(#19785,#19786,#19787,#19788,#19789,
#19790,#19791,#19792),.UNSPECIFIED.,.F.,.F.,(4,2,2,4),(0.,0.000279899994294914,
0.000559799988589829,0.00111959997717965),.UNSPECIFIED.);
#499=B_SPLINE_CURVE_WITH_KNOTS('',3,(#19801,#19802,#19803,#19804,#19805,
#19806,#19807,#19808,#19809,#19810,#19811,#19812,#19813,#19814,#19815,#19816,
#19817,#19818,#19819,#19820,#19821,#19822,#19823,#19824,#19825,#19826,#19827,
#19828,#19829,#19830,#19831,#19832,#19833,#19834,#19835,#19836,#19837,#19838,
#19839,#19840,#19841,#19842,#19843,#19844,#19845,#19846,#19847,#19848,#19849,
#19850,#19851,#19852,#19853,#19854,#19855),.UNSPECIFIED.,.F.,.F.,(4,3,3,
3,3,3,3,3,3,3,3,3,3,3,3,3,3,3,4),(0.,1.69818973347602E-5,8.14940608001835E-5,
0.000144346127345461,0.000176187184848137,0.00018812758141164,0.000198575428404705,
0.000271710357356162,0.000368390804273793,0.000407565536034244,0.00052242872563187,
0.000543393651925935,0.000543420714712325,0.000611348304051366,0.000713239688059926,
0.000815131072068487,0.000915281326815586,0.00101655523192821,0.00108684142942465),
 .UNSPECIFIED.);
#500=B_SPLINE_CURVE_WITH_KNOTS('',3,(#19859,#19860,#19861,#19862,#19863,
#19864,#19865,#19866,#19867,#19868,#19869,#19870,#19871,#19872,#19873,#19874,
#19875,#19876,#19877,#19878,#19879,#19880),.UNSPECIFIED.,.F.,.F.,(4,3,3,
3,3,3,3,4),(0.,0.000387003724944105,0.00055259360350697,0.000554201545442304,
0.000760942537037389,0.000934672813960999,0.0010883087198129,0.00110840309088461),
 .UNSPECIFIED.);
#501=B_SPLINE_CURVE_WITH_KNOTS('',3,(#19884,#19885,#19886,#19887,#19888,
#19889,#19890,#19891),.UNSPECIFIED.,.F.,.F.,(4,2,2,4),(0.,0.000279899994294911,
0.000559799988589822,0.00111959997717963),.UNSPECIFIED.);
#502=B_SPLINE_CURVE_WITH_KNOTS('',3,(#19895,#19896,#19897,#19898,#19899,
#19900,#19901,#19902,#19903,#19904,#19905,#19906,#19907,#19908,#19909,#19910,
#19911,#19912,#19913,#19914,#19915,#19916,#19917,#19918,#19919,#19920,#19921,
#19922,#19923,#19924,#19925,#19926,#19927,#19928,#19929,#19930,#19931,#19932,
#19933,#19934,#19935,#19936,#19937,#19938,#19939,#19940,#19941,#19942,#19943,
#19944,#19945,#19946,#19947,#19948,#19949),.UNSPECIFIED.,.F.,.F.,(4,3,3,
3,3,3,3,3,3,3,3,3,3,3,3,3,3,3,4),(0.,6.41135074214198E-5,0.000127328256829034,
0.00017544947823129,0.000175455278330849,0.000350898956462581,0.000350910556668772,
0.000701797912925182,0.00070182111333644,0.000745660282483008,0.000850761974083878,
0.000899178575935396,0.00097593772266159,0.00101431729602469,0.00105269686938778,
0.00115231295106392,0.00122814634761908,0.0013375661193188,0.00140359582585039),
 .UNSPECIFIED.);
#503=B_SPLINE_CURVE_WITH_KNOTS('',3,(#19957,#19958,#19959,#19960,#19961,
#19962,#19963,#19964),.UNSPECIFIED.,.F.,.F.,(4,2,2,4),(0.,0.00951523528670846,
0.0142728529300627,0.0190304705734169),.UNSPECIFIED.);
#504=B_SPLINE_CURVE_WITH_KNOTS('',3,(#19968,#19969,#19970,#19971,#19972,
#19973,#19974,#19975),.UNSPECIFIED.,.F.,.F.,(4,2,2,4),(0.,0.00476132581272555,
0.00952265162545109,0.0190453032509022),.UNSPECIFIED.);
#505=B_SPLINE_CURVE_WITH_KNOTS('',3,(#19982,#19983,#19984,#19985,#19986,
#19987,#19988,#19989,#19990,#19991,#19992,#19993,#19994,#19995,#19996,#19997,
#19998,#19999,#20000,#20001,#20002,#20003,#20004,#20005,#20006,#20007,#20008,
#20009,#20010,#20011,#20012,#20013,#20014,#20015),.UNSPECIFIED.,.F.,.F.,
(4,3,3,3,3,3,3,3,3,3,3,4),(0.00419407786743781,0.00785137040128593,0.00864322402522921,
0.0088821607644223,0.0105632172612041,0.0122879239673615,0.0130923701830206,
0.0136962196480357,0.0161859644983365,0.018720550100699,0.0213309666507153,
0.0219906624986034),.UNSPECIFIED.);
#506=B_SPLINE_CURVE_WITH_KNOTS('',3,(#20019,#20020,#20021,#20022,#20023,
#20024,#20025,#20026,#20027,#20028,#20029,#20030,#20031,#20032,#20033,#20034,
#20035,#20036,#20037,#20038,#20039,#20040,#20041,#20042,#20043,#20044,#20045,
#20046,#20047,#20048,#20049,#20050,#20051,#20052),.UNSPECIFIED.,.F.,.F.,
(4,3,3,3,3,3,3,3,3,3,3,4),(0.,0.00259497273884202,0.00513490948758917,0.00760920564643932,
0.00831654261042366,0.00892204401521709,0.0106541774041306,0.0123507369871751,
0.0131434725515692,0.0133830660228256,0.0170412668384166,0.0178440880304342),
 .UNSPECIFIED.);
#507=B_SPLINE_CURVE_WITH_KNOTS('',3,(#20059,#20060,#20061,#20062,#20063,
#20064,#20065,#20066,#20067,#20068,#20069,#20070,#20071,#20072,#20073,#20074,
#20075,#20076,#20077,#20078,#20079,#20080,#20081,#20082,#20083,#20084,#20085,
#20086,#20087,#20088,#20089),.UNSPECIFIED.,.F.,.F.,(4,3,3,3,3,3,3,3,3,3,
4),(0.00423087891556468,0.0137133753542596,0.0177375823121119,0.0182590193856109,
0.0201182201176651,0.0211142581612487,0.0218072955502239,0.0244909340103855,
0.025340876493083,0.0282925811008711,0.0312442857086592),.UNSPECIFIED.);
#508=B_SPLINE_CURVE_WITH_KNOTS('',3,(#20093,#20094,#20095,#20096,#20097,
#20098,#20099,#20100,#20101,#20102,#20103,#20104,#20105,#20106,#20107,#20108,
#20109,#20110,#20111,#20112,#20113,#20114,#20115,#20116,#20117,#20118,#20119,
#20120,#20121,#20122,#20123,#20124,#20125,#20126,#20127,#20128,#20129),
 .UNSPECIFIED.,.F.,.F.,(4,3,3,3,3,3,3,3,3,3,3,3,4),(0.,0.00293383627619294,
0.00586767255238587,0.0067139943242657,0.00908462661547173,0.00938017817101409,
0.0100709914863986,0.0117876962255473,0.0129061418604892,0.0134279886485314,
0.0185395617459084,0.0234677092734861,0.0268559772970628),.UNSPECIFIED.);
#509=B_SPLINE_CURVE_WITH_KNOTS('',3,(#20133,#20134,#20135,#20136,#20137,
#20138),.UNSPECIFIED.,.F.,.F.,(4,2,4),(0.,0.00327855488628776,0.00654795604494931),
 .UNSPECIFIED.);
#510=B_SPLINE_CURVE_WITH_KNOTS('',3,(#20147,#20148,#20149,#20150,#20151,
#20152),.UNSPECIFIED.,.F.,.F.,(4,2,4),(0.,0.00326940115867362,0.00654795604497327),
 .UNSPECIFIED.);
#511=B_SPLINE_CURVE_WITH_KNOTS('',3,(#20181,#20182,#20183,#20184,#20185,
#20186,#20187),.UNSPECIFIED.,.F.,.F.,(4,3,4),(0.,0.00700450430818859,0.00878441731503683),
 .UNSPECIFIED.);
#512=B_SPLINE_CURVE_WITH_KNOTS('',3,(#20203,#20204,#20205,#20206),
 .UNSPECIFIED.,.F.,.F.,(4,4),(0.,0.00906386388585899),.UNSPECIFIED.);
#513=B_SPLINE_CURVE_WITH_KNOTS('',3,(#20254,#20255,#20256,#20257,#20258,
#20259,#20260,#20261,#20262,#20263,#20264,#20265,#20266,#20267,#20268,#20269,
#20270,#20271,#20272,#20273,#20274,#20275,#20276,#20277,#20278,#20279,#20280,
#20281,#20282,#20283,#20284,#20285,#20286,#20287,#20288,#20289,#20290,#20291,
#20292,#20293,#20294,#20295,#20296,#20297,#20298,#20299,#20300,#20301,#20302),
 .UNSPECIFIED.,.F.,.F.,(4,3,3,3,3,3,3,3,3,3,3,3,3,3,3,3,4),(0.,0.000121245606188157,
0.000242857142460205,0.000287360877759076,0.00028827001783867,0.000443403913026412,
0.000574721755518153,0.000575971165655785,0.000665917057794762,0.000718402194397691,
0.00079024241383746,0.000826162523557345,0.000862082633277229,0.000975072145658159,
0.00100576307215677,0.00111728780498847,0.00114944351103631),
 .UNSPECIFIED.);
#514=B_SPLINE_CURVE_WITH_KNOTS('',3,(#20308,#20309,#20310,#20311,#20312,
#20313,#20314,#20315),.UNSPECIFIED.,.F.,.F.,(4,2,2,4),(0.,0.0138082473482012,
0.0207123710223018,0.0276164946964023),.UNSPECIFIED.);
#515=B_SPLINE_CURVE_WITH_KNOTS('',3,(#20327,#20328,#20329,#20330,#20331,
#20332,#20333,#20334,#20335,#20336,#20337,#20338,#20339,#20340,#20341,#20342,
#20343,#20344,#20345,#20346,#20347,#20348,#20349,#20350,#20351,#20352,#20353,
#20354,#20355,#20356,#20357,#20358,#20359,#20360),.UNSPECIFIED.,.F.,.F.,
(4,3,3,3,3,3,3,3,3,3,3,4),(0.,0.000110567770976802,0.000229163742145944,
0.000349602945016014,0.000466129197473093,0.0005039626123088,0.000504370554078788,
0.000654658246680043,0.000733772187615292,0.000861351751012203,0.000986409541283704,
0.00100874110815758),.UNSPECIFIED.);
#516=B_SPLINE_CURVE_WITH_KNOTS('',3,(#20377,#20378,#20379,#20380,#20381,
#20382,#20383,#20384,#20385,#20386,#20387,#20388,#20389,#20390,#20391,#20392,
#20393,#20394,#20395,#20396,#20397,#20398,#20399,#20400,#20401,#20402,#20403,
#20404),.UNSPECIFIED.,.F.,.F.,(4,3,3,3,3,3,3,3,3,4),(0.,9.61627041892685E-5,
0.000194643124037823,0.000263598431963766,0.000263909149293665,0.000510523428020468,
0.000527611135930389,0.00052781829858733,0.000791654292983009,0.00105563659717465),
 .UNSPECIFIED.);
#517=B_SPLINE_CURVE_WITH_KNOTS('',3,(#20410,#20411,#20412,#20413,#20414,
#20415,#20416,#20417,#20418,#20419,#20420,#20421,#20422,#20423,#20424,#20425),
 .UNSPECIFIED.,.F.,.F.,(4,3,3,3,3,4),(4.53161437099327E-15,0.00201520691464592,
0.00402253547213016,0.00602595242291411,0.00802370171983992,0.00993491157965329),
 .UNSPECIFIED.);
#518=B_SPLINE_CURVE_WITH_KNOTS('',3,(#20427,#20428,#20429,#20430,#20431,
#20432,#20433,#20434,#20435,#20436,#20437,#20438,#20439,#20440,#20441,#20442,
#20443,#20444,#20445,#20446,#20447,#20448,#20449,#20450,#20451,#20452,#20453,
#20454,#20455,#20456,#20457,#20458,#20459,#20460,#20461,#20462,#20463,#20464,
#20465,#20466,#20467,#20468,#20469),.UNSPECIFIED.,.F.,.F.,(4,3,3,3,3,3,
3,3,3,3,3,3,3,3,4),(0.,0.000142261508827042,0.000306612281831946,0.000354680426257009,
0.000354839578464811,0.000671890822089835,0.000709360852514019,0.000709794319646003,
0.000798030959078271,0.00093103611892465,0.00106404127877103,0.00117707199637858,
0.00124138149189953,0.00135612593310508,0.00141872170502804),
 .UNSPECIFIED.);
#519=B_SPLINE_CURVE_WITH_KNOTS('',3,(#20476,#20477,#20478,#20479,#20480,
#20481,#20482,#20483,#20484,#20485,#20486,#20487,#20488,#20489,#20490,#20491,
#20492,#20493,#20494,#20495,#20496,#20497,#20498,#20499,#20500,#20501,#20502,
#20503,#20504,#20505,#20506,#20507,#20508,#20509,#20510,#20511,#20512,#20513,
#20514,#20515,#20516,#20517,#20518,#20519,#20520,#20521,#20522,#20523,#20524,
#20525,#20526,#20527,#20528,#20529,#20530),.UNSPECIFIED.,.F.,.F.,(4,3,3,
3,3,3,3,3,3,3,3,3,3,3,3,3,3,3,4),(0.,0.00292798214607904,0.00577262065187083,
0.00682756145262549,0.00693335737727645,0.00947217443522634,0.0103475581420103,
0.0104000360659147,0.0118697041221879,0.0132773954676776,0.0138667147545529,
0.013878114522684,0.0166264516377915,0.0173333934431911,0.0189487413423515,
0.0205003989924771,0.0210540430948269,0.0243937363016876,0.0277334295085483),
 .UNSPECIFIED.);
#520=B_SPLINE_CURVE_WITH_KNOTS('',3,(#20551,#20552,#20553,#20554,#20555,
#20556,#20557,#20558,#20559,#20560,#20561,#20562,#20563,#20564,#20565,#20566,
#20567,#20568,#20569,#20570,#20571,#20572,#20573,#20574,#20575,#20576,#20577,
#20578,#20579,#20580,#20581,#20582,#20583,#20584,#20585,#20586,#20587,#20588,
#20589,#20590),.UNSPECIFIED.,.F.,.F.,(4,3,3,3,3,3,3,3,3,3,3,3,3,4),(0.,
0.00261722397919538,0.00435913346757957,0.0043687095238485,0.00564078314595562,
0.00692512632512478,0.008186704139069,0.008737419047697,0.0087491646894187,
0.0122136782966271,0.0131061285715455,0.0147515701823087,0.016420240909498,
0.017474838095394),.UNSPECIFIED.);
#521=B_SPLINE_CURVE_WITH_KNOTS('',3,(#20636,#20637,#20638,#20639,#20640,
#20641,#20642,#20643,#20644,#20645,#20646,#20647,#20648),.UNSPECIFIED.,
 .F.,.F.,(4,3,3,3,4),(0.,0.000355508868042915,0.000556947538855278,0.000557267210332337,
0.00111453442066467),.UNSPECIFIED.);
#522=B_SPLINE_CURVE_WITH_KNOTS('',3,(#20650,#20651,#20652,#20653,#20654,
#20655,#20656,#20657,#20658,#20659,#20660,#20661,#20662,#20663,#20664,#20665,
#20666,#20667,#20668,#20669,#20670,#20671,#20672,#20673,#20674,#20675,#20676,
#20677,#20678,#20679,#20680,#20681,#20682,#20683,#20684,#20685,#20686,#20687,
#20688,#20689,#20690,#20691,#20692,#20693,#20694,#20695,#20696,#20697,#20698,
#20699,#20700,#20701,#20702,#20703,#20704,#20705,#20706,#20707,#20708,#20709,
#20710,#20711,#20712,#20713,#20714,#20715,#20716),.UNSPECIFIED.,.F.,.F.,
(4,3,3,3,3,3,3,3,3,3,3,3,3,3,3,3,3,3,3,3,3,3,4),(0.,0.00277040425654159,
0.00554080851308318,0.00557505688803485,0.00791560355762107,0.0083263576942907,
0.00836258533205228,0.0100018252550587,0.011122873465018,0.0111501137760697,
0.0223002275521394,0.0223209744612517,0.0250877559961568,0.025120499376563,
0.0278752844401743,0.0279173397075125,0.0311894101768246,0.0334503413282091,
0.0334957141052527,0.0369394202828642,0.040438907290041,0.044027168743403,
0.0446004551042788),.UNSPECIFIED.);
#523=B_SPLINE_CURVE_WITH_KNOTS('',3,(#20717,#20718,#20719,#20720,#20721,
#20722,#20723,#20724,#20725,#20726,#20727,#20728,#20729,#20730,#20731,#20732,
#20733,#20734,#20735),.UNSPECIFIED.,.F.,.F.,(4,3,3,3,3,3,4),(0.,0.000209520759737123,
0.000422285836605981,0.000553215152468032,0.000554217096220492,0.000897330597223569,
0.00110843419244098),.UNSPECIFIED.);
#524=B_SPLINE_CURVE_WITH_KNOTS('',3,(#20748,#20749,#20750,#20751,#20752,
#20753,#20754,#20755,#20756,#20757,#20758,#20759,#20760),.UNSPECIFIED.,
 .F.,.F.,(4,3,3,3,4),(0.,0.000732343305081284,0.00114589002873166,0.00114609016424997,
0.00229218032849994),.UNSPECIFIED.);
#525=B_SPLINE_CURVE_WITH_KNOTS('',3,(#20762,#20763,#20764,#20765,#20766,
#20767,#20768,#20769,#20770,#20771,#20772,#20773,#20774,#20775,#20776,#20777,
#20778,#20779,#20780,#20781,#20782,#20783,#20784,#20785,#20786,#20787,#20788,
#20789,#20790,#20791,#20792,#20793,#20794,#20795),.UNSPECIFIED.,.F.,.F.,
(4,3,3,3,3,3,3,3,3,3,3,4),(0.,0.0036541472315085,0.00727615609223089,0.00868437231710706,
0.00868483454405465,0.0100721107297951,0.0114668861300835,0.0128270292725488,
0.0130265584756606,0.0130435595235904,0.0155867439443868,0.0173687446342141),
 .UNSPECIFIED.);
#526=B_SPLINE_CURVE_WITH_KNOTS('',3,(#20797,#20798,#20799,#20800,#20801,
#20802,#20803,#20804,#20805,#20806,#20807,#20808,#20809),.UNSPECIFIED.,
 .F.,.F.,(4,3,3,3,4),(0.,0.000722789662749714,0.00114552600039176,0.00114627200830298,
0.00229254401660596),.UNSPECIFIED.);
#527=B_SPLINE_CURVE_WITH_KNOTS('',3,(#20819,#20820,#20821,#20822,#20823,
#20824,#20825,#20826),.UNSPECIFIED.,.F.,.F.,(4,2,2,4),(0.,0.00951523528670842,
0.0142728529300626,0.0190304705734168),.UNSPECIFIED.);
#528=B_SPLINE_CURVE_WITH_KNOTS('',3,(#20830,#20831,#20832,#20833,#20834,
#20835,#20836,#20837),.UNSPECIFIED.,.F.,.F.,(4,2,2,4),(0.,0.00476132581272552,
0.00952265162545105,0.0190453032509021),.UNSPECIFIED.);
#529=B_SPLINE_CURVE_WITH_KNOTS('',3,(#20844,#20845,#20846,#20847,#20848,
#20849,#20850,#20851,#20852,#20853,#20854,#20855,#20856,#20857,#20858,#20859,
#20860,#20861,#20862,#20863,#20864,#20865,#20866,#20867,#20868,#20869,#20870,
#20871,#20872,#20873,#20874,#20875,#20876,#20877),.UNSPECIFIED.,.F.,.F.,
(4,3,3,3,3,3,3,3,3,3,3,4),(0.00419407786743798,0.00785137041686624,0.00864322402522942,
0.00888216076442249,0.0105632172612883,0.0122879239673143,0.0130923701830209,
0.0136962196480359,0.0161859644983103,0.0187205501006744,0.0213309666507051,
0.0219906624986038),.UNSPECIFIED.);
#530=B_SPLINE_CURVE_WITH_KNOTS('',3,(#20881,#20882,#20883,#20884,#20885,
#20886,#20887,#20888,#20889,#20890,#20891,#20892,#20893,#20894,#20895,#20896,
#20897,#20898,#20899,#20900,#20901,#20902,#20903,#20904,#20905,#20906,#20907,
#20908,#20909,#20910,#20911,#20912,#20913,#20914),.UNSPECIFIED.,.F.,.F.,
(4,3,3,3,3,3,3,3,3,3,3,4),(0.,0.00259497273991662,0.00513490948980078,0.0076092056498656,
0.00831654261042356,0.00892204401521706,0.0106541774039888,0.0123507369870092,
0.0131434725515691,0.0133830660228256,0.017041266814901,0.0178440880304341),
 .UNSPECIFIED.);
#531=B_SPLINE_CURVE_WITH_KNOTS('',3,(#20919,#20920,#20921,#20922,#20923,
#20924),.UNSPECIFIED.,.F.,.F.,(4,2,4),(0.,0.00327855488628776,0.00654795604494929),
 .UNSPECIFIED.);
#532=B_SPLINE_CURVE_WITH_KNOTS('',3,(#20934,#20935,#20936,#20937,#20938,
#20939),.UNSPECIFIED.,.F.,.F.,(4,2,4),(0.,0.00326940115867351,0.00654795604497326),
 .UNSPECIFIED.);
#533=B_SPLINE_CURVE_WITH_KNOTS('',3,(#20962,#20963,#20964,#20965,#20966,
#20967,#20968),.UNSPECIFIED.,.F.,.F.,(4,3,4),(0.,0.00700450431179497,0.00878441731503681),
 .UNSPECIFIED.);
#534=B_SPLINE_CURVE_WITH_KNOTS('',3,(#20984,#20985,#20986,#20987),
 .UNSPECIFIED.,.F.,.F.,(4,4),(0.,0.00906386388585898),.UNSPECIFIED.);
#535=B_SPLINE_CURVE_WITH_KNOTS('',3,(#21029,#21030,#21031,#21032,#21033,
#21034,#21035,#21036,#21037,#21038,#21039,#21040,#21041,#21042,#21043,#21044,
#21045,#21046,#21047,#21048,#21049,#21050,#21051,#21052,#21053,#21054,#21055,
#21056,#21057,#21058,#21059,#21060,#21061,#21062,#21063,#21064,#21065,#21066,
#21067,#21068,#21069,#21070,#21071,#21072,#21073,#21074,#21075,#21076,#21077),
 .UNSPECIFIED.,.F.,.F.,(4,3,3,3,3,3,3,3,3,3,3,3,3,3,3,3,4),(0.,0.000121245606219857,
0.00024285714250704,0.000287360877759074,0.000288270017838685,0.000443403913075757,
0.000574721755518148,0.000575971165655791,0.000665917057795795,0.000718402194397685,
0.000790242413837453,0.000826162523557337,0.000862082633277221,0.000975072145653548,
0.00100576307215676,0.00111728780499056,0.0011494435110363),
 .UNSPECIFIED.);
#536=B_SPLINE_CURVE_WITH_KNOTS('',3,(#21083,#21084,#21085,#21086,#21087,
#21088,#21089,#21090),.UNSPECIFIED.,.F.,.F.,(4,2,2,4),(0.,0.0138082473482012,
0.0207123710223018,0.0276164946964024),.UNSPECIFIED.);
#537=B_SPLINE_CURVE_WITH_KNOTS('',3,(#21105,#21106,#21107,#21108,#21109,
#21110,#21111,#21112,#21113,#21114,#21115,#21116,#21117,#21118,#21119,#21120,
#21121,#21122,#21123,#21124,#21125,#21126,#21127,#21128,#21129,#21130,#21131,
#21132,#21133,#21134,#21135,#21136,#21137,#21138),.UNSPECIFIED.,.F.,.F.,
(4,3,3,3,3,3,3,3,3,3,3,4),(0.,0.000110567770962462,0.000229163742115291,
0.000349602944967853,0.000466129197406935,0.000503962612308805,0.000504370554078785,
0.000654658246624721,0.000733772187615348,0.000861351750904368,0.000986409541163883,
0.00100874110815757),.UNSPECIFIED.);
#538=B_SPLINE_CURVE_WITH_KNOTS('',3,(#21156,#21157,#21158,#21159,#21160,
#21161,#21162,#21163,#21164,#21165,#21166,#21167,#21168,#21169,#21170,#21171,
#21172,#21173,#21174,#21175,#21176,#21177,#21178,#21179,#21180,#21181,#21182,
#21183),.UNSPECIFIED.,.F.,.F.,(4,3,3,3,3,3,3,3,3,4),(0.,9.61627041725452E-5,
0.000194643124037966,0.000263598431963772,0.00026390914929366,0.000510523427664749,
0.000527611135930377,0.00052781829858732,0.000791654292983059,0.00105563659717466),
 .UNSPECIFIED.);
#539=B_SPLINE_CURVE_WITH_KNOTS('',3,(#21189,#21190,#21191,#21192,#21193,
#21194,#21195,#21196,#21197,#21198,#21199,#21200,#21201,#21202,#21203,#21204),
 .UNSPECIFIED.,.F.,.F.,(4,3,3,3,3,4),(4.52453455287509E-15,0.00201520691454269,
0.00402253547200752,0.00602595242278867,0.008023701719707,0.00993491157965328),
 .UNSPECIFIED.);
#540=B_SPLINE_CURVE_WITH_KNOTS('',3,(#21206,#21207,#21208,#21209,#21210,
#21211,#21212,#21213,#21214,#21215,#21216,#21217,#21218,#21219,#21220,#21221,
#21222,#21223,#21224,#21225,#21226,#21227,#21228,#21229,#21230,#21231,#21232,
#21233,#21234,#21235,#21236,#21237,#21238,#21239,#21240,#21241,#21242,#21243,
#21244,#21245,#21246,#21247,#21248),.UNSPECIFIED.,.F.,.F.,(4,3,3,3,3,3,
3,3,3,3,3,3,3,3,4),(0.,0.000142261508819856,0.000306612281818102,0.000354680426257006,
0.000354839578464825,0.000671890823263132,0.000709360852514012,0.000709794319645991,
0.000798030959078264,0.000931036118924641,0.00106404127877102,0.00117707199638153,
0.00124138149189952,0.00135612593304764,0.00141872170502802),
 .UNSPECIFIED.);
#541=B_SPLINE_CURVE_WITH_KNOTS('',3,(#21255,#21256,#21257,#21258,#21259,
#21260,#21261,#21262,#21263,#21264,#21265,#21266,#21267,#21268,#21269,#21270,
#21271,#21272,#21273,#21274,#21275,#21276,#21277,#21278,#21279,#21280,#21281,
#21282,#21283,#21284,#21285,#21286,#21287,#21288,#21289,#21290,#21291,#21292,
#21293,#21294,#21295,#21296,#21297,#21298,#21299,#21300,#21301,#21302,#21303,
#21304,#21305,#21306,#21307,#21308,#21309),.UNSPECIFIED.,.F.,.F.,(4,3,3,
3,3,3,3,3,3,3,3,3,3,3,3,3,3,3,4),(0.,0.00292798214153551,0.0057726206412551,
0.00682756145262537,0.00693335737727641,0.00947217442119118,0.0103475581420101,
0.0104000360659146,0.0118697041223215,0.013277395467897,0.0138667147545528,
0.0138781145226838,0.016626451636874,0.017333393443191,0.0189487413424095,
0.0205003989924608,0.0210540430948119,0.02439373630168,0.0277334295085482),
 .UNSPECIFIED.);
#542=B_SPLINE_CURVE_WITH_KNOTS('',3,(#21321,#21322,#21323,#21324,#21325,
#21326,#21327,#21328,#21329,#21330,#21331,#21332,#21333,#21334,#21335,#21336,
#21337,#21338,#21339,#21340,#21341,#21342,#21343,#21344,#21345,#21346,#21347,
#21348,#21349,#21350,#21351,#21352,#21353,#21354,#21355,#21356,#21357,#21358,
#21359,#21360),.UNSPECIFIED.,.F.,.F.,(4,3,3,3,3,3,3,3,3,3,3,3,3,4),(0.,
0.00261722398002284,0.00435913346757954,0.00436870952384852,0.00564078314584605,
0.00692512632493898,0.00818670413883311,0.00873741904769704,0.00874916468941873,
0.0122136783028313,0.0131061285715456,0.0147515701824667,0.0164202409098317,
0.0174748380953941),.UNSPECIFIED.);
#543=B_SPLINE_CURVE_WITH_KNOTS('',3,(#21365,#21366,#21367,#21368,#21369,
#21370,#21371,#21372,#21373,#21374,#21375,#21376,#21377,#21378,#21379,#21380,
#21381,#21382,#21383),.UNSPECIFIED.,.F.,.F.,(4,3,3,3,3,3,4),(0.,0.000209520759759855,
0.000422285836655203,0.000553215152468034,0.000554217096220497,0.000897330597719915,
0.00110843419244099),.UNSPECIFIED.);
#544=B_SPLINE_CURVE_WITH_KNOTS('',3,(#21395,#21396,#21397,#21398,#21399,
#21400,#21401,#21402,#21403,#21404,#21405,#21406,#21407),.UNSPECIFIED.,
 .F.,.F.,(4,3,3,3,4),(0.,0.0003555088680465,0.000556947538855288,0.000557267210332349,
0.0011145344206647),.UNSPECIFIED.);
#545=B_SPLINE_CURVE_WITH_KNOTS('',3,(#21408,#21409,#21410,#21411,#21412,
#21413,#21414,#21415,#21416,#21417,#21418,#21419,#21420,#21421,#21422,#21423,
#21424,#21425,#21426,#21427,#21428,#21429,#21430,#21431,#21432,#21433,#21434,
#21435,#21436,#21437,#21438,#21439,#21440,#21441,#21442,#21443,#21444,#21445,
#21446,#21447,#21448,#21449,#21450,#21451,#21452,#21453,#21454,#21455,#21456,
#21457,#21458,#21459,#21460,#21461,#21462,#21463,#21464,#21465,#21466,#21467,
#21468,#21469,#21470,#21471,#21472,#21473,#21474),.UNSPECIFIED.,.F.,.F.,
(4,3,3,3,3,3,3,3,3,3,3,3,3,3,3,3,3,3,3,3,3,3,4),(0.,0.00277040425654159,
0.00554080851308317,0.00557505688803486,0.00791560355474336,0.0083263576942907,
0.00836258533205228,0.0100018252550135,0.0111228734650181,0.0111501137760697,
0.0223002275521394,0.0223209744612517,0.0250877559961568,0.0251204993765631,
0.0278752844401743,0.0279173397075124,0.0311894101769749,0.0334503413282091,
0.0334957141052527,0.0369394202827702,0.0404389072898642,0.0440271687431145,
0.0446004551042788),.UNSPECIFIED.);
#546=B_SPLINE_CURVE_WITH_KNOTS('',3,(#21485,#21486,#21487,#21488,#21489,
#21490,#21491,#21492,#21493,#21494,#21495,#21496,#21497),.UNSPECIFIED.,
 .F.,.F.,(4,3,3,3,4),(0.,0.000732343305562431,0.00114589002873164,0.00114609016424995,
0.00229218032849991),.UNSPECIFIED.);
#547=B_SPLINE_CURVE_WITH_KNOTS('',3,(#21499,#21500,#21501,#21502,#21503,
#21504,#21505,#21506,#21507,#21508,#21509,#21510,#21511,#21512,#21513,#21514,
#21515,#21516,#21517,#21518,#21519,#21520,#21521,#21522,#21523,#21524,#21525,
#21526,#21527,#21528,#21529,#21530,#21531,#21532),.UNSPECIFIED.,.F.,.F.,
(4,3,3,3,3,3,3,3,3,3,3,4),(0.,0.00365414724118463,0.00727615611117417,0.0086843723171071,
0.0086848345440547,0.0100721107296907,0.0114668861299102,0.0128270292722496,
0.0130265584756607,0.0130435595235905,0.0155867439504688,0.0173687446342142),
 .UNSPECIFIED.);
#548=B_SPLINE_CURVE_WITH_KNOTS('',3,(#21534,#21535,#21536,#21537,#21538,
#21539,#21540,#21541,#21542,#21543,#21544,#21545,#21546),.UNSPECIFIED.,
 .F.,.F.,(4,3,3,3,4),(0.,0.000722789662613087,0.00114552600039172,0.00114627200830295,
0.00229254401660589),.UNSPECIFIED.);
#549=B_SPLINE_CURVE_WITH_KNOTS('',3,(#21558,#21559,#21560,#21561,#21562,
#21563,#21564,#21565),.UNSPECIFIED.,.F.,.F.,(4,2,2,4),(0.,0.00951523528670849,
0.0142728529300627,0.019030470573417),.UNSPECIFIED.);
#550=B_SPLINE_CURVE_WITH_KNOTS('',3,(#21569,#21570,#21571,#21572,#21573,
#21574,#21575,#21576),.UNSPECIFIED.,.F.,.F.,(4,2,2,4),(0.,0.00476132581272557,
0.00952265162545114,0.0190453032509023),.UNSPECIFIED.);
#551=B_SPLINE_CURVE_WITH_KNOTS('',3,(#21583,#21584,#21585,#21586,#21587,
#21588,#21589,#21590,#21591,#21592,#21593,#21594,#21595,#21596,#21597,#21598,
#21599,#21600,#21601,#21602,#21603,#21604,#21605,#21606,#21607,#21608,#21609,
#21610,#21611,#21612,#21613,#21614,#21615,#21616),.UNSPECIFIED.,.F.,.F.,
(4,3,3,3,3,3,3,3,3,3,3,4),(0.00419407786743743,0.00785137040303032,0.00864322402522884,
0.00888216076442196,0.0105632172608223,0.0122879239665899,0.0130923701830202,
0.0136962196480357,0.0161859644983781,0.0187205501007953,0.021330966650845,
0.0219906624986031),.UNSPECIFIED.);
#552=B_SPLINE_CURVE_WITH_KNOTS('',3,(#21620,#21621,#21622,#21623,#21624,
#21625,#21626,#21627,#21628,#21629,#21630,#21631,#21632,#21633,#21634,#21635,
#21636,#21637,#21638,#21639,#21640,#21641,#21642,#21643,#21644,#21645,#21646,
#21647,#21648,#21649,#21650,#21651,#21652,#21653),.UNSPECIFIED.,.F.,.F.,
(4,3,3,3,3,3,3,3,3,3,3,4),(0.,0.00259497273971206,0.00513490948937697,0.00760920564921991,
0.00831654261042337,0.00892204401521714,0.010654177403752,0.0123507369864928,
0.0131434725515693,0.0133830660228257,0.0170412668230596,0.0178440880304343),
 .UNSPECIFIED.);
#553=B_SPLINE_CURVE_WITH_KNOTS('',3,(#21658,#21659,#21660,#21661,#21662,
#21663),.UNSPECIFIED.,.F.,.F.,(4,2,4),(0.,0.00327855488628777,0.00654795604494931),
 .UNSPECIFIED.);
#554=B_SPLINE_CURVE_WITH_KNOTS('',3,(#21674,#21675,#21676,#21677,#21678,
#21679),.UNSPECIFIED.,.F.,.F.,(4,2,4),(0.,0.00326940115867351,0.00654795604497327),
 .UNSPECIFIED.);
#555=B_SPLINE_CURVE_WITH_KNOTS('',3,(#21705,#21706,#21707,#21708,#21709,
#21710,#21711),.UNSPECIFIED.,.F.,.F.,(4,3,4),(0.,0.00700450431517081,0.00878441731503683),
 .UNSPECIFIED.);
#556=B_SPLINE_CURVE_WITH_KNOTS('',3,(#21724,#21725,#21726,#21727),
 .UNSPECIFIED.,.F.,.F.,(4,4),(0.,0.00906386388585899),.UNSPECIFIED.);
#557=B_SPLINE_CURVE_WITH_KNOTS('',3,(#21782,#21783,#21784,#21785,#21786,
#21787,#21788,#21789,#21790,#21791,#21792,#21793,#21794,#21795,#21796,#21797,
#21798,#21799,#21800,#21801,#21802,#21803,#21804,#21805,#21806,#21807,#21808,
#21809,#21810,#21811,#21812,#21813,#21814,#21815,#21816,#21817,#21818,#21819,
#21820,#21821,#21822,#21823,#21824,#21825,#21826,#21827,#21828,#21829,#21830),
 .UNSPECIFIED.,.F.,.F.,(4,3,3,3,3,3,3,3,3,3,3,3,3,3,3,3,4),(0.,0.000121245606178752,
0.000242857142425659,0.000287360877759076,0.000288270017838685,0.000443403913041565,
0.000574721755518153,0.000575971165655798,0.000665917057788043,0.000718402194397691,
0.00079024241383746,0.000826162523557345,0.000862082633277229,0.000975072145641835,
0.00100576307215677,0.00111728780497355,0.00114944351103631),
 .UNSPECIFIED.);
#558=B_SPLINE_CURVE_WITH_KNOTS('',3,(#21836,#21837,#21838,#21839,#21840,
#21841,#21842,#21843),.UNSPECIFIED.,.F.,.F.,(4,2,2,4),(0.,0.0138082473482012,
0.0207123710223018,0.0276164946964023),.UNSPECIFIED.);
#559=B_SPLINE_CURVE_WITH_KNOTS('',3,(#21853,#21854,#21855,#21856,#21857,
#21858,#21859,#21860,#21861,#21862,#21863,#21864,#21865,#21866,#21867,#21868,
#21869,#21870,#21871,#21872,#21873,#21874,#21875,#21876,#21877,#21878,#21879,
#21880,#21881,#21882,#21883,#21884,#21885,#21886),.UNSPECIFIED.,.F.,.F.,
(4,3,3,3,3,3,3,3,3,3,3,4),(0.,0.000110567770974224,0.000229163742141399,
0.000349602945008942,0.000466129197462143,0.00050396261230882,0.00050437055407879,
0.000654658246767277,0.000733772187615245,0.000861351750994649,0.000986409541178866,
0.00100874110815758),.UNSPECIFIED.);
#560=B_SPLINE_CURVE_WITH_KNOTS('',3,(#21903,#21904,#21905,#21906,#21907,
#21908,#21909,#21910,#21911,#21912,#21913,#21914,#21915,#21916,#21917,#21918,
#21919,#21920,#21921,#21922,#21923,#21924,#21925,#21926,#21927,#21928,#21929,
#21930),.UNSPECIFIED.,.F.,.F.,(4,3,3,3,3,3,3,3,3,4),(0.,9.61627041694446E-5,
0.000194643124010955,0.000263598431963752,0.000263909149293657,0.000510523427602487,
0.000527611135930373,0.000527818298587313,0.000791654292982851,0.00105563659717465),
 .UNSPECIFIED.);
#561=B_SPLINE_CURVE_WITH_KNOTS('',3,(#21936,#21937,#21938,#21939,#21940,
#21941,#21942,#21943,#21944,#21945,#21946,#21947,#21948,#21949,#21950,#21951),
 .UNSPECIFIED.,.F.,.F.,(4,3,3,3,3,4),(4.53150918211895E-15,0.0020152069145278,
0.00402253547199676,0.0060259524227816,0.00802370171969666,0.00993491157965328),
 .UNSPECIFIED.);
#562=B_SPLINE_CURVE_WITH_KNOTS('',3,(#21953,#21954,#21955,#21956,#21957,
#21958,#21959,#21960,#21961,#21962,#21963,#21964,#21965,#21966,#21967,#21968,
#21969,#21970,#21971,#21972,#21973,#21974,#21975,#21976,#21977,#21978,#21979,
#21980,#21981,#21982,#21983,#21984,#21985,#21986,#21987,#21988,#21989,#21990,
#21991,#21992,#21993,#21994,#21995),.UNSPECIFIED.,.F.,.F.,(4,3,3,3,3,3,
3,3,3,3,3,3,3,3,4),(0.,0.000142261508866842,0.000306612281910534,0.000354680426257011,
0.000354839578464814,0.000671890822871748,0.000709360852514021,0.00070979431964599,
0.000798030959078274,0.000931036118924653,0.00106404127877103,0.0011770719963786,
0.00124138149189954,0.00135612593306929,0.00141872170502804),
 .UNSPECIFIED.);
#563=B_SPLINE_CURVE_WITH_KNOTS('',3,(#22002,#22003,#22004,#22005,#22006,
#22007,#22008,#22009,#22010,#22011,#22012,#22013,#22014,#22015,#22016,#22017,
#22018,#22019,#22020,#22021,#22022,#22023,#22024,#22025,#22026,#22027,#22028,
#22029,#22030,#22031,#22032,#22033,#22034,#22035,#22036,#22037,#22038,#22039,
#22040,#22041,#22042,#22043,#22044,#22045,#22046,#22047,#22048,#22049,#22050,
#22051,#22052,#22053,#22054,#22055,#22056),.UNSPECIFIED.,.F.,.F.,(4,3,3,
3,3,3,3,3,3,3,3,3,3,3,3,3,3,3,4),(0.,0.00292798214826902,0.00577262065532403,
0.00682756145262549,0.00693335737727643,0.00947217443781762,0.0103475581420102,
0.0104000360659147,0.0118697041220001,0.0132773954673753,0.0138667147545529,
0.013878114522684,0.0166264516375164,0.0173333934431911,0.0189487413423672,
0.0205003989924343,0.021054043092682,0.0243937363006151,0.0277334295085482),
 .UNSPECIFIED.);
#564=B_SPLINE_CURVE_WITH_KNOTS('',3,(#22097,#22098,#22099,#22100,#22101,
#22102,#22103,#22104),.UNSPECIFIED.,.F.,.F.,(4,2,2,4),(0.,0.00951523528670844,
0.0142728529300627,0.0190304705734169),.UNSPECIFIED.);
#565=B_SPLINE_CURVE_WITH_KNOTS('',3,(#22108,#22109,#22110,#22111,#22112,
#22113,#22114,#22115),.UNSPECIFIED.,.F.,.F.,(4,2,2,4),(0.,0.00476132581272554,
0.00952265162545108,0.0190453032509022),.UNSPECIFIED.);
#566=B_SPLINE_CURVE_WITH_KNOTS('',3,(#22120,#22121,#22122,#22123,#22124,
#22125),.UNSPECIFIED.,.F.,.F.,(4,2,4),(0.,0.0032785548862878,0.00654795604494929),
 .UNSPECIFIED.);
#567=B_SPLINE_CURVE_WITH_KNOTS('',3,(#22136,#22137,#22138,#22139,#22140,
#22141),.UNSPECIFIED.,.F.,.F.,(4,2,4),(0.,0.00326940115867351,0.00654795604497326),
 .UNSPECIFIED.);
#568=B_SPLINE_CURVE_WITH_KNOTS('',3,(#22162,#22163,#22164,#22165,#22166,
#22167,#22168),.UNSPECIFIED.,.F.,.F.,(4,3,4),(1.73472347597681E-18,0.00700450431037659,
0.00878441731503682),.UNSPECIFIED.);
#569=B_SPLINE_CURVE_WITH_KNOTS('',3,(#22183,#22184,#22185,#22186),
 .UNSPECIFIED.,.F.,.F.,(4,4),(0.,0.009063863885859),.UNSPECIFIED.);
#570=B_SPLINE_CURVE_WITH_KNOTS('',3,(#22315,#22316,#22317,#22318,#22319,
#22320),.UNSPECIFIED.,.F.,.F.,(4,2,4),(0.,0.5,1.),.UNSPECIFIED.);
#571=B_SPLINE_CURVE_WITH_KNOTS('',3,(#22322,#22323,#22324,#22325,#22326,
#22327,#22328,#22329,#22330,#22331,#22332,#22333,#22334,#22335,#22336,#22337),
 .UNSPECIFIED.,.F.,.F.,(4,3,3,3,3,4),(0.,0.269515461283795,0.518490249146468,
0.759245124573234,0.982227995954739,1.),.UNSPECIFIED.);
#572=B_SPLINE_CURVE_WITH_KNOTS('',3,(#22338,#22339,#22340,#22341,#22342,
#22343),.UNSPECIFIED.,.F.,.F.,(4,2,4),(0.,0.5,1.),.UNSPECIFIED.);
#573=B_SPLINE_CURVE_WITH_KNOTS('',3,(#22408,#22409,#22410,#22411),
 .UNSPECIFIED.,.F.,.F.,(4,4),(0.,0.99999526872431),.UNSPECIFIED.);
#574=B_SPLINE_CURVE_WITH_KNOTS('',3,(#22413,#22414,#22415,#22416,#22417,
#22418),.UNSPECIFIED.,.F.,.F.,(4,2,4),(7.44333906889603E-6,0.5,1.),
 .UNSPECIFIED.);
#575=B_SPLINE_CURVE_WITH_KNOTS('',3,(#22419,#22420,#22421,#22422,#22423,
#22424),.UNSPECIFIED.,.F.,.F.,(4,2,4),(0.,0.5,1.),.UNSPECIFIED.);
#576=B_SPLINE_CURVE_WITH_KNOTS('',3,(#22473,#22474,#22475,#22476,#22477,
#22478,#22479,#22480,#22481,#22482,#22483,#22484,#22485,#22486,#22487,#22488),
 .UNSPECIFIED.,.F.,.F.,(4,3,3,3,3,4),(0.,0.2058948841142,0.424353797242841,
0.652795164048127,0.901134029685474,1.),.UNSPECIFIED.);
#577=B_SPLINE_CURVE_WITH_KNOTS('',3,(#22489,#22490,#22491,#22492,#22493,
#22494),.UNSPECIFIED.,.F.,.F.,(4,2,4),(0.,0.5,1.),.UNSPECIFIED.);
#578=B_SPLINE_CURVE_WITH_KNOTS('',3,(#22544,#22545,#22546,#22547,#22548,
#22549,#22550,#22551,#22552,#22553,#22554,#22555,#22556,#22557,#22558,#22559),
 .UNSPECIFIED.,.F.,.F.,(4,3,3,3,3,4),(0.,0.249999999999982,0.478354309316489,
0.695627207633627,0.902571772792554,0.999999999999926),.UNSPECIFIED.);
#579=B_SPLINE_CURVE_WITH_KNOTS('',3,(#22560,#22561,#22562,#22563,#22564,
#22565),.UNSPECIFIED.,.F.,.F.,(4,2,4),(0.,0.5,1.),.UNSPECIFIED.);
#580=B_SPLINE_CURVE_WITH_KNOTS('',3,(#22630,#22631,#22632,#22633,#22634,
#22635),.UNSPECIFIED.,.F.,.F.,(4,2,4),(0.,0.5,1.),.UNSPECIFIED.);
#581=B_SPLINE_CURVE_WITH_KNOTS('',3,(#22637,#22638,#22639,#22640,#22641,
#22642,#22643,#22644,#22645,#22646,#22647,#22648,#22649,#22650,#22651,#22652,
#22653,#22654,#22655,#22656,#22657,#22658,#22659,#22660,#22661,#22662,#22663,
#22664,#22665,#22666,#22667,#22668,#22669,#22670,#22671,#22672,#22673,#22674,
#22675,#22676,#22677,#22678,#22679,#22680,#22681,#22682,#22683,#22684,#22685,
#22686,#22687,#22688,#22689,#22690,#22691),.UNSPECIFIED.,.F.,.F.,(4,3,3,
3,3,3,3,3,3,3,3,3,3,3,3,3,3,3,4),(0.,0.134829595806097,0.3019357508242,
0.331938859566891,0.520486711309055,0.653948260259039,0.766867847735502,
0.847465247187294,0.903670142103914,0.941441061010362,0.964211312778628,
0.978961681102042,0.986981564546894,0.993490782273447,0.996745391136724,
0.998372695568362,0.999186347492603,0.999785290684486,0.999999999416845),
 .UNSPECIFIED.);
#582=B_SPLINE_CURVE_WITH_KNOTS('',3,(#22692,#22693,#22694,#22695,#22696,
#22697),.UNSPECIFIED.,.F.,.F.,(4,2,4),(0.,0.5,1.),.UNSPECIFIED.);
#583=B_SPLINE_CURVE_WITH_KNOTS('',3,(#22748,#22749,#22750,#22751,#22752,
#22753),.UNSPECIFIED.,.F.,.F.,(4,2,4),(0.,0.5,1.),.UNSPECIFIED.);
#584=B_SPLINE_CURVE_WITH_KNOTS('',3,(#22754,#22755,#22756,#22757,#22758,
#22759,#22760,#22761,#22762,#22763,#22764,#22765,#22766,#22767,#22768,#22769),
 .UNSPECIFIED.,.F.,.F.,(4,3,3,3,3,4),(0.,0.205894884114374,0.424353797243356,
0.652795164048942,0.901134029686469,1.),.UNSPECIFIED.);
#585=B_SPLINE_CURVE_WITH_KNOTS('',3,(#22770,#22771,#22772,#22773,#22774,
#22775),.UNSPECIFIED.,.F.,.F.,(4,2,4),(0.,0.5,1.),.UNSPECIFIED.);
#586=B_SPLINE_CURVE_WITH_KNOTS('',3,(#22825,#22826,#22827,#22828,#22829,
#22830,#22831,#22832,#22833,#22834,#22835,#22836,#22837,#22838,#22839,#22840),
 .UNSPECIFIED.,.F.,.F.,(4,3,3,3,3,4),(0.,0.25,0.478354309317608,0.695627207636338,
0.90257177279645,1.),.UNSPECIFIED.);
#587=B_SPLINE_CURVE_WITH_KNOTS('',3,(#22841,#22842,#22843,#22844,#22845,
#22846),.UNSPECIFIED.,.F.,.F.,(4,2,4),(0.,0.5,1.),.UNSPECIFIED.);
#588=B_SPLINE_CURVE_WITH_KNOTS('',3,(#22911,#22912,#22913,#22914,#22915,
#22916),.UNSPECIFIED.,.F.,.F.,(4,2,4),(0.,0.5,1.),.UNSPECIFIED.);
#589=B_SPLINE_CURVE_WITH_KNOTS('',3,(#22918,#22919,#22920,#22921),
 .UNSPECIFIED.,.F.,.F.,(4,4),(0.,1.),.UNSPECIFIED.);
#590=B_SPLINE_CURVE_WITH_KNOTS('',3,(#22922,#22923,#22924,#22925,#22926,
#22927),.UNSPECIFIED.,.F.,.F.,(4,2,4),(0.,0.5,1.),.UNSPECIFIED.);
#591=B_SPLINE_CURVE_WITH_KNOTS('',3,(#22988,#22989,#22990,#22991,#22992,
#22993,#22994,#22995,#22996,#22997,#22998,#22999,#23000),.UNSPECIFIED.,
 .F.,.F.,(4,3,3,3,4),(0.,0.223169250633758,0.461855220689223,0.714975201891676,
1.),.UNSPECIFIED.);
#592=B_SPLINE_CURVE_WITH_KNOTS('',3,(#23001,#23002,#23003,#23004,#23005,
#23006),.UNSPECIFIED.,.F.,.F.,(4,2,4),(0.,0.5,1.),.UNSPECIFIED.);
#593=B_SPLINE_CURVE_WITH_KNOTS('',3,(#23069,#23070,#23071,#23072,#23073,
#23074),.UNSPECIFIED.,.F.,.F.,(4,2,4),(0.,0.5,1.),.UNSPECIFIED.);
#594=B_SPLINE_CURVE_WITH_KNOTS('',3,(#23136,#23137,#23138,#23139,#23140,
#23141),.UNSPECIFIED.,.F.,.F.,(4,2,4),(0.,0.5,1.),.UNSPECIFIED.);
#595=B_SPLINE_CURVE_WITH_KNOTS('',3,(#23143,#23144,#23145,#23146,#23147,
#23148,#23149,#23150,#23151,#23152,#23153,#23154,#23155,#23156,#23157,#23158),
 .UNSPECIFIED.,.F.,.F.,(4,3,3,3,3,4),(0.,0.269515461284035,0.518490249146748,
0.759245124573374,0.982227995955184,1.),.UNSPECIFIED.);
#596=B_SPLINE_CURVE_WITH_KNOTS('',3,(#23159,#23160,#23161,#23162,#23163,
#23164),.UNSPECIFIED.,.F.,.F.,(4,2,4),(0.,0.5,1.),.UNSPECIFIED.);
#597=B_SPLINE_CURVE_WITH_KNOTS('',3,(#23229,#23230,#23231,#23232),
 .UNSPECIFIED.,.F.,.F.,(4,4),(0.,0.999995268720932),.UNSPECIFIED.);
#598=B_SPLINE_CURVE_WITH_KNOTS('',3,(#23234,#23235,#23236,#23237,#23238,
#23239),.UNSPECIFIED.,.F.,.F.,(4,2,4),(7.44334456133663E-6,0.5,1.),
 .UNSPECIFIED.);
#599=B_SPLINE_CURVE_WITH_KNOTS('',3,(#23240,#23241,#23242,#23243,#23244,
#23245),.UNSPECIFIED.,.F.,.F.,(4,2,4),(0.,0.5,1.),.UNSPECIFIED.);
#600=B_SPLINE_CURVE_WITH_KNOTS('',3,(#23294,#23295,#23296,#23297,#23298,
#23299,#23300,#23301,#23302,#23303,#23304,#23305,#23306,#23307,#23308,#23309),
 .UNSPECIFIED.,.F.,.F.,(4,3,3,3,3,4),(0.,0.205894884114519,0.424353797243679,
0.652795164049289,0.901134029687007,1.),.UNSPECIFIED.);
#601=B_SPLINE_CURVE_WITH_KNOTS('',3,(#23310,#23311,#23312,#23313,#23314,
#23315),.UNSPECIFIED.,.F.,.F.,(4,2,4),(0.,0.5,1.),.UNSPECIFIED.);
#602=B_SPLINE_CURVE_WITH_KNOTS('',3,(#23365,#23366,#23367,#23368,#23369,
#23370,#23371,#23372,#23373,#23374,#23375,#23376,#23377,#23378,#23379,#23380),
 .UNSPECIFIED.,.F.,.F.,(4,3,3,3,3,4),(0.,0.25,0.478354309316686,0.695627207634347,
0.902571772793475,1.),.UNSPECIFIED.);
#603=B_SPLINE_CURVE_WITH_KNOTS('',3,(#23381,#23382,#23383,#23384,#23385,
#23386),.UNSPECIFIED.,.F.,.F.,(4,2,4),(0.,0.5,1.),.UNSPECIFIED.);
#604=B_SPLINE_CURVE_WITH_KNOTS('',3,(#23451,#23452,#23453,#23454,#23455,
#23456),.UNSPECIFIED.,.F.,.F.,(4,2,4),(0.,0.5,1.),.UNSPECIFIED.);
#605=B_SPLINE_CURVE_WITH_KNOTS('',3,(#23458,#23459,#23460,#23461,#23462,
#23463,#23464,#23465,#23466,#23467,#23468,#23469,#23470,#23471,#23472,#23473,
#23474,#23475,#23476,#23477,#23478,#23479,#23480,#23481,#23482,#23483,#23484,
#23485,#23486,#23487,#23488,#23489,#23490,#23491,#23492,#23493,#23494,#23495,
#23496,#23497,#23498,#23499,#23500,#23501,#23502,#23503,#23504,#23505,#23506,
#23507,#23508,#23509,#23510,#23511,#23512),.UNSPECIFIED.,.F.,.F.,(4,3,3,
3,3,3,3,3,3,3,3,3,3,3,3,3,3,3,4),(0.,0.134829323934977,0.301935713922455,
0.331938859566998,0.520486828090896,0.653948260259002,0.765695413226449,
0.845739444745421,0.901726372988166,0.939310870056937,0.962010943846672,
0.977750863055006,0.9886476997431,0.993490782263339,0.99674539113167,0.998372695565835,
0.999186347491368,0.999785290683289,0.999999999416902),.UNSPECIFIED.);
#606=B_SPLINE_CURVE_WITH_KNOTS('',3,(#23513,#23514,#23515,#23516,#23517,
#23518),.UNSPECIFIED.,.F.,.F.,(4,2,4),(0.,0.5,1.),.UNSPECIFIED.);
#607=B_SPLINE_CURVE_WITH_KNOTS('',3,(#23569,#23570,#23571,#23572,#23573,
#23574),.UNSPECIFIED.,.F.,.F.,(4,2,4),(0.,0.5,1.),.UNSPECIFIED.);
#608=B_SPLINE_CURVE_WITH_KNOTS('',3,(#23575,#23576,#23577,#23578,#23579,
#23580,#23581,#23582,#23583,#23584,#23585,#23586,#23587,#23588,#23589,#23590),
 .UNSPECIFIED.,.F.,.F.,(4,3,3,3,3,4),(0.,0.205894884112877,0.424353797240785,
0.652795164045189,0.901134029682195,1.),.UNSPECIFIED.);
#609=B_SPLINE_CURVE_WITH_KNOTS('',3,(#23591,#23592,#23593,#23594,#23595,
#23596),.UNSPECIFIED.,.F.,.F.,(4,2,4),(0.,0.5,1.),.UNSPECIFIED.);
#610=B_SPLINE_CURVE_WITH_KNOTS('',3,(#23646,#23647,#23648,#23649,#23650,
#23651,#23652,#23653,#23654,#23655,#23656,#23657,#23658,#23659,#23660,#23661),
 .UNSPECIFIED.,.F.,.F.,(4,3,3,3,3,4),(0.,0.25,0.478354309316566,0.695627207633873,
0.902571772792968,1.),.UNSPECIFIED.);
#611=B_SPLINE_CURVE_WITH_KNOTS('',3,(#23662,#23663,#23664,#23665,#23666,
#23667),.UNSPECIFIED.,.F.,.F.,(4,2,4),(0.,0.5,1.),.UNSPECIFIED.);
#612=B_SPLINE_CURVE_WITH_KNOTS('',3,(#23732,#23733,#23734,#23735,#23736,
#23737),.UNSPECIFIED.,.F.,.F.,(4,2,4),(0.,0.5,1.),.UNSPECIFIED.);
#613=B_SPLINE_CURVE_WITH_KNOTS('',3,(#23739,#23740,#23741,#23742),
 .UNSPECIFIED.,.F.,.F.,(4,4),(0.,1.),.UNSPECIFIED.);
#614=B_SPLINE_CURVE_WITH_KNOTS('',3,(#23743,#23744,#23745,#23746,#23747,
#23748),.UNSPECIFIED.,.F.,.F.,(4,2,4),(0.,0.5,1.),.UNSPECIFIED.);
#615=B_SPLINE_CURVE_WITH_KNOTS('',3,(#23809,#23810,#23811,#23812,#23813,
#23814,#23815,#23816,#23817,#23818,#23819,#23820,#23821),.UNSPECIFIED.,
 .F.,.F.,(4,3,3,3,4),(0.,0.223169250633671,0.461855220688962,0.714975201891147,
1.),.UNSPECIFIED.);
#616=B_SPLINE_CURVE_WITH_KNOTS('',3,(#23822,#23823,#23824,#23825,#23826,
#23827),.UNSPECIFIED.,.F.,.F.,(4,2,4),(0.,0.5,1.),.UNSPECIFIED.);
#617=B_SPLINE_CURVE_WITH_KNOTS('',3,(#23890,#23891,#23892,#23893,#23894,
#23895),.UNSPECIFIED.,.F.,.F.,(4,2,4),(0.,0.5,1.),.UNSPECIFIED.);
#618=B_SPLINE_CURVE_WITH_KNOTS('',3,(#23908,#23909,#23910,#23911,#23912,
#23913,#23914,#23915,#23916,#23917,#23918,#23919,#23920,#23921,#23922,#23923,
#23924,#23925,#23926,#23927,#23928,#23929,#23930,#23931,#23932,#23933,#23934,
#23935,#23936,#23937,#23938,#23939,#23940,#23941,#23942,#23943,#23944,#23945,
#23946,#23947,#23948,#23949,#23950,#23951,#23952,#23953,#23954,#23955,#23956,
#23957,#23958,#23959,#23960,#23961,#23962,#23963,#23964,#23965,#23966,#23967,
#23968,#23969,#23970,#23971,#23972,#23973,#23974,#23975,#23976,#23977,#23978,
#23979,#23980,#23981,#23982,#23983),.UNSPECIFIED.,.F.,.F.,(4,3,3,3,3,3,
3,3,3,3,3,3,3,3,3,3,3,3,3,3,3,3,3,3,3,4),(0.,1.95383290192994E-5,4.88458225482484E-5,
6.3499569312723E-5,6.71630060038416E-5,7.26581610405195E-5,7.81533160771975E-5,
0.000107954788053304,0.000117229974115796,0.000122114556370621,0.000124319385320046,
0.000126388565843593,0.000156306632154395,0.000183190273141628,0.000195383290192993,
0.000210037036957468,0.000222859065376383,0.000260630252152872,0.000268336943281978,
0.000312613264308788,0.000345493122408439,0.000400681528988149,0.000461636530308903,
0.000526902227788225,0.000600651716916799,0.00062522616402666),
 .UNSPECIFIED.);
#619=B_SPLINE_CURVE_WITH_KNOTS('',3,(#24010,#24011,#24012,#24013,#24014,
#24015,#24016,#24017,#24018,#24019,#24020,#24021,#24022,#24023,#24024,#24025,
#24026,#24027,#24028,#24029,#24030,#24031,#24032,#24033,#24034,#24035,#24036,
#24037,#24038,#24039,#24040,#24041,#24042,#24043,#24044,#24045,#24046,#24047,
#24048,#24049,#24050,#24051,#24052,#24053,#24054,#24055,#24056,#24057,#24058,
#24059,#24060,#24061,#24062,#24063,#24064,#24065,#24066,#24067),
 .UNSPECIFIED.,.F.,.F.,(4,3,3,3,3,3,3,3,3,3,3,3,3,3,3,3,3,3,3,4),(0.,8.33528450034202E-5,
0.000157226441487617,0.000225533822547471,0.00028951662415279,0.000348414967230199,
0.000378847230940207,0.000425063895935628,0.000434497171244448,0.000472969202699083,
0.000509314375642632,0.000542883032634857,0.000568270846410307,0.000610359908966051,
0.000640506736109503,0.000662982654145361,0.000689264740462159,0.000715678191795904,
0.000742518573435838,0.000757694461880414),.UNSPECIFIED.);
#620=B_SPLINE_CURVE_WITH_KNOTS('',3,(#24131,#24132,#24133,#24134,#24135,
#24136,#24137,#24138,#24139,#24140,#24141,#24142,#24143,#24144,#24145,#24146,
#24147,#24148,#24149,#24150,#24151,#24152,#24153,#24154,#24155),
 .UNSPECIFIED.,.F.,.F.,(4,3,3,3,3,3,3,3,4),(0.,8.77855222411457E-5,0.000180911661749747,
0.000284642473054724,0.000399672366761005,0.000487602524799653,0.000496563116819161,
0.000792478626183723,0.000993116632308356),.UNSPECIFIED.);
#621=B_SPLINE_CURVE_WITH_KNOTS('',3,(#24186,#24187,#24188,#24189,#24190,
#24191,#24192,#24193,#24194,#24195,#24196,#24197,#24198,#24199,#24200,#24201,
#24202,#24203,#24204,#24205,#24206,#24207,#24208,#24209,#24210),
 .UNSPECIFIED.,.F.,.F.,(4,3,3,3,3,3,3,3,4),(9.46798387615072E-9,0.000265027614959612,
0.000494820327889037,0.000505114957780789,0.000628257448099428,0.000739957890430424,
0.00084406403792606,0.000940011289227427,0.000989640655778074),
 .UNSPECIFIED.);
#622=B_SPLINE_CURVE_WITH_KNOTS('',3,(#24211,#24212,#24213,#24214,#24215,
#24216),.UNSPECIFIED.,.F.,.F.,(4,2,4),(7.44333395304289E-6,0.5,1.),
 .UNSPECIFIED.);
#623=B_SPLINE_CURVE_WITH_KNOTS('',3,(#24268,#24269,#24270,#24271,#24272,
#24273,#24274,#24275,#24276,#24277,#24278,#24279,#24280,#24281,#24282,#24283,
#24284,#24285,#24286,#24287,#24288,#24289,#24290,#24291,#24292,#24293,#24294,
#24295,#24296,#24297,#24298,#24299,#24300,#24301,#24302,#24303,#24304,#24305,
#24306,#24307,#24308,#24309,#24310,#24311,#24312,#24313,#24314,#24315,#24316,
#24317,#24318,#24319),.UNSPECIFIED.,.F.,.F.,(4,3,3,3,3,3,3,3,3,3,3,3,3,
3,3,3,3,4),(0.,4.1276445995066E-5,8.42546564931361E-5,0.000129571564840061,
0.000139714696155289,0.00019740107551137,0.000258094770764446,0.000279429392310577,
0.000359695196555143,0.000442730223930049,0.000529248927812506,0.000558858784621132,
0.000667945714892336,0.000780388678479812,0.000891339019476349,0.0010045282943593,
0.00110832362887639,0.00111771756924224),.UNSPECIFIED.);
#624=B_SPLINE_CURVE_WITH_KNOTS('',3,(#24386,#24387,#24388,#24389,#24390,
#24391,#24392,#24393,#24394,#24395,#24396,#24397,#24398,#24399,#24400,#24401,
#24402,#24403,#24404,#24405,#24406,#24407,#24408,#24409,#24410,#24411,#24412,
#24413,#24414,#24415,#24416,#24417,#24418,#24419,#24420,#24421,#24422,#24423,
#24424,#24425,#24426,#24427,#24428,#24429,#24430,#24431,#24432,#24433,#24434,
#24435,#24436,#24437,#24438,#24439,#24440),.UNSPECIFIED.,.F.,.F.,(4,3,3,
3,3,3,3,3,3,3,3,3,3,3,3,3,3,3,4),(1.00003361382536E-7,0.000627368768300138,
0.00125605092262165,0.00251210184524329,0.00502420369048659,0.013553717306397,
0.023404944736136,0.0239781242527868,0.0394341509419622,0.0631200523923673,
0.106735413774525,0.174618556157698,0.276325871435081,0.346051748925113,
0.519710818552453,0.668061140433113,0.834030570216557,0.968862390059979,
1.),.UNSPECIFIED.);
#625=B_SPLINE_CURVE_WITH_KNOTS('',3,(#24474,#24475,#24476,#24477,#24478,
#24479,#24480,#24481,#24482,#24483,#24484,#24485,#24486,#24487,#24488,#24489,
#24490,#24491,#24492,#24493,#24494,#24495,#24496,#24497,#24498,#24499,#24500,
#24501,#24502,#24503,#24504,#24505,#24506,#24507,#24508,#24509,#24510,#24511,
#24512,#24513,#24514,#24515,#24516,#24517,#24518,#24519),.UNSPECIFIED.,
 .F.,.F.,(4,3,3,3,3,3,3,3,3,3,3,3,3,3,3,4),(0.,9.72968081736543E-5,0.000188076340042391,
0.000274624933132362,0.000355070980215829,0.000389187232694617,0.000449617363167268,
0.000507814172801453,0.000562918686627687,0.000583780849041926,0.00062425089166696,
0.000662781785097529,0.000699618916511921,0.000735289518531963,0.000769568105219451,
0.000778374465389236),.UNSPECIFIED.);
#626=B_SPLINE_CURVE_WITH_KNOTS('',3,(#24523,#24524,#24525,#24526,#24527,
#24528,#24529,#24530,#24531,#24532,#24533,#24534,#24535,#24536,#24537,#24538,
#24539,#24540,#24541,#24542,#24543,#24544,#24545,#24546,#24547,#24548,#24549,
#24550,#24551,#24552,#24553,#24554,#24555,#24556),.UNSPECIFIED.,.F.,.F.,
(4,3,3,3,3,3,3,3,3,3,3,4),(0.,6.4784657425023E-5,0.000128085038055946,0.00019334280002843,
0.000254275817474415,0.000258600562000915,0.000269706482902608,0.000323662397377516,
0.000382521450096718,0.000443803383543172,0.00050542857129966,0.000539412965805216),
 .UNSPECIFIED.);
#627=B_SPLINE_CURVE_WITH_KNOTS('',3,(#24569,#24570,#24571,#24572,#24573,
#24574,#24575,#24576,#24577,#24578,#24579,#24580),.UNSPECIFIED.,.F.,.F.,
(4,2,2,2,2,4),(9.94226249721363E-9,0.000325172939224849,0.000650345878449699,
0.000975518817674548,0.00113810528728698,0.0013006917568994),
 .UNSPECIFIED.);
#628=B_SPLINE_CURVE_WITH_KNOTS('',3,(#24634,#24635,#24636,#24637,#24638,
#24639,#24640,#24641,#24642,#24643,#24644,#24645),.UNSPECIFIED.,.F.,.F.,
(4,2,2,2,2,4),(9.94226628845883E-9,0.000325172939224847,0.000650345878449693,
0.00097551881767454,0.00113810528728697,0.00130069175689939),
 .UNSPECIFIED.);
#629=B_SPLINE_CURVE_WITH_KNOTS('',3,(#24714,#24715,#24716,#24717,#24718,
#24719,#24720,#24721,#24722,#24723,#24724,#24725,#24726,#24727,#24728,#24729,
#24730,#24731,#24732,#24733,#24734,#24735,#24736,#24737,#24738),
 .UNSPECIFIED.,.F.,.F.,(4,3,3,3,3,3,3,3,4),(0.,9.58519120578613E-5,0.000201048393011152,
0.000313533962690052,0.000443358794827932,0.000487856029895832,0.000498221418747222,
0.000765061137597118,0.000996433304434568),.UNSPECIFIED.);
#630=B_SPLINE_CURVE_WITH_KNOTS('',3,(#24771,#24772,#24773,#24774,#24775,
#24776,#24777,#24778,#24779,#24780,#24781,#24782,#24783,#24784,#24785,#24786,
#24787,#24788,#24789,#24790,#24791,#24792,#24793,#24794,#24795),
 .UNSPECIFIED.,.F.,.F.,(4,3,3,3,3,3,3,3,4),(0.,8.88404632360193E-5,0.000183111749600284,
0.000288167720068051,0.000405111512909157,0.000488005422625335,0.000496805101503793,
0.000790206339202793,0.000993600597453218),.UNSPECIFIED.);
#631=B_SPLINE_CURVE_WITH_KNOTS('',3,(#24882,#24883,#24884,#24885,#24886,
#24887,#24888,#24889,#24890,#24891,#24892,#24893,#24894,#24895,#24896,#24897,
#24898,#24899,#24900,#24901,#24902,#24903,#24904,#24905,#24906,#24907,#24908,
#24909,#24910,#24911,#24912,#24913,#24914,#24915,#24916,#24917,#24918,#24919,
#24920,#24921,#24922,#24923,#24924,#24925,#24926,#24927,#24928,#24929,#24930,
#24931,#24932,#24933),.UNSPECIFIED.,.F.,.F.,(4,3,3,3,3,3,3,3,3,3,3,3,3,
3,3,3,3,4),(0.,4.12764459950958E-5,8.42546564931839E-5,0.000129571564840137,
0.000139714696155272,0.000197401075511458,0.000258094770764663,0.000279429392310544,
0.000359695196555155,0.0004427302239301,0.000529248927812585,0.000558858784621111,
0.000667945714892309,0.000780388678479793,0.000891339019476335,0.00100452829435929,
0.0011083236288764,0.00111771756924224),.UNSPECIFIED.);
#632=B_SPLINE_CURVE_WITH_KNOTS('',3,(#24965,#24966,#24967,#24968,#24969,
#24970,#24971,#24972,#24973,#24974,#24975,#24976,#24977,#24978,#24979,#24980,
#24981,#24982,#24983,#24984,#24985,#24986,#24987,#24988,#24989,#24990,#24991,
#24992,#24993,#24994,#24995,#24996,#24997,#24998,#24999,#25000,#25001,#25002,
#25003,#25004,#25005,#25006,#25007,#25008,#25009,#25010,#25011,#25012,#25013,
#25014,#25015,#25016,#25017,#25018,#25019,#25020,#25021,#25022,#25023,#25024,
#25025,#25026,#25027,#25028),.UNSPECIFIED.,.F.,.F.,(4,3,3,3,3,3,3,3,3,3,
3,3,3,3,3,3,3,3,3,3,3,4),(0.,9.68515416477823E-5,0.000192020529402715,0.000279284320016411,
0.00036189847675362,0.000438321326769842,0.000477527492667515,0.000529607759318425,
0.000578407666764912,0.000625243185949314,0.000670767212475296,0.000713433961486794,
0.000716291239001278,0.0007544629939221,0.000791422812842767,0.000826961927143274,
0.00083567311216816,0.000863826223827008,0.000892456091105036,0.000921613281236568,
0.000951948647270463,0.000955054985335042),.UNSPECIFIED.);
#633=B_SPLINE_CURVE_WITH_KNOTS('',3,(#25034,#25035,#25036,#25037,#25038,
#25039,#25040,#25041,#25042,#25043,#25044,#25045,#25046,#25047,#25048,#25049,
#25050,#25051,#25052,#25053,#25054,#25055,#25056,#25057,#25058,#25059,#25060,
#25061,#25062,#25063,#25064,#25065,#25066,#25067,#25068,#25069,#25070,#25071,
#25072,#25073,#25074,#25075,#25076,#25077,#25078,#25079),.UNSPECIFIED.,
 .F.,.F.,(4,3,3,3,3,3,3,3,3,3,3,3,3,3,3,4),(0.,7.40646428061214E-5,0.000146779369918774,
0.000164860955696857,0.000232495741978612,0.000300130528260368,0.000322950277848782,
0.000361000159968374,0.000375163160325465,0.000412679476358013,0.000450195792390562,
0.000468403009741517,0.000509319401675059,0.000549287864653555,0.000588177998696803,
0.000600261056520756),.UNSPECIFIED.);
#634=B_SPLINE_CURVE_WITH_KNOTS('',3,(#25094,#25095,#25096,#25097,#25098,
#25099,#25100,#25101,#25102,#25103,#25104,#25105,#25106,#25107,#25108,#25109,
#25110,#25111,#25112,#25113,#25114,#25115,#25116,#25117,#25118,#25119,#25120,
#25121,#25122,#25123,#25124,#25125,#25126,#25127,#25128,#25129,#25130,#25131,
#25132,#25133,#25134,#25135,#25136,#25137,#25138,#25139,#25140,#25141,#25142,
#25143,#25144,#25145,#25146,#25147,#25148,#25149,#25150,#25151,#25152,#25153,
#25154),.UNSPECIFIED.,.F.,.F.,(4,3,3,3,3,3,3,3,3,3,3,3,3,3,3,3,3,3,3,3,
4),(0.,3.01683521755624E-5,5.95123638943077E-5,8.83024180022877E-5,0.00011676839189743,
0.00012067340870225,0.000156899735255077,0.000194095346003556,0.000232946053825429,
0.000241346817404499,0.00028483712090787,0.000330243027192198,0.000378792539153568,
0.000430743086981298,0.000482693634809027,0.000560072810733523,0.000642027313860096,
0.00073189117824408,0.000825743849904349,0.000923569286423716,0.000965387269618084),
 .UNSPECIFIED.);
#635=B_SPLINE_CURVE_WITH_KNOTS('',3,(#25274,#25275,#25276,#25277,#25278,
#25279,#25280,#25281,#25282,#25283,#25284,#25285,#25286,#25287,#25288,#25289,
#25290,#25291,#25292,#25293,#25294,#25295,#25296,#25297,#25298,#25299,#25300,
#25301,#25302,#25303,#25304,#25305,#25306,#25307,#25308,#25309,#25310),
 .UNSPECIFIED.,.F.,.F.,(4,3,3,3,3,3,3,3,3,3,3,3,4),(0.,6.99403169130158E-5,
0.00013663881220017,0.00019323995121994,0.000204958218300255,0.000257951721023207,
0.00027327762440034,0.000285453692681066,0.000346137712528328,0.000408654588979332,
0.000472636894880584,0.000539340363922078,0.000546555248800679),
 .UNSPECIFIED.);
#636=B_SPLINE_CURVE_WITH_KNOTS('',3,(#25387,#25388,#25389,#25390,#25391,
#25392,#25393,#25394,#25395,#25396,#25397,#25398,#25399,#25400,#25401,#25402,
#25403,#25404,#25405,#25406,#25407,#25408,#25409,#25410,#25411,#25412,#25413,
#25414,#25415,#25416,#25417,#25418,#25419,#25420,#25421,#25422,#25423,#25424,
#25425,#25426,#25427,#25428,#25429,#25430,#25431,#25432,#25433,#25434,#25435,
#25436,#25437,#25438,#25439,#25440,#25441,#25442,#25443,#25444,#25445,#25446,
#25447,#25448,#25449,#25450,#25451,#25452,#25453,#25454,#25455,#25456,#25457,
#25458,#25459,#25460,#25461,#25462),.UNSPECIFIED.,.F.,.F.,(4,3,3,3,3,3,
3,3,3,3,3,3,3,3,3,3,3,3,3,3,3,3,3,3,3,4),(1.90409143160226E-17,1.95383290192995E-5,
4.88458225482488E-5,6.34995693127234E-5,6.71630060038421E-5,7.26581610405201E-5,
7.8153316077198E-5,0.000107954788056933,0.000117229974115797,0.000122114556370622,
0.00012431938532005,0.000126388565843594,0.000156306632154396,0.000183190273141605,
0.000195383290192993,0.000210037036957467,0.000222859065376382,0.000260630252152406,
0.000268336943281981,0.000312613264308786,0.000345493122480558,0.000400681529065493,
0.000461636530392023,0.000526902227878309,0.000600651717012678,0.000625226164026665),
 .UNSPECIFIED.);
#637=B_SPLINE_CURVE_WITH_KNOTS('',3,(#25476,#25477,#25478,#25479,#25480,
#25481,#25482,#25483,#25484,#25485,#25486,#25487,#25488,#25489,#25490,#25491,
#25492,#25493,#25494,#25495,#25496,#25497,#25498,#25499,#25500,#25501,#25502,
#25503,#25504,#25505,#25506,#25507,#25508,#25509,#25510,#25511,#25512,#25513,
#25514,#25515,#25516,#25517,#25518,#25519,#25520,#25521,#25522,#25523,#25524,
#25525,#25526,#25527,#25528,#25529,#25530,#25531,#25532,#25533,#25534,#25535,
#25536,#25537,#25538,#25539,#25540,#25541,#25542,#25543,#25544,#25545,#25546,
#25547,#25548,#25549,#25550,#25551),.UNSPECIFIED.,.F.,.F.,(4,3,3,3,3,3,
3,3,3,3,3,3,3,3,3,3,3,3,3,3,3,3,3,3,3,4),(0.,1.95383290192989E-5,4.88458225482473E-5,
6.34995693127215E-5,6.71630060038401E-5,7.26581610405179E-5,7.81533160771957E-5,
0.000107954788054619,0.000117229974115794,0.000122114556370618,0.000124319385320053,
0.00012638856584359,0.000156306632154391,0.000183190273142427,0.000195383290192988,
0.000210037036957462,0.000222859065376376,0.000260630252155243,0.000268336943281989,
0.000312613264308778,0.000345493122395937,0.000400681528975873,0.00046163653029605,
0.00052690222777407,0.000600651716897933,0.000625226163983449),
 .UNSPECIFIED.);
#638=B_SPLINE_CURVE_WITH_KNOTS('',3,(#25586,#25587,#25588,#25589,#25590,
#25591,#25592,#25593,#25594,#25595,#25596,#25597,#25598,#25599,#25600,#25601,
#25602,#25603,#25604,#25605,#25606,#25607,#25608,#25609,#25610,#25611,#25612,
#25613,#25614,#25615,#25616,#25617,#25618,#25619,#25620,#25621,#25622,#25623,
#25624,#25625,#25626,#25627,#25628,#25629,#25630,#25631),.UNSPECIFIED.,
 .F.,.F.,(4,3,3,3,3,3,3,3,3,3,3,3,3,3,3,4),(0.,3.50262368530255E-5,7.11751710414925E-5,
0.000109339082869859,0.000148762751082846,0.000189988996389714,0.000198220556017289,
0.000254911247280624,0.000313675244695655,0.00037559496150714,0.000396441112034577,
0.000477792055759519,0.000566506458105226,0.00065905994774777,0.000755430891867985,
0.000792882224069153),.UNSPECIFIED.);
#639=B_SPLINE_CURVE_WITH_KNOTS('',3,(#25657,#25658,#25659,#25660,#25661,
#25662,#25663,#25664,#25665,#25666,#25667,#25668,#25669,#25670,#25671,#25672,
#25673,#25674,#25675,#25676,#25677,#25678,#25679,#25680,#25681,#25682,#25683,
#25684,#25685,#25686,#25687,#25688,#25689,#25690,#25691,#25692,#25693,#25694,
#25695,#25696,#25697,#25698,#25699,#25700,#25701,#25702,#25703,#25704,#25705,
#25706,#25707,#25708,#25709,#25710,#25711,#25712,#25713,#25714),
 .UNSPECIFIED.,.F.,.F.,(4,3,3,3,3,3,3,3,3,3,3,3,3,3,3,3,3,3,3,4),(0.,8.33528450008425E-5,
0.000157226441485683,0.000225533822544734,0.000289516624149074,0.000348414967225308,
0.000378847230940205,0.000425063895934943,0.000434497171244511,0.000472969202698466,
0.000509314375641268,0.000542883032632685,0.000568270846410303,0.000610359908966047,
0.000640506736108079,0.000662982654145355,0.000689264740462126,0.000715678191795885,
0.000742518573435992,0.000757694461880407),.UNSPECIFIED.);
#640=B_SPLINE_CURVE_WITH_KNOTS('',3,(#25764,#25765,#25766,#25767,#25768,
#25769,#25770,#25771,#25772,#25773,#25774,#25775,#25776,#25777,#25778,#25779,
#25780,#25781,#25782,#25783,#25784,#25785,#25786,#25787,#25788,#25789,#25790,
#25791,#25792,#25793,#25794,#25795,#25796,#25797,#25798,#25799,#25800,#25801,
#25802,#25803,#25804,#25805,#25806,#25807,#25808,#25809,#25810,#25811,#25812,
#25813,#25814,#25815,#25816,#25817,#25818,#25819,#25820,#25821),
 .UNSPECIFIED.,.F.,.F.,(4,3,3,3,3,3,3,3,3,3,3,3,3,3,3,3,3,3,3,4),(0.,8.3352844998188E-5,
0.000157226441483691,0.000225533822540938,0.000289516624143318,0.00034841496721732,
0.0003788472309402,0.000425063895934259,0.000434497171244525,0.000472969202698661,
0.000509314375641677,0.000542883032633348,0.000568270846410307,0.000610359908966059,
0.000640506736109255,0.000662982654145359,0.00068926474046212,0.000715678191795907,
0.000742518573436032,0.000757694461880412),.UNSPECIFIED.);
#641=B_SPLINE_CURVE_WITH_KNOTS('',3,(#25855,#25856,#25857,#25858,#25859,
#25860,#25861,#25862,#25863,#25864,#25865,#25866,#25867,#25868,#25869,#25870,
#25871,#25872,#25873,#25874,#25875,#25876,#25877,#25878,#25879,#25880,#25881,
#25882,#25883,#25884,#25885,#25886,#25887,#25888,#25889,#25890,#25891,#25892,
#25893,#25894,#25895,#25896,#25897,#25898,#25899,#25900),.UNSPECIFIED.,
 .F.,.F.,(4,3,3,3,3,3,3,3,3,3,3,3,3,3,3,4),(0.,7.40646428067027E-5,0.00014677936992103,
0.000164860955696577,0.000232495741978471,0.000300130528260365,0.000322950277848778,
0.000361000159970521,0.000375163160325462,0.00041267947635801,0.000450195792390558,
0.000468403009741581,0.000509319401678437,0.000549287864660548,0.000588177998707373,
0.000600261056520751),.UNSPECIFIED.);
#642=B_SPLINE_CURVE_WITH_KNOTS('',3,(#25935,#25936,#25937,#25938,#25939,
#25940,#25941,#25942,#25943,#25944,#25945,#25946,#25947,#25948,#25949,#25950,
#25951,#25952,#25953,#25954,#25955,#25956,#25957,#25958,#25959,#25960,#25961,
#25962,#25963,#25964,#25965,#25966,#25967,#25968,#25969,#25970,#25971,#25972,
#25973,#25974,#25975,#25976,#25977,#25978,#25979,#25980),.UNSPECIFIED.,
 .F.,.F.,(4,3,3,3,3,3,3,3,3,3,3,3,3,3,3,4),(0.,4.01784152582232E-5,8.11318192707994E-5,
0.000123430231631933,0.00013379748131031,0.000151845918076035,0.000189807397595043,
0.000231866097105714,0.000275906952597149,0.000281134062468639,0.000303691836152069,
0.000372309715976617,0.000440927595801166,0.000514103167127634,0.000588539200903764,
0.000607383672304138),.UNSPECIFIED.);
#643=B_SPLINE_CURVE_WITH_KNOTS('',3,(#26033,#26034,#26035,#26036,#26037,
#26038,#26039,#26040,#26041,#26042,#26043,#26044,#26045,#26046,#26047,#26048,
#26049,#26050,#26051,#26052,#26053,#26054,#26055,#26056,#26057),
 .UNSPECIFIED.,.F.,.F.,(4,3,3,3,3,3,3,3,4),(0.,8.78783823229168E-5,0.000181106371765768,
0.000284958381202673,0.000400167490967761,0.000487646104112346,0.000496588354691666,
0.000792223039523606,0.000993167107609097),.UNSPECIFIED.);
#644=B_SPLINE_CURVE_WITH_KNOTS('',3,(#26088,#26089,#26090,#26091,#26092,
#26093,#26094,#26095,#26096,#26097,#26098,#26099,#26100,#26101,#26102,#26103,
#26104,#26105,#26106,#26107,#26108,#26109,#26110,#26111,#26112),
 .UNSPECIFIED.,.F.,.F.,(4,3,3,3,3,3,3,3,4),(9.46798652745075E-9,0.000265027615065046,
0.000494820327888722,0.00050511495778071,0.000628257448094622,0.000739957890426431,
0.000844064037925376,0.000940011289231895,0.000989640655777444),
 .UNSPECIFIED.);
#645=B_SPLINE_CURVE_WITH_KNOTS('',3,(#26113,#26114,#26115,#26116,#26117,
#26118),.UNSPECIFIED.,.F.,.F.,(4,2,4),(7.44334043044855E-6,0.5,1.),
 .UNSPECIFIED.);
#646=B_SPLINE_CURVE_WITH_KNOTS('',3,(#26251,#26252,#26253,#26254,#26255,
#26256,#26257,#26258,#26259,#26260,#26261,#26262,#26263,#26264,#26265,#26266,
#26267,#26268,#26269,#26270,#26271,#26272,#26273,#26274,#26275,#26276,#26277,
#26278,#26279,#26280,#26281,#26282,#26283,#26284,#26285,#26286,#26287,#26288,
#26289,#26290,#26291,#26292,#26293,#26294,#26295,#26296,#26297,#26298,#26299,
#26300,#26301,#26302,#26303,#26304,#26305),.UNSPECIFIED.,.F.,.F.,(4,3,3,
3,3,3,3,3,3,3,3,3,3,3,3,3,3,3,4),(1.00003366271743E-7,0.000627368764008543,
0.00125605094111647,0.00251210188223294,0.00502420376446587,0.0136336598992699,
0.0252314310431504,0.0410681024056911,0.0681502020062923,0.113858415357405,
0.184994129390117,0.291968963770629,0.346051748925135,0.51971092269832,
0.668061140433059,0.82760635706631,0.964639961031585,0.987151573699562,
1.),.UNSPECIFIED.);
#647=B_SPLINE_CURVE_WITH_KNOTS('',3,(#26339,#26340,#26341,#26342,#26343,
#26344,#26345,#26346,#26347,#26348,#26349,#26350,#26351,#26352,#26353,#26354,
#26355,#26356,#26357,#26358,#26359,#26360,#26361,#26362,#26363,#26364,#26365,
#26366,#26367,#26368,#26369,#26370,#26371,#26372,#26373,#26374,#26375,#26376,
#26377,#26378,#26379,#26380,#26381,#26382,#26383,#26384),.UNSPECIFIED.,
 .F.,.F.,(4,3,3,3,3,3,3,3,3,3,3,3,3,3,3,4),(0.,9.7296808173656E-5,0.000188076340040901,
0.000274624933129628,0.000355070980212206,0.000389187232694624,0.000449617363166583,
0.000507814172800233,0.000562918686626053,0.000583780849041926,0.000624250891657903,
0.000662781785090734,0.000699618916497541,0.000735289518509887,0.000769568105189037,
0.000778374465389229),.UNSPECIFIED.);
#648=B_SPLINE_CURVE_WITH_KNOTS('',3,(#26388,#26389,#26390,#26391,#26392,
#26393,#26394,#26395,#26396,#26397,#26398,#26399,#26400,#26401,#26402,#26403,
#26404,#26405,#26406,#26407,#26408,#26409,#26410,#26411,#26412,#26413,#26414,
#26415,#26416,#26417,#26418,#26419,#26420,#26421),.UNSPECIFIED.,.F.,.F.,
(4,3,3,3,3,3,3,3,3,3,3,4),(0.,6.47846574208782E-5,0.000128085038048596,
0.000193342800024759,0.000254275817470981,0.000258600562000923,0.000269706482902613,
0.000323662397375826,0.000382521450093377,0.000443803383538095,0.00050542857129258,
0.000539412965805225),.UNSPECIFIED.);
#649=B_SPLINE_CURVE_WITH_KNOTS('',3,(#26425,#26426,#26427,#26428,#26429,
#26430,#26431,#26432,#26433,#26434,#26435,#26436,#26437,#26438,#26439,#26440,
#26441,#26442,#26443,#26444,#26445,#26446,#26447,#26448,#26449,#26450,#26451,
#26452,#26453,#26454,#26455,#26456,#26457,#26458,#26459,#26460,#26461,#26462,
#26463,#26464,#26465,#26466,#26467,#26468,#26469,#26470),.UNSPECIFIED.,
 .F.,.F.,(4,3,3,3,3,3,3,3,3,3,3,3,3,3,3,4),(0.,7.33096139802609E-5,0.00014538886142587,
0.000163772356053824,0.000231283930773087,0.00029879550549235,0.00032102040376583,
0.000359079183382255,0.000373494381865439,0.000410843820051984,0.000448193258238528,
0.000465950705574258,0.000507344602018312,0.000547782593938721,0.00058711828767304,
0.000597591010984707),.UNSPECIFIED.);
#650=B_SPLINE_CURVE_WITH_KNOTS('',3,(#26478,#26479,#26480,#26481,#26482,
#26483,#26484,#26485,#26486,#26487,#26488,#26489,#26490,#26491,#26492,#26493,
#26494,#26495,#26496,#26497,#26498,#26499,#26500,#26501,#26502,#26503,#26504,
#26505,#26506,#26507,#26508,#26509,#26510,#26511),.UNSPECIFIED.,.F.,.F.,
(4,3,3,3,3,3,3,3,3,3,3,4),(0.,6.47846574211507E-5,0.000128085038050523,
0.000193342800025718,0.000254275817473748,0.000258600562000914,0.000269706482902609,
0.000323662397372321,0.000382521450086426,0.000443803383527674,0.00050542857127833,
0.000539412965805219),.UNSPECIFIED.);
#651=B_SPLINE_CURVE_WITH_KNOTS('',3,(#26527,#26528,#26529,#26530,#26531,
#26532,#26533,#26534,#26535,#26536,#26537,#26538),.UNSPECIFIED.,.F.,.F.,
(4,2,2,2,2,4),(9.94226663611176E-9,0.00032517293922485,0.0006503458784497,
0.00097551881767455,0.00113810528728698,0.0013006917568994),
 .UNSPECIFIED.);
#652=B_SPLINE_CURVE_WITH_KNOTS('',3,(#26686,#26687,#26688,#26689,#26690,
#26691,#26692,#26693,#26694,#26695,#26696,#26697,#26698,#26699,#26700,#26701,
#26702,#26703,#26704,#26705,#26706,#26707,#26708,#26709,#26710,#26711,#26712,
#26713,#26714,#26715,#26716,#26717,#26718,#26719,#26720,#26721,#26722,#26723,
#26724,#26725,#26726,#26727,#26728,#26729,#26730,#26731,#26732,#26733,#26734,
#26735,#26736,#26737),.UNSPECIFIED.,.F.,.F.,(4,3,3,3,3,3,3,3,3,3,3,3,3,
3,3,3,3,4),(0.,4.12764459949069E-5,8.42546564927975E-5,0.000129571564839558,
0.000139714696155275,0.000197401075511389,0.000258094770764511,0.000279429392310549,
0.000359695196555218,0.00044273022393022,0.000529248927812781,0.000558858784621119,
0.000667945714892313,0.000780388678479799,0.000891339019476329,0.00100452829435929,
0.00110832362887638,0.00111771756924225),.UNSPECIFIED.);
#653=B_SPLINE_CURVE_WITH_KNOTS('',3,(#26769,#26770,#26771,#26772,#26773,
#26774,#26775,#26776,#26777,#26778,#26779,#26780,#26781,#26782,#26783,#26784,
#26785,#26786,#26787,#26788,#26789,#26790,#26791,#26792,#26793,#26794,#26795,
#26796,#26797,#26798,#26799,#26800,#26801,#26802,#26803,#26804,#26805,#26806,
#26807,#26808,#26809,#26810,#26811,#26812,#26813,#26814,#26815,#26816,#26817,
#26818,#26819,#26820,#26821,#26822,#26823,#26824,#26825,#26826,#26827,#26828,
#26829,#26830,#26831,#26832),.UNSPECIFIED.,.F.,.F.,(4,3,3,3,3,3,3,3,3,3,
3,3,3,3,3,3,3,3,3,3,3,4),(0.,9.68515416480563E-5,0.000192020529402926,0.000279284320016308,
0.000361898476753293,0.000438321326769534,0.000477527492667534,0.00052960775931866,
0.000578407666765381,0.000625243185950011,0.00067076721247565,0.000713433961487206,
0.000716291239001288,0.000754462993922578,0.000791422812843817,0.000826961927144892,
0.000835673112168161,0.000863826223827739,0.000892456091106298,0.000921613281238493,
0.000951948647272746,0.000955054985335033),.UNSPECIFIED.);
#654=B_SPLINE_CURVE_WITH_KNOTS('',3,(#26841,#26842,#26843,#26844,#26845,
#26846,#26847,#26848,#26849,#26850,#26851,#26852,#26853,#26854,#26855,#26856,
#26857,#26858,#26859,#26860,#26861,#26862,#26863,#26864,#26865,#26866,#26867,
#26868,#26869,#26870,#26871),.UNSPECIFIED.,.F.,.F.,(4,3,3,3,3,3,3,3,3,3,
4),(0.,4.98163029433582E-5,0.000100000315597884,0.000150867282275571,0.000202142388486024,
0.000254132046646703,0.000271251473618865,0.000333586404663745,0.000403372432315032,
0.000481003240191196,0.00054250294723773),.UNSPECIFIED.);
#655=B_SPLINE_CURVE_WITH_KNOTS('',3,(#26911,#26912,#26913,#26914,#26915,
#26916,#26917,#26918,#26919,#26920,#26921,#26922,#26923,#26924,#26925,#26926,
#26927,#26928,#26929,#26930,#26931,#26932,#26933,#26934,#26935,#26936,#26937,
#26938,#26939,#26940,#26941,#26942,#26943,#26944,#26945,#26946,#26947),
 .UNSPECIFIED.,.F.,.F.,(4,3,3,3,3,3,3,3,3,3,3,3,4),(0.,6.99403168951901E-5,
0.000136638812200168,0.00019323995121385,0.000204958218300252,0.000257951721019661,
0.000273277624400336,0.00028545369268105,0.000346137712527676,0.00040865458897473,
0.00047263689487051,0.000539340363905251,0.000546555248800672),
 .UNSPECIFIED.);
#656=B_SPLINE_CURVE_WITH_KNOTS('',3,(#27013,#27014,#27015,#27016,#27017,
#27018,#27019,#27020,#27021,#27022,#27023,#27024,#27025,#27026,#27027,#27028,
#27029,#27030,#27031,#27032,#27033,#27034,#27035,#27036,#27037,#27038,#27039,
#27040,#27041,#27042,#27043,#27044,#27045,#27046,#27047,#27048,#27049,#27050,
#27051,#27052,#27053,#27054,#27055,#27056,#27057,#27058),.UNSPECIFIED.,
 .F.,.F.,(4,3,3,3,3,3,3,3,3,3,3,3,3,3,3,4),(0.,3.97160926935229E-5,8.01799642593007E-5,
0.000121988391402582,0.000134049545972337,0.000152559369824133,0.000190699212280166,
0.000233020073010242,0.000277317564290133,0.000281953897382099,0.000305118739648266,
0.000373877625544705,0.000442636511441145,0.000516471370795696,0.000591684329573585,
0.000610237479296514),.UNSPECIFIED.);
#657=B_SPLINE_CURVE_WITH_KNOTS('',3,(#27060,#27061,#27062,#27063,#27064,
#27065,#27066,#27067,#27068,#27069,#27070,#27071,#27072,#27073,#27074,#27075,
#27076,#27077,#27078,#27079,#27080,#27081,#27082,#27083,#27084,#27085,#27086,
#27087,#27088,#27089,#27090,#27091,#27092,#27093,#27094,#27095,#27096,#27097,
#27098,#27099,#27100,#27101,#27102,#27103,#27104,#27105),.UNSPECIFIED.,
 .F.,.F.,(4,3,3,3,3,3,3,3,3,3,3,3,3,3,3,4),(0.,7.40646428074384E-5,0.000146779369922617,
0.000164860955696866,0.000232495741978627,0.000300130528260388,0.000322950277848808,
0.000361000159970105,0.000375163160325479,0.000412679476358025,0.000450195792390571,
0.000468403009741553,0.000509319401678602,0.000549287864660367,0.000588177998706901,
0.000600261056520754),.UNSPECIFIED.);
#658=B_SPLINE_CURVE_WITH_KNOTS('',3,(#27140,#27141,#27142,#27143,#27144,
#27145,#27146,#27147,#27148,#27149,#27150,#27151,#27152,#27153,#27154,#27155,
#27156,#27157,#27158,#27159,#27160,#27161,#27162,#27163,#27164,#27165,#27166,
#27167,#27168,#27169,#27170,#27171,#27172,#27173,#27174,#27175,#27176,#27177,
#27178,#27179,#27180,#27181,#27182,#27183,#27184,#27185),.UNSPECIFIED.,
 .F.,.F.,(4,3,3,3,3,3,3,3,3,3,3,3,3,3,3,4),(0.,4.01784152590413E-5,8.11318192717161E-5,
0.00012343023163194,0.000133797481310322,0.000151845918076025,0.000189807397595031,
0.000231866097106636,0.000275906952598724,0.000281134062468662,0.000303691836152049,
0.000372309715976737,0.000440927595801426,0.000514103167120356,0.000588539200891124,
0.000607383672304106),.UNSPECIFIED.);
#659=B_SPLINE_CURVE_WITH_KNOTS('',3,(#27193,#27194,#27195,#27196,#27197,
#27198,#27199,#27200,#27201,#27202,#27203,#27204,#27205,#27206,#27207,#27208,
#27209,#27210,#27211,#27212,#27213,#27214,#27215,#27216,#27217,#27218,#27219,
#27220,#27221,#27222,#27223,#27224,#27225,#27226,#27227,#27228,#27229,#27230,
#27231,#27232,#27233,#27234,#27235,#27236,#27237,#27238,#27239,#27240,#27241,
#27242,#27243,#27244),.UNSPECIFIED.,.F.,.F.,(4,3,3,3,3,3,3,3,3,3,3,3,3,
3,3,3,3,4),(0.,0.000104093954358116,0.000217335668171905,0.000328639449066821,
0.000442850129340045,0.000551144481414275,0.00055706080961327,0.0006429177227539,
0.000726322659738398,0.00080560830646621,0.000835591214419904,0.000896354287923508,
0.000954074031547537,0.000974856416823221,0.00101967443613433,0.00106279159941887,
0.00110343944760186,0.00111412161922654),.UNSPECIFIED.);
#660=B_SPLINE_CURVE_WITH_KNOTS('',3,(#27294,#27295,#27296,#27297,#27298,
#27299,#27300,#27301,#27302,#27303,#27304,#27305,#27306,#27307,#27308,#27309,
#27310,#27311,#27312,#27313,#27314,#27315,#27316,#27317,#27318,#27319,#27320,
#27321,#27322,#27323,#27324,#27325,#27326,#27327,#27328,#27329,#27330,#27331,
#27332,#27333,#27334,#27335,#27336,#27337,#27338,#27339,#27340,#27341,#27342,
#27343,#27344,#27345,#27346,#27347,#27348,#27349,#27350,#27351,#27352,#27353,
#27354),.UNSPECIFIED.,.F.,.F.,(4,3,3,3,3,3,3,3,3,3,3,3,3,3,3,3,3,3,3,3,
4),(0.,3.01683521755654E-5,5.95123638939948E-5,8.83024180015813E-5,0.000116768391896489,
0.000120673408702262,0.000156899735254867,0.000194095346003115,0.000232946053824629,
0.000241346817404523,0.000284837120908685,0.000330243027193698,0.000378792539155905,
0.000430743086982471,0.000482693634809037,0.00056007281073296,0.000642027313858774,
0.000731891178241761,0.00082574384990152,0.000923569286420814,0.000965387269618077),
 .UNSPECIFIED.);
#661=B_SPLINE_CURVE_WITH_KNOTS('',3,(#27385,#27386,#27387,#27388,#27389,
#27390,#27391,#27392,#27393,#27394,#27395,#27396,#27397,#27398,#27399,#27400,
#27401,#27402,#27403,#27404,#27405,#27406,#27407,#27408,#27409,#27410,#27411,
#27412,#27413,#27414,#27415,#27416,#27417,#27418,#27419,#27420,#27421,#27422,
#27423,#27424,#27425,#27426,#27427,#27428,#27429,#27430),.UNSPECIFIED.,
 .F.,.F.,(4,3,3,3,3,3,3,3,3,3,3,3,3,3,3,4),(0.,7.33096139968579E-5,0.000145388861463487,
0.000163772356054208,0.000231283930773278,0.000298795505492349,0.000321020403765824,
0.000359079183383553,0.000373494381865434,0.000410843820051977,0.00044819325823852,
0.000465950705574249,0.000507344602017609,0.000547782593937178,0.000587118287670288,
0.000597591010984692),.UNSPECIFIED.);
#662=B_SPLINE_CURVE_WITH_KNOTS('',3,(#27478,#27479,#27480,#27481,#27482,
#27483,#27484,#27485,#27486,#27487,#27488,#27489),.UNSPECIFIED.,.F.,.F.,
(4,2,2,2,2,4),(9.9422622804038E-9,0.000325172939224853,0.000650345878449707,
0.00097551881767456,0.00113810528728698,0.00130069175689939),
 .UNSPECIFIED.);
#663=B_SPLINE_CURVE_WITH_KNOTS('',3,(#27544,#27545,#27546,#27547,#27548,
#27549,#27550,#27551,#27552,#27553,#27554,#27555,#27556,#27557,#27558,#27559,
#27560,#27561,#27562,#27563,#27564,#27565,#27566,#27567,#27568),
 .UNSPECIFIED.,.F.,.F.,(4,3,3,3,3,3,3,3,4),(0.,9.58519120559013E-5,0.000201048393009301,
0.000313533962690425,0.000443358794838372,0.000487856029895822,0.000498221418747226,
0.000765061137597183,0.000996433304431859),.UNSPECIFIED.);
#664=B_SPLINE_CURVE_WITH_KNOTS('',3,(#27603,#27604,#27605,#27606,#27607,
#27608,#27609,#27610,#27611,#27612,#27613,#27614,#27615,#27616,#27617,#27618,
#27619,#27620,#27621,#27622,#27623,#27624,#27625,#27626,#27627,#27628,#27629,
#27630,#27631,#27632,#27633),.UNSPECIFIED.,.F.,.F.,(4,3,3,3,3,3,3,3,3,3,
4),(0.,4.98163029433653E-5,0.000100000315597862,0.000150867282275564,0.000202142388486088,
0.000254132046646779,0.000271251473618865,0.000333586404663683,0.000403372432314982,
0.000481003240191066,0.00054250294723773),.UNSPECIFIED.);
#665=B_SPLINE_CURVE_WITH_KNOTS('',3,(#27668,#27669,#27670,#27671,#27672,
#27673,#27674,#27675,#27676,#27677,#27678,#27679,#27680,#27681,#27682,#27683,
#27684,#27685,#27686,#27687,#27688,#27689,#27690,#27691,#27692),
 .UNSPECIFIED.,.F.,.F.,(4,3,3,3,3,3,3,3,4),(0.,8.83378490479586E-5,0.000182066239385022,
0.000286502548781802,0.000402561956922467,0.000487834363092893,0.000496699977573566,
0.000791146466104245,0.000993390351418002),.UNSPECIFIED.);
#666=B_SPLINE_CURVE_WITH_KNOTS('',3,(#27837,#27838,#27839,#27840,#27841,
#27842,#27843,#27844,#27845,#27846,#27847,#27848,#27849,#27850,#27851,#27852,
#27853,#27854,#27855,#27856,#27857,#27858,#27859,#27860,#27861,#27862,#27863,
#27864,#27865,#27866,#27867,#27868,#27869,#27870),.UNSPECIFIED.,.F.,.F.,
(4,3,3,3,3,3,3,3,3,3,3,4),(0.,6.47846574223387E-5,0.000128085038052483,
0.000193342800026691,0.000254275817474483,0.000258600562000898,0.000269706482902605,
0.000323662397373896,0.000382521450089233,0.000443803383531375,0.000505428571282867,
0.00053941296580521),.UNSPECIFIED.);
#667=B_SPLINE_CURVE_WITH_KNOTS('',3,(#27909,#27910,#27911,#27912,#27913,
#27914,#27915,#27916,#27917,#27918,#27919,#27920,#27921,#27922,#27923,#27924,
#27925,#27926,#27927,#27928,#27929,#27930,#27931,#27932,#27933,#27934,#27935,
#27936,#27937,#27938,#27939,#27940,#27941,#27942,#27943,#27944,#27945,#27946,
#27947,#27948,#27949,#27950,#27951,#27952,#27953,#27954),.UNSPECIFIED.,
 .F.,.F.,(4,3,3,3,3,3,3,3,3,3,3,3,3,3,3,4),(0.,3.50262368532445E-5,7.11751710419857E-5,
0.000109339082870391,0.000148762751083315,0.000189988996390031,0.000198220556017292,
0.000254911247279634,0.000313675244693709,0.000375594961504314,0.000396441112034585,
0.000477792055753319,0.000566506458090588,0.000659059947720601,0.000755430891818796,
0.000792882224069168),.UNSPECIFIED.);
#668=B_SPLINE_CURVE_WITH_KNOTS('',3,(#27979,#27980,#27981,#27982,#27983,
#27984,#27985,#27986,#27987,#27988,#27989,#27990,#27991,#27992,#27993,#27994,
#27995,#27996,#27997,#27998,#27999,#28000,#28001,#28002,#28003,#28004,#28005,
#28006,#28007,#28008,#28009,#28010,#28011,#28012,#28013,#28014,#28015,#28016,
#28017,#28018,#28019,#28020,#28021,#28022,#28023,#28024,#28025,#28026,#28027,
#28028,#28029,#28030,#28031,#28032,#28033,#28034,#28035,#28036,#28037,#28038,
#28039,#28040,#28041,#28042,#28043,#28044,#28045,#28046,#28047,#28048,#28049,
#28050,#28051,#28052,#28053,#28054,#28055,#28056,#28057,#28058,#28059,#28060,
#28061,#28062,#28063),.UNSPECIFIED.,.F.,.F.,(4,3,3,3,3,3,3,3,3,3,3,3,3,
3,3,3,3,3,3,3,3,3,3,3,3,3,3,3,4),(3.63939196670295E-10,7.80137041101504E-5,
0.000136523982192763,0.000158465336473743,0.000196862706465458,0.00025445876145303,
0.000283256788946816,0.000297655802693709,0.000312054816440602,0.000356230898886013,
0.000390068520550753,0.000399820233564522,0.000408352982451569,0.000438217603556236,
0.000464692044654508,0.000468082224660904,0.000487585650688441,0.000494899435448768,
0.00049809921628141,0.00050001235016164,0.000504098805342616,0.000534061837383381,
0.000546095928771053,0.000550971785277938,0.000555542900753142,0.000586967153584001,
0.000589826266817172,0.00061930792844511,0.000624109632881203),
 .UNSPECIFIED.);
#669=B_SPLINE_CURVE_WITH_KNOTS('',3,(#28095,#28096,#28097,#28098,#28099,
#28100,#28101,#28102,#28103,#28104,#28105,#28106,#28107,#28108,#28109,#28110,
#28111,#28112,#28113,#28114,#28115,#28116,#28117,#28118,#28119,#28120,#28121,
#28122,#28123,#28124,#28125,#28126,#28127,#28128,#28129,#28130,#28131,#28132,
#28133,#28134,#28135,#28136,#28137,#28138,#28139,#28140,#28141,#28142,#28143,
#28144,#28145,#28146,#28147,#28148,#28149,#28150,#28151,#28152,#28153,#28154,
#28155,#28156,#28157,#28158,#28159,#28160,#28161,#28162,#28163,#28164,#28165,
#28166,#28167,#28168,#28169,#28170,#28171,#28172,#28173,#28174,#28175,#28176,
#28177,#28178,#28179,#28180,#28181,#28182),.UNSPECIFIED.,.F.,.F.,(4,3,3,
3,3,3,3,3,3,3,3,3,3,3,3,3,3,3,3,3,3,3,3,3,3,3,3,3,3,4),(0.,2.50679729420699E-5,
3.13295796930182E-5,4.72260971999786E-5,7.10708734604193E-5,8.29932615906396E-5,
8.89544556557498E-5,9.04447541720273E-5,9.49156497208599E-5,0.000121982835340966,
0.00014237347458129,0.000145339588635067,0.000147646510203545,0.0001803434454297,
0.00018983129944172,0.000220219538030718,0.000237289124302146,0.000255085808624806,
0.000262871858015969,0.000270171279320185,0.000314583791963415,0.000324174511012843,
0.000376787272343466,0.000379662598883424,0.000415768922432964,0.000477328763328744,
0.000543052315574684,0.000616743070253868,0.000699630235102015,0.000759325197766855),
 .UNSPECIFIED.);
#670=B_SPLINE_CURVE_WITH_KNOTS('',3,(#28222,#28223,#28224,#28225,#28226,
#28227,#28228,#28229,#28230,#28231,#28232,#28233,#28234),.UNSPECIFIED.,
 .F.,.F.,(4,3,3,3,4),(0.,0.00112869544108361,0.00112886842160677,0.0017855132108252,
0.00225773684321331),.UNSPECIFIED.);
#671=B_SPLINE_CURVE_WITH_KNOTS('',3,(#28282,#28283,#28284,#28285,#28286,
#28287,#28288,#28289,#28290,#28291,#28292,#28293,#28294,#28295,#28296,#28297),
 .UNSPECIFIED.,.F.,.F.,(4,3,3,3,3,4),(1.73472347597681E-18,0.000789165583599754,
0.00112882209307301,0.00112972782036785,0.00186613475216116,0.00225764418614602),
 .UNSPECIFIED.);
#672=B_SPLINE_CURVE_WITH_KNOTS('',3,(#28361,#28362,#28363,#28364,#28365,
#28366,#28367,#28368,#28369,#28370,#28371,#28372,#28373,#28374,#28375,#28376,
#28377,#28378,#28379,#28380,#28381,#28382),.UNSPECIFIED.,.F.,.F.,(4,3,3,
3,3,3,3,4),(0.,0.000187383859258548,0.000390718319973205,0.000506671891006544,
0.000510839709360771,0.000711636939114786,0.00091215180264492,0.00102167941872154),
 .UNSPECIFIED.);
#673=B_SPLINE_CURVE_WITH_KNOTS('',3,(#28403,#28404,#28405,#28406,#28407,
#28408,#28409,#28410,#28411,#28412,#28413,#28414,#28415,#28416,#28417,#28418),
 .UNSPECIFIED.,.F.,.F.,(4,3,3,3,3,4),(3.46944695195361E-18,0.000789165584742738,
0.00112882209307305,0.00112972782036789,0.0018661347548332,0.0022576441861461),
 .UNSPECIFIED.);
#674=B_SPLINE_CURVE_WITH_KNOTS('',3,(#28530,#28531,#28532,#28533,#28534,
#28535,#28536,#28537,#28538,#28539,#28540,#28541,#28542,#28543,#28544,#28545,
#28546,#28547,#28548),.UNSPECIFIED.,.F.,.F.,(4,3,3,3,3,3,4),(0.,0.000411399963284772,
0.000510753962571242,0.000514787301367235,0.000703786539778562,0.000866757158960636,
0.00102150792514248),.UNSPECIFIED.);
#675=B_SPLINE_CURVE_WITH_KNOTS('',3,(#28553,#28554,#28555,#28556,#28557,
#28558,#28559,#28560,#28561,#28562,#28563,#28564,#28565),.UNSPECIFIED.,
 .F.,.F.,(4,3,3,3,4),(0.,0.00112869544108359,0.00112886842160676,0.00178551321104577,
0.00225773684321329),.UNSPECIFIED.);
#676=B_SPLINE_CURVE_WITH_KNOTS('',3,(#28675,#28676,#28677,#28678,#28679,
#28680,#28681,#28682,#28683,#28684,#28685,#28686,#28687),.UNSPECIFIED.,
 .F.,.F.,(4,3,3,3,4),(2.36524922520259E-16,0.000656666445676668,0.00112890565164586,
0.00112907863787392,0.00225781130329172),.UNSPECIFIED.);
#677=B_SPLINE_CURVE_WITH_KNOTS('',3,(#28694,#28695,#28696,#28697,#28698,
#28699,#28700,#28701,#28702,#28703,#28704,#28705,#28706,#28707,#28708,#28709,
#28710,#28711,#28712),.UNSPECIFIED.,.F.,.F.,(4,3,3,3,3,3,4),(0.,0.000411399964056932,
0.00051075396257123,0.000514787301367217,0.000703786539700468,0.000866757158900925,
0.00102150792514246),.UNSPECIFIED.);
#678=B_SPLINE_CURVE_WITH_KNOTS('',3,(#28795,#28796,#28797,#28798,#28799,
#28800,#28801,#28802,#28803,#28804,#28805,#28806,#28807,#28808,#28809,#28810),
 .UNSPECIFIED.,.F.,.F.,(4,3,3,3,3,4),(0.,0.000736491667076813,0.00112804614732749,
0.00112895197883811,0.00191820836757618,0.00225790395767623),
 .UNSPECIFIED.);
#679=B_SPLINE_CURVE_WITH_KNOTS('',3,(#28876,#28877,#28878,#28879,#28880,
#28881,#28882,#28883,#28884,#28885,#28886,#28887,#28888,#28889,#28890,#28891,
#28892,#28893,#28894,#28895,#28896,#28897),.UNSPECIFIED.,.F.,.F.,(4,3,3,
3,3,3,3,4),(0.,0.000187383859222642,0.000390718319947459,0.000506671891006534,
0.000510839709360756,0.000711636939101215,0.000912151802618219,0.00102167941872151),
 .UNSPECIFIED.);
#680=B_SPLINE_CURVE_WITH_KNOTS('',3,(#28939,#28940,#28941,#28942,#28943,
#28944,#28945,#28946,#28947,#28948,#28949,#28950,#28951,#28952,#28953,#28954,
#28955,#28956,#28957,#28958,#28959,#28960),.UNSPECIFIED.,.F.,.F.,(4,3,3,
3,3,3,3,4),(0.,0.000187383859212357,0.000390718320022676,0.000506671891006541,
0.000510839709360768,0.000711636939116541,0.000912151802649271,0.00102167941872154),
 .UNSPECIFIED.);
#681=B_SPLINE_CURVE_WITH_KNOTS('',3,(#29027,#29028,#29029,#29030,#29031,
#29032,#29033,#29034,#29035,#29036,#29037,#29038,#29039,#29040,#29041,#29042),
 .UNSPECIFIED.,.F.,.F.,(4,3,3,3,3,4),(0.,0.000736491665055099,0.00112804614732747,
0.00112895197883809,0.00191820836627224,0.00225790395767619),
 .UNSPECIFIED.);
#682=B_SPLINE_CURVE_WITH_KNOTS('',3,(#29167,#29168,#29169,#29170,#29171,
#29172,#29173,#29174,#29175,#29176,#29177,#29178,#29179,#29180,#29181,#29182,
#29183,#29184,#29185),.UNSPECIFIED.,.F.,.F.,(4,3,3,3,3,3,4),(0.,0.000160829789774429,
0.000333619132037895,0.000508566612075994,0.00051261464436556,0.000925513337291967,
0.00102522928873112),.UNSPECIFIED.);
#683=B_SPLINE_CURVE_WITH_KNOTS('',3,(#29206,#29207,#29208,#29209,#29210,
#29211,#29212,#29213,#29214,#29215,#29216,#29217,#29218),.UNSPECIFIED.,
 .F.,.F.,(4,3,3,3,4),(2.37963132368939E-16,0.000656666445458113,0.00112890565164585,
0.00112907863787391,0.00225781130329169),.UNSPECIFIED.);
#684=B_SPLINE_CURVE_WITH_KNOTS('',3,(#29251,#29252,#29253,#29254,#29255,
#29256,#29257,#29258,#29259,#29260,#29261,#29262,#29263,#29264,#29265,#29266,
#29267,#29268,#29269),.UNSPECIFIED.,.F.,.F.,(4,3,3,3,3,3,4),(0.,0.000411399963336404,
0.000510753962571242,0.000514787301367239,0.000703786539777697,0.000866757158959836,
0.00102150792514248),.UNSPECIFIED.);
#685=B_SPLINE_CURVE_WITH_KNOTS('',3,(#29394,#29395,#29396,#29397,#29398,
#29399,#29400,#29401,#29402,#29403,#29404,#29405,#29406,#29407,#29408,#29409,
#29410,#29411,#29412,#29413,#29414,#29415),.UNSPECIFIED.,.F.,.F.,(4,3,3,
3,3,3,3,4),(0.,0.000197996176151733,0.000401763276582256,0.000511744806759771,
0.000515920009585647,0.000722551962790744,0.000911736942394862,0.00102348961351954),
 .UNSPECIFIED.);
#686=B_SPLINE_CURVE_WITH_KNOTS('',3,(#29492,#29493,#29494,#29495,#29496,
#29497),.UNSPECIFIED.,.F.,.F.,(4,2,4),(0.,0.5,1.),.UNSPECIFIED.);
#687=B_SPLINE_CURVE_WITH_KNOTS('',3,(#29499,#29500,#29501,#29502,#29503,
#29504,#29505,#29506,#29507,#29508,#29509,#29510,#29511,#29512,#29513,#29514),
 .UNSPECIFIED.,.F.,.F.,(4,3,3,3,3,4),(0.,0.25,0.478355226420189,0.695629167073083,
0.902574508587078,1.),.UNSPECIFIED.);
#688=B_SPLINE_CURVE_WITH_KNOTS('',3,(#29515,#29516,#29517,#29518,#29519,
#29520),.UNSPECIFIED.,.F.,.F.,(4,2,4),(0.,0.5,1.),.UNSPECIFIED.);
#689=B_SPLINE_CURVE_WITH_KNOTS('',3,(#29585,#29586,#29587,#29588,#29589,
#29590),.UNSPECIFIED.,.F.,.F.,(4,2,4),(0.,0.5,1.),.UNSPECIFIED.);
#690=B_SPLINE_CURVE_WITH_KNOTS('',3,(#29592,#29593,#29594,#29595),
 .UNSPECIFIED.,.F.,.F.,(4,4),(0.,1.),.UNSPECIFIED.);
#691=B_SPLINE_CURVE_WITH_KNOTS('',3,(#29596,#29597,#29598,#29599,#29600,
#29601),.UNSPECIFIED.,.F.,.F.,(4,2,4),(0.,0.5,1.),.UNSPECIFIED.);
#692=B_SPLINE_CURVE_WITH_KNOTS('',3,(#29662,#29663,#29664,#29665,#29666,
#29667,#29668,#29669,#29670,#29671,#29672,#29673,#29674),.UNSPECIFIED.,
 .F.,.F.,(4,3,3,3,4),(0.,0.223169250634155,0.461855220689887,0.714975201892481,
1.),.UNSPECIFIED.);
#693=B_SPLINE_CURVE_WITH_KNOTS('',3,(#29675,#29676,#29677,#29678,#29679,
#29680),.UNSPECIFIED.,.F.,.F.,(4,2,4),(0.,0.5,1.),.UNSPECIFIED.);
#694=B_SPLINE_CURVE_WITH_KNOTS('',3,(#29742,#29743,#29744,#29745,#29746,
#29747,#29748,#29749,#29750,#29751,#29752,#29753,#29754,#29755,#29756,#29757),
 .UNSPECIFIED.,.F.,.F.,(4,3,3,3,3,4),(0.,0.26951546128406,0.518490249146965,
0.759245124573483,0.982227995955573,1.),.UNSPECIFIED.);
#695=B_SPLINE_CURVE_WITH_KNOTS('',3,(#29758,#29759,#29760,#29761,#29762,
#29763),.UNSPECIFIED.,.F.,.F.,(4,2,4),(0.,0.5,1.),.UNSPECIFIED.);
#696=B_SPLINE_CURVE_WITH_KNOTS('',3,(#29828,#29829,#29830,#29831),
 .UNSPECIFIED.,.F.,.F.,(4,4),(0.,1.),.UNSPECIFIED.);
#697=B_SPLINE_CURVE_WITH_KNOTS('',3,(#29833,#29834,#29835,#29836,#29837,
#29838,#29839,#29840,#29841,#29842,#29843,#29844,#29845,#29846,#29847,#29848,
#29849,#29850,#29851,#29852,#29853,#29854,#29855,#29856,#29857,#29858,#29859,
#29860,#29861,#29862,#29863,#29864,#29865,#29866,#29867,#29868,#29869,#29870,
#29871,#29872,#29873,#29874,#29875,#29876,#29877,#29878,#29879,#29880,#29881,
#29882,#29883,#29884,#29885,#29886,#29887,#29888,#29889,#29890,#29891,#29892,
#29893,#29894,#29895,#29896),.UNSPECIFIED.,.F.,.F.,(4,3,3,3,3,3,3,3,3,3,
3,3,3,3,3,3,3,3,3,3,3,4),(0.,0.184274983493926,0.325645671627907,0.482911947486233,
0.55677277721243,0.609022292004883,0.640178223344559,0.724682266712519,
0.782814976637048,0.841808654689151,0.899384096462184,0.938008402815887,
0.960709962461591,0.975964848021033,0.985714019774265,0.992447416236639,
0.995463191527497,0.997731595763749,0.998865797881874,0.999432898547245,
0.999931188332118,0.999999999212616),.UNSPECIFIED.);
#698=B_SPLINE_CURVE_WITH_KNOTS('',3,(#29897,#29898,#29899,#29900,#29901,
#29902),.UNSPECIFIED.,.F.,.F.,(4,2,4),(0.,0.5,1.),.UNSPECIFIED.);
#699=B_SPLINE_CURVE_WITH_KNOTS('',3,(#29953,#29954,#29955,#29956,#29957,
#29958),.UNSPECIFIED.,.F.,.F.,(4,2,4),(0.,0.5,1.),.UNSPECIFIED.);
#700=B_SPLINE_CURVE_WITH_KNOTS('',3,(#29959,#29960,#29961,#29962,#29963,
#29964,#29965,#29966,#29967,#29968,#29969,#29970,#29971,#29972,#29973,#29974),
 .UNSPECIFIED.,.F.,.F.,(4,3,3,3,3,4),(0.,0.205895634064056,0.424355643769067,
0.652797994841561,0.901136507518082,1.),.UNSPECIFIED.);
#701=B_SPLINE_CURVE_WITH_KNOTS('',3,(#29975,#29976,#29977,#29978,#29979,
#29980),.UNSPECIFIED.,.F.,.F.,(4,2,4),(0.,0.5,1.),.UNSPECIFIED.);
#702=B_SPLINE_CURVE_WITH_KNOTS('',3,(#30030,#30031,#30032,#30033,#30034,
#30035,#30036,#30037,#30038,#30039,#30040,#30041,#30042,#30043,#30044,#30045),
 .UNSPECIFIED.,.F.,.F.,(4,3,3,3,3,4),(0.,0.25,0.478355226419942,0.695629167072226,
0.902574508585992,1.),.UNSPECIFIED.);
#703=B_SPLINE_CURVE_WITH_KNOTS('',3,(#30046,#30047,#30048,#30049,#30050,
#30051),.UNSPECIFIED.,.F.,.F.,(4,2,4),(0.,0.5,1.),.UNSPECIFIED.);
#704=B_SPLINE_CURVE_WITH_KNOTS('',3,(#30116,#30117,#30118,#30119,#30120,
#30121),.UNSPECIFIED.,.F.,.F.,(4,2,4),(0.,0.5,1.),.UNSPECIFIED.);
#705=B_SPLINE_CURVE_WITH_KNOTS('',3,(#30123,#30124,#30125,#30126),
 .UNSPECIFIED.,.F.,.F.,(4,4),(0.,1.),.UNSPECIFIED.);
#706=B_SPLINE_CURVE_WITH_KNOTS('',3,(#30127,#30128,#30129,#30130,#30131,
#30132),.UNSPECIFIED.,.F.,.F.,(4,2,4),(0.,0.5,1.),.UNSPECIFIED.);
#707=B_SPLINE_CURVE_WITH_KNOTS('',3,(#30193,#30194,#30195,#30196,#30197,
#30198,#30199,#30200,#30201,#30202,#30203,#30204,#30205),.UNSPECIFIED.,
 .F.,.F.,(4,3,3,3,4),(0.,0.223169250633592,0.461855220688884,0.714975201891238,
1.),.UNSPECIFIED.);
#708=B_SPLINE_CURVE_WITH_KNOTS('',3,(#30206,#30207,#30208,#30209,#30210,
#30211),.UNSPECIFIED.,.F.,.F.,(4,2,4),(0.,0.5,1.),.UNSPECIFIED.);
#709=B_SPLINE_CURVE_WITH_KNOTS('',3,(#30274,#30275,#30276,#30277,#30278,
#30279),.UNSPECIFIED.,.F.,.F.,(4,2,4),(0.,0.5,1.),.UNSPECIFIED.);
#710=B_SPLINE_CURVE_WITH_KNOTS('',3,(#30341,#30342,#30343,#30344,#30345,
#30346),.UNSPECIFIED.,.F.,.F.,(4,2,4),(0.,0.5,1.),.UNSPECIFIED.);
#711=B_SPLINE_CURVE_WITH_KNOTS('',3,(#30348,#30349,#30350,#30351,#30352,
#30353,#30354,#30355,#30356,#30357,#30358,#30359,#30360,#30361,#30362,#30363),
 .UNSPECIFIED.,.F.,.F.,(4,3,3,3,3,4),(0.,0.269515461284092,0.518490249146695,
0.759245124573347,0.982227995954943,1.),.UNSPECIFIED.);
#712=B_SPLINE_CURVE_WITH_KNOTS('',3,(#30364,#30365,#30366,#30367,#30368,
#30369),.UNSPECIFIED.,.F.,.F.,(4,2,4),(0.,0.5,1.),.UNSPECIFIED.);
#713=B_SPLINE_CURVE_WITH_KNOTS('',3,(#30434,#30435,#30436,#30437),
 .UNSPECIFIED.,.F.,.F.,(4,4),(0.,1.),.UNSPECIFIED.);
#714=B_SPLINE_CURVE_WITH_KNOTS('',3,(#30439,#30440,#30441,#30442,#30443,
#30444),.UNSPECIFIED.,.F.,.F.,(4,2,4),(0.,0.5,1.),.UNSPECIFIED.);
#715=B_SPLINE_CURVE_WITH_KNOTS('',3,(#30445,#30446,#30447,#30448,#30449,
#30450),.UNSPECIFIED.,.F.,.F.,(4,2,4),(0.,0.5,1.),.UNSPECIFIED.);
#716=B_SPLINE_CURVE_WITH_KNOTS('',3,(#30499,#30500,#30501,#30502,#30503,
#30504,#30505,#30506,#30507,#30508,#30509,#30510,#30511,#30512,#30513,#30514),
 .UNSPECIFIED.,.F.,.F.,(4,3,3,3,3,4),(0.,0.205895634064936,0.424355643770462,
0.652797994843313,0.901136507520509,1.),.UNSPECIFIED.);
#717=B_SPLINE_CURVE_WITH_KNOTS('',3,(#30515,#30516,#30517,#30518,#30519,
#30520),.UNSPECIFIED.,.F.,.F.,(4,2,4),(0.,0.5,1.),.UNSPECIFIED.);
#718=B_SPLINE_CURVE_WITH_KNOTS('',3,(#30570,#30571,#30572,#30573,#30574,
#30575,#30576,#30577,#30578,#30579,#30580,#30581,#30582,#30583,#30584,#30585),
 .UNSPECIFIED.,.F.,.F.,(4,3,3,3,3,4),(0.,0.25,0.478355226421249,0.695629167075021,
0.902574508590587,1.),.UNSPECIFIED.);
#719=B_SPLINE_CURVE_WITH_KNOTS('',3,(#30586,#30587,#30588,#30589,#30590,
#30591),.UNSPECIFIED.,.F.,.F.,(4,2,4),(0.,0.5,1.),.UNSPECIFIED.);
#720=B_SPLINE_CURVE_WITH_KNOTS('',3,(#30656,#30657,#30658,#30659,#30660,
#30661),.UNSPECIFIED.,.F.,.F.,(4,2,4),(0.,0.5,1.),.UNSPECIFIED.);
#721=B_SPLINE_CURVE_WITH_KNOTS('',3,(#30663,#30664,#30665,#30666,#30667,
#30668,#30669,#30670,#30671,#30672,#30673,#30674,#30675,#30676,#30677,#30678,
#30679,#30680,#30681,#30682,#30683,#30684,#30685,#30686,#30687,#30688,#30689,
#30690,#30691,#30692,#30693,#30694,#30695,#30696,#30697,#30698,#30699,#30700,
#30701,#30702,#30703,#30704,#30705,#30706,#30707,#30708,#30709,#30710,#30711,
#30712,#30713,#30714,#30715,#30716,#30717),.UNSPECIFIED.,.F.,.F.,(4,3,3,
3,3,3,3,3,3,3,3,3,3,3,3,3,3,3,4),(0.,0.134829460600233,0.301935450994647,
0.331938859566448,0.520486721225732,0.653948260231371,0.766867850117276,
0.847465272943437,0.903670198362982,0.941441109775431,0.964211265170187,
0.978961680044948,0.986981420564942,0.993490710282471,0.996745355141236,
0.998372677570618,0.999186338355832,0.999785281511195,0.999999999141046),
 .UNSPECIFIED.);
#722=B_SPLINE_CURVE_WITH_KNOTS('',3,(#30718,#30719,#30720,#30721,#30722,
#30723),.UNSPECIFIED.,.F.,.F.,(4,2,4),(0.,0.5,1.),.UNSPECIFIED.);
#723=B_SPLINE_CURVE_WITH_KNOTS('',3,(#30774,#30775,#30776,#30777,#30778,
#30779),.UNSPECIFIED.,.F.,.F.,(4,2,4),(0.,0.5,1.),.UNSPECIFIED.);
#724=B_SPLINE_CURVE_WITH_KNOTS('',3,(#30780,#30781,#30782,#30783,#30784,
#30785,#30786,#30787,#30788,#30789,#30790,#30791,#30792,#30793,#30794,#30795),
 .UNSPECIFIED.,.F.,.F.,(4,3,3,3,3,4),(0.,0.205895634064023,0.424355643768918,
0.65279799484117,0.901136507517712,1.),.UNSPECIFIED.);
#725=B_SPLINE_CURVE_WITH_KNOTS('',3,(#30796,#30797,#30798,#30799,#30800,
#30801),.UNSPECIFIED.,.F.,.F.,(4,2,4),(0.,0.5,1.),.UNSPECIFIED.);
#726=B_SPLINE_CURVE_WITH_KNOTS('',3,(#30851,#30852,#30853,#30854,#30855,
#30856,#30857,#30858,#30859,#30860,#30861,#30862,#30863,#30864,#30865,#30866),
 .UNSPECIFIED.,.F.,.F.,(4,3,3,3,3,4),(0.,0.25,0.478355226420375,0.695629167073178,
0.902574508587577,1.),.UNSPECIFIED.);
#727=B_SPLINE_CURVE_WITH_KNOTS('',3,(#30867,#30868,#30869,#30870,#30871,
#30872),.UNSPECIFIED.,.F.,.F.,(4,2,4),(0.,0.5,1.),.UNSPECIFIED.);
#728=B_SPLINE_CURVE_WITH_KNOTS('',3,(#30937,#30938,#30939,#30940,#30941,
#30942),.UNSPECIFIED.,.F.,.F.,(4,2,4),(0.,0.5,1.),.UNSPECIFIED.);
#729=B_SPLINE_CURVE_WITH_KNOTS('',3,(#30944,#30945,#30946,#30947,#30948,
#30949,#30950,#30951,#30952,#30953,#30954,#30955,#30956,#30957,#30958,#30959,
#30960,#30961,#30962,#30963,#30964,#30965,#30966,#30967,#30968,#30969,#30970,
#30971,#30972,#30973,#30974,#30975,#30976,#30977,#30978,#30979,#30980,#30981,
#30982,#30983,#30984,#30985,#30986,#30987,#30988,#30989,#30990,#30991,#30992,
#30993,#30994,#30995,#30996,#30997,#30998),.UNSPECIFIED.,.F.,.F.,(4,3,3,
3,3,3,3,3,3,3,3,3,3,3,3,3,3,3,4),(0.,0.134829524450431,0.301935899082962,
0.331938859566374,0.520486852331808,0.653948260231437,0.765695406250714,
0.845739463039844,0.901726408213813,0.939310939832059,0.962010705761424,
0.977750708016431,0.988647584692032,0.993490710271438,0.996745355135719,
0.998372677567859,0.999186338354459,0.999785281509885,0.999999999141059),
 .UNSPECIFIED.);
#730=B_SPLINE_CURVE_WITH_KNOTS('',3,(#30999,#31000,#31001,#31002,#31003,
#31004),.UNSPECIFIED.,.F.,.F.,(4,2,4),(0.,0.5,1.),.UNSPECIFIED.);
#731=B_SPLINE_CURVE_WITH_KNOTS('',3,(#31066,#31067,#31068,#31069,#31070,
#31071),.UNSPECIFIED.,.F.,.F.,(4,2,4),(0.,0.5,1.),.UNSPECIFIED.);
#732=B_SPLINE_CURVE_WITH_KNOTS('',3,(#31134,#31135,#31136,#31137,#31138,
#31139),.UNSPECIFIED.,.F.,.F.,(4,2,4),(0.,0.5,1.),.UNSPECIFIED.);
#733=B_SPLINE_CURVE_WITH_KNOTS('',3,(#31161,#31162,#31163,#31164,#31165,
#31166,#31167,#31168,#31169,#31170,#31171,#31172,#31173,#31174,#31175,#31176,
#31177,#31178,#31179,#31180,#31181,#31182),.UNSPECIFIED.,.F.,.F.,(4,3,3,
3,3,3,3,4),(0.,0.000123360913687075,0.00025951037912914,0.000406482329163153,
0.000585460068616017,0.000594183385201075,0.000955339327009254,0.00118832361361941),
 .UNSPECIFIED.);
#734=B_SPLINE_CURVE_WITH_KNOTS('',3,(#31203,#31204,#31205,#31206,#31207,
#31208,#31209,#31210,#31211,#31212,#31213,#31214,#31215,#31216,#31217,#31218,
#31219,#31220,#31221,#31222,#31223,#31224),.UNSPECIFIED.,.F.,.F.,(4,3,3,
3,3,3,3,4),(4.30167323683359E-8,0.00029867815700615,0.000593798351081719,
0.000602268552183542,0.0007833357220942,0.000949532856772951,0.00110145074954496,
0.00118759670216344),.UNSPECIFIED.);
#735=B_SPLINE_CURVE_WITH_KNOTS('',3,(#31273,#31274,#31275,#31276,#31277,
#31278),.UNSPECIFIED.,.F.,.F.,(4,2,4),(0.,0.5,1.),.UNSPECIFIED.);
#736=B_SPLINE_CURVE_WITH_KNOTS('',3,(#31350,#31351,#31352,#31353,#31354,
#31355,#31356,#31357,#31358,#31359,#31360,#31361,#31362,#31363,#31364,#31365,
#31366,#31367,#31368,#31369,#31370,#31371,#31372,#31373,#31374,#31375,#31376,
#31377,#31378,#31379,#31380,#31381,#31382,#31383,#31384,#31385,#31386,#31387,
#31388,#31389,#31390,#31391,#31392,#31393,#31394,#31395,#31396,#31397,#31398,
#31399,#31400,#31401,#31402,#31403,#31404),.UNSPECIFIED.,.F.,.F.,(4,3,3,
3,3,3,3,3,3,3,3,3,3,3,3,3,3,3,4),(8.57224357468246E-10,0.000627254895781897,
0.00125605220505132,0.00251210441010265,0.00502420882020529,0.0136336628022367,
0.0252314236373915,0.0410680722324126,0.0681502624529836,0.113858512147431,
0.184994280858008,0.291969184096878,0.346051748925883,0.519710693631118,
0.668061140433536,0.827606356909723,0.964640047971178,0.98715157338591,
1.),.UNSPECIFIED.);
#737=B_SPLINE_CURVE_WITH_KNOTS('',3,(#31423,#31424,#31425,#31426,#31427,
#31428,#31429,#31430,#31431,#31432,#31433,#31434,#31435,#31436,#31437,#31438,
#31439,#31440,#31441,#31442,#31443,#31444,#31445,#31446,#31447),
 .UNSPECIFIED.,.F.,.F.,(4,3,3,3,3,3,3,3,4),(4.30147703006247E-8,0.000270288099787492,
0.000513938606912812,0.00059425364289645,0.000603710958331439,0.000790752044623706,
0.000965824226330528,0.00112861151875137,0.0011885072857929),
 .UNSPECIFIED.);
#738=B_SPLINE_CURVE_WITH_KNOTS('',3,(#31466,#31467,#31468,#31469,#31470,
#31471,#31472,#31473,#31474,#31475,#31476,#31477,#31478,#31479,#31480,#31481,
#31482,#31483,#31484,#31485,#31486,#31487),.UNSPECIFIED.,.F.,.F.,(4,3,3,
3,3,3,3,4),(0.,0.000158882102081258,0.00032688426378663,0.000515357261128183,
0.000587493639452289,0.000595665178359072,0.000945792692676976,0.00119128711121805),
 .UNSPECIFIED.);
#739=B_SPLINE_CURVE_WITH_KNOTS('',3,(#31508,#31509,#31510,#31511,#31512,
#31513,#31514,#31515,#31516,#31517,#31518,#31519,#31520,#31521,#31522,#31523,
#31524,#31525,#31526,#31527,#31528,#31529),.UNSPECIFIED.,.F.,.F.,(4,3,3,
3,3,3,3,4),(1.90660672321663E-16,0.000123777251417005,0.000260370684246027,
0.000407829318327282,0.00058555605220498,0.000594289208708569,0.000954348914487693,
0.00118853525410901),.UNSPECIFIED.);
#740=B_SPLINE_CURVE_WITH_KNOTS('',3,(#31604,#31605,#31606,#31607,#31608,
#31609),.UNSPECIFIED.,.F.,.F.,(4,2,4),(0.,0.5,1.),.UNSPECIFIED.);
#741=B_SPLINE_CURVE_WITH_KNOTS('',3,(#31638,#31639,#31640,#31641,#31642,
#31643,#31644,#31645,#31646,#31647,#31648,#31649,#31650,#31651,#31652,#31653,
#31654,#31655,#31656,#31657,#31658,#31659,#31660,#31661,#31662),
 .UNSPECIFIED.,.F.,.F.,(4,3,3,3,3,3,3,3,4),(0.,0.000164956261028691,0.000338143702530957,
0.000527870844727718,0.000582731284092286,0.000592094961956777,0.000848990011105951,
0.00112806173363088,0.00118414707026094),.UNSPECIFIED.);
#742=B_SPLINE_CURVE_WITH_KNOTS('',3,(#31788,#31789,#31790,#31791,#31792,
#31793,#31794,#31795,#31796,#31797,#31798,#31799,#31800,#31801,#31802,#31803,
#31804,#31805,#31806,#31807,#31808,#31809,#31810,#31811,#31812,#31813,#31814,
#31815,#31816,#31817,#31818,#31819,#31820,#31821,#31822,#31823,#31824,#31825,
#31826,#31827,#31828,#31829,#31830,#31831,#31832,#31833,#31834,#31835,#31836,
#31837,#31838,#31839),.UNSPECIFIED.,.F.,.F.,(4,3,3,3,3,3,3,3,3,3,3,3,3,
3,3,3,3,4),(8.57205116275548E-10,0.00062725489807238,0.00125605219573295,
0.0025121043914659,0.00502420878293179,0.0136336627391616,0.0252314235092207,
0.0410680718371953,0.0681502630269255,0.113858513076608,0.184994282344012,
0.291969186221209,0.34605174892585,0.519710992297142,0.668061140433496,
0.834030570216748,0.968862259433357,1.),.UNSPECIFIED.);
#743=B_SPLINE_CURVE_WITH_KNOTS('',3,(#31858,#31859,#31860,#31861,#31862,
#31863,#31864,#31865,#31866,#31867,#31868,#31869,#31870,#31871,#31872,#31873,
#31874,#31875,#31876,#31877,#31878,#31879),.UNSPECIFIED.,.F.,.F.,(4,3,3,
3,3,3,3,4),(4.30167364622209E-8,0.000298678157011449,0.000593798351081719,
0.000602268552183536,0.000783335722089147,0.000949532856766907,0.00110145074954175,
0.00118759670216344),.UNSPECIFIED.);
#744=B_SPLINE_CURVE_WITH_KNOTS('',3,(#31997,#31998,#31999,#32000,#32001,
#32002,#32003,#32004,#32005,#32006,#32007,#32008,#32009,#32010,#32011,#32012,
#32013,#32014,#32015,#32016,#32017,#32018),.UNSPECIFIED.,.F.,.F.,(4,3,3,
3,3,3,3,4),(0.,0.000123360913700324,0.000259510379141672,0.00040648232915685,
0.000585460068616011,0.000594183385201068,0.000955339326765691,0.00118832361362475),
 .UNSPECIFIED.);
#745=B_SPLINE_CURVE_WITH_KNOTS('',3,(#32202,#32203,#32204,#32205,#32206,
#32207,#32208,#32209,#32210,#32211),.UNSPECIFIED.,.F.,.F.,(4,2,2,2,4),(0.276263636539841,
0.629117133783239,1.26931031034628,1.89807374671191,2.54124258875015),
 .UNSPECIFIED.);
#746=B_SPLINE_CURVE_WITH_KNOTS('',3,(#32215,#32216,#32217,#32218,#32219,
#32220,#32221,#32222,#32223,#32224),.UNSPECIFIED.,.F.,.F.,(4,2,2,2,4),(1.00000001210554E-6,
0.634808922936136,1.24939733333229,1.87099835051043,2.49652016978958),
 .UNSPECIFIED.);
#747=B_SPLINE_CURVE_WITH_KNOTS('',3,(#32226,#32227,#32228,#32229,#32230,
#32231,#32232,#32233,#32234,#32235),.UNSPECIFIED.,.F.,.F.,(4,2,2,2,4),(9.90463797838316E-7,
0.628842488476587,1.26874459572359,1.89778547935364,2.54125154834499),
 .UNSPECIFIED.);
#748=B_SPLINE_CURVE_WITH_KNOTS('',3,(#32239,#32240,#32241,#32242,#32243,
#32244,#32245,#32246,#32247,#32248),.UNSPECIFIED.,.F.,.F.,(4,2,2,2,4),(1.00000001226936E-6,
0.634808922936138,1.24939733333229,1.87099835051041,2.49652016978955),
 .UNSPECIFIED.);
#749=B_SPLINE_CURVE_WITH_KNOTS('',3,(#32250,#32251,#32252,#32253,#32254,
#32255,#32256,#32257,#32258,#32259),.UNSPECIFIED.,.F.,.F.,(4,2,2,2,4),(9.90463797798848E-7,
0.62884248847666,1.26874459572371,1.8977854793538,2.54125154834516),
 .UNSPECIFIED.);
#750=B_SPLINE_CURVE_WITH_KNOTS('',3,(#32265,#32266,#32267,#32268,#32269,
#32270,#32271,#32272,#32273,#32274),.UNSPECIFIED.,.F.,.F.,(4,2,2,2,4),(1.00000001376695E-6,
0.680457901220549,1.33757522030194,1.9141295972232,2.49600347486028),
 .UNSPECIFIED.);
#751=B_SPLINE_CURVE_WITH_KNOTS('',3,(#32276,#32277,#32278,#32279,#32280,
#32281,#32282,#32283,#32284,#32285),.UNSPECIFIED.,.F.,.F.,(4,2,2,2,4),(-2.54325661086045,
-1.81843643838175,-1.11345157109682,-0.553213495814432,-1.00000000724521E-6),
 .UNSPECIFIED.);
#752=B_SPLINE_CURVE_WITH_KNOTS('',3,(#32289,#32290,#32291,#32292,#32293,
#32294,#32295,#32296,#32297,#32298),.UNSPECIFIED.,.F.,.F.,(4,2,2,2,4),(1.00000001195455E-6,
0.634808922936142,1.24939733333231,1.87099835051046,2.49652016978959),
 .UNSPECIFIED.);
#753=B_SPLINE_CURVE_WITH_KNOTS('',3,(#32300,#32301,#32302,#32303,#32304,
#32305,#32306,#32307,#32308,#32309),.UNSPECIFIED.,.F.,.F.,(4,2,2,2,4),(9.90463797727588E-7,
0.628842488476649,1.26874459572375,1.89778547935391,2.54125154834539),
 .UNSPECIFIED.);
#754=B_SPLINE_CURVE_WITH_KNOTS('',3,(#32313,#32314,#32315,#32316,#32317,
#32318,#32319,#32320,#32321,#32322),.UNSPECIFIED.,.F.,.F.,(4,2,2,2,4),(1.00000001181796E-6,
0.634808922936134,1.24939733333227,1.87099835051039,2.4965201697895),
 .UNSPECIFIED.);
#755=B_SPLINE_CURVE_WITH_KNOTS('',3,(#32324,#32325,#32326,#32327,#32328,
#32329,#32330,#32331,#32332,#32333),.UNSPECIFIED.,.F.,.F.,(4,2,2,2,4),(9.90463798206886E-7,
0.6288424884766,1.26874459572362,1.89778547935369,2.54125154834506),
 .UNSPECIFIED.);
#756=B_SPLINE_CURVE_WITH_KNOTS('',3,(#32337,#32338,#32339,#32340,#32341,
#32342,#32343,#32344,#32345,#32346),.UNSPECIFIED.,.F.,.F.,(4,2,2,2,4),(1.00000001290734E-6,
0.634808922936141,1.24939733333231,1.87099835051047,2.49652016978959),
 .UNSPECIFIED.);
#757=B_SPLINE_CURVE_WITH_KNOTS('',3,(#32348,#32349,#32350,#32351,#32352,
#32353,#32354,#32355,#32356,#32357),.UNSPECIFIED.,.F.,.F.,(4,2,2,2,4),(9.9046379766505E-7,
0.628842488476696,1.26874459572384,1.89778547935403,2.54125154834553),
 .UNSPECIFIED.);
#758=B_SPLINE_CURVE_WITH_KNOTS('',3,(#32363,#32364,#32365,#32366),
 .UNSPECIFIED.,.F.,.F.,(4,4),(2.08467470935283,2.49651756792621),
 .UNSPECIFIED.);
#759=B_SPLINE_CURVE_WITH_KNOTS('',3,(#32367,#32368,#32369,#32370),
 .UNSPECIFIED.,.F.,.F.,(4,4),(9.99129608606638E-7,0.276263636539841),
 .UNSPECIFIED.);
#760=B_SPLINE_CURVE_WITH_KNOTS('',3,(#32396,#32397,#32398,#32399,#32400,
#32401,#32402,#32403,#32404,#32405),.UNSPECIFIED.,.F.,.F.,(4,2,2,2,4),(-4.16323414483187,
-3.10732772174226,-2.02362880934783,-0.957049330172841,-1.00000000020696E-6),
 .UNSPECIFIED.);
#761=B_SPLINE_CURVE_WITH_KNOTS('',3,(#32408,#32409,#32410,#32411,#32412,
#32413,#32414,#32415),.UNSPECIFIED.,.F.,.F.,(4,2,2,4),(-3.79953187020984,
-2.88369731719006,-1.89738143645868,-9.66593405760108E-7),.UNSPECIFIED.);
#762=B_SPLINE_CURVE_WITH_KNOTS('',3,(#32421,#32422,#32423,#32424,#32425,
#32426,#32427,#32428,#32429,#32430),.UNSPECIFIED.,.F.,.F.,(4,2,2,2,4),(-0.416082413068314,
-0.360585309636598,-0.306832956120282,-0.200050893588257,-1.00000028174785E-6),
 .UNSPECIFIED.);
#763=B_SPLINE_CURVE_WITH_KNOTS('',3,(#32432,#32433,#32434,#32435,#32436,
#32437,#32438),.UNSPECIFIED.,.F.,.F.,(4,3,4),(6.80202241033507E-5,0.000423360973853086,
0.00074564696373395),.UNSPECIFIED.);
#764=B_SPLINE_CURVE_WITH_KNOTS('',3,(#32439,#32440,#32441,#32442,#32443,
#32444,#32445,#32446,#32447,#32448,#32449,#32450),.UNSPECIFIED.,.F.,.F.,
(4,2,2,2,2,4),(-0.410791572873837,-0.314481286284345,-0.223124863886982,
-0.108117426869209,-0.0434561601514269,-1.00000038416592E-6),
 .UNSPECIFIED.);
#765=B_SPLINE_CURVE_WITH_KNOTS('',3,(#32452,#32453,#32454,#32455,#32456,
#32457,#32458,#32459,#32460,#32461),.UNSPECIFIED.,.F.,.F.,(4,2,2,2,4),(-0.416082413067571,
-0.360585309635978,-0.306832956119768,-0.200050893587991,-1.00000028163683E-6),
 .UNSPECIFIED.);
#766=B_SPLINE_CURVE_WITH_KNOTS('',3,(#32463,#32464,#32465,#32466,#32467,
#32468,#32469),.UNSPECIFIED.,.F.,.F.,(4,3,4),(6.80202241033475E-5,0.000423360973855293,
0.000745646963733951),.UNSPECIFIED.);
#767=B_SPLINE_CURVE_WITH_KNOTS('',3,(#32470,#32471,#32472,#32473,#32474,
#32475,#32476,#32477,#32478,#32479,#32480,#32481),.UNSPECIFIED.,.F.,.F.,
(4,2,2,2,2,4),(-0.410791572872332,-0.314481286283402,-0.223124863886612,
-0.108117426869205,-0.0434561601514252,-1.00000038433246E-6),
 .UNSPECIFIED.);
#768=B_SPLINE_CURVE_WITH_KNOTS('',3,(#32483,#32484,#32485,#32486,#32487,
#32488,#32489,#32490,#32491,#32492),.UNSPECIFIED.,.F.,.F.,(4,2,2,2,4),(-0.416082413068048,
-0.360584308223045,-0.30683210398761,-0.2000503380104,-1.00000028219194E-6),
 .UNSPECIFIED.);
#769=B_SPLINE_CURVE_WITH_KNOTS('',3,(#32494,#32495,#32496,#32497,#32498,
#32499,#32500),.UNSPECIFIED.,.F.,.F.,(4,3,4),(6.80202241033436E-5,0.000423360973850319,
0.000745646963733949),.UNSPECIFIED.);
#770=B_SPLINE_CURVE_WITH_KNOTS('',3,(#32502,#32503,#32504,#32505,#32506,
#32507,#32508,#32509,#32510,#32511,#32512,#32513),.UNSPECIFIED.,.F.,.F.,
(4,2,2,2,2,4),(-0.410791572872144,-0.314481286283286,-0.223124863886566,
-0.108117426869204,-0.043456160151425,-1.00000038433246E-6),
 .UNSPECIFIED.);
#771=B_SPLINE_CURVE_WITH_KNOTS('',3,(#32516,#32517,#32518,#32519,#32520,
#32521,#32522,#32523,#32524,#32525),.UNSPECIFIED.,.F.,.F.,(4,2,2,2,4),(-0.416082413068513,
-0.360585309636774,-0.306832956120457,-0.200050893588368,-1.00000028135927E-6),
 .UNSPECIFIED.);
#772=B_SPLINE_CURVE_WITH_KNOTS('',3,(#32527,#32528,#32529,#32530,#32531,
#32532,#32533),.UNSPECIFIED.,.F.,.F.,(4,3,4),(6.80202241033427E-5,0.000423360973852712,
0.00074564696373395),.UNSPECIFIED.);
#773=B_SPLINE_CURVE_WITH_KNOTS('',3,(#32534,#32535,#32536,#32537,#32538,
#32539,#32540,#32541,#32542,#32543,#32544,#32545),.UNSPECIFIED.,.F.,.F.,
(4,2,2,2,2,4),(-0.410791572872511,-0.314481286283472,-0.223124863886587,
-0.108117426869161,-0.0434561601514204,-1.00000038433246E-6),
 .UNSPECIFIED.);
#774=B_SPLINE_CURVE_WITH_KNOTS('',3,(#32547,#32548,#32549,#32550,#32551,
#32552,#32553,#32554,#32555,#32556),.UNSPECIFIED.,.F.,.F.,(4,2,2,2,4),(-0.416082413068343,
-0.360584308223297,-0.306832103987803,-0.200050338010502,-1.00000028147029E-6),
 .UNSPECIFIED.);
#775=B_SPLINE_CURVE_WITH_KNOTS('',3,(#32558,#32559,#32560,#32561,#32562,
#32563,#32564),.UNSPECIFIED.,.F.,.F.,(4,3,4),(6.80202241033462E-5,0.000423360973856063,
0.000745646963733952),.UNSPECIFIED.);
#776=B_SPLINE_CURVE_WITH_KNOTS('',3,(#32565,#32566,#32567,#32568,#32569,
#32570,#32571,#32572,#32573,#32574,#32575,#32576),.UNSPECIFIED.,.F.,.F.,
(4,2,2,2,2,4),(-0.410791572872343,-0.314480677796283,-0.223124432164779,
-0.108117217674975,-0.0434560760701422,-1.00000038427694E-6),
 .UNSPECIFIED.);
#777=B_SPLINE_CURVE_WITH_KNOTS('',3,(#32578,#32579,#32580,#32581,#32582,
#32583,#32584,#32585,#32586,#32587),.UNSPECIFIED.,.F.,.F.,(4,2,2,2,4),(-0.41608241306817,
-0.360584308223134,-0.306832103987679,-0.200050338010442,-1.00000028141478E-6),
 .UNSPECIFIED.);
#778=B_SPLINE_CURVE_WITH_KNOTS('',3,(#32589,#32590,#32591,#32592,#32593,
#32594,#32595),.UNSPECIFIED.,.F.,.F.,(4,3,4),(6.80202241033419E-5,0.000423360973850686,
0.000745646963733949),.UNSPECIFIED.);
#779=B_SPLINE_CURVE_WITH_KNOTS('',3,(#32596,#32597,#32598,#32599,#32600,
#32601,#32602,#32603,#32604,#32605,#32606,#32607),.UNSPECIFIED.,.F.,.F.,
(4,2,2,2,2,4),(-0.410791572871703,-0.314481286282978,-0.223124863886396,
-0.108117426869157,-0.0434561601514192,-1.00000038499859E-6),
 .UNSPECIFIED.);
#780=B_SPLINE_CURVE_WITH_KNOTS('',3,(#32609,#32610,#32611,#32612,#32613,
#32614,#32615,#32616,#32617,#32618),.UNSPECIFIED.,.F.,.F.,(4,2,2,2,4),(-0.416082413069045,
-0.360585309637195,-0.306832956120764,-0.200050893588512,-1.00000028130376E-6),
 .UNSPECIFIED.);
#781=B_SPLINE_CURVE_WITH_KNOTS('',3,(#32620,#32621,#32622,#32623,#32624,
#32625,#32626),.UNSPECIFIED.,.F.,.F.,(4,3,4),(6.80202241033508E-5,0.000423360973851168,
0.000745646963733949),.UNSPECIFIED.);
#782=B_SPLINE_CURVE_WITH_KNOTS('',3,(#32627,#32628,#32629,#32630,#32631,
#32632,#32633,#32634,#32635,#32636,#32637,#32638),.UNSPECIFIED.,.F.,.F.,
(4,2,2,2,2,4),(-0.410791572871773,-0.314480677795932,-0.223124432164652,
-0.108117217674975,-0.0434560760701403,-1.0000003840549E-6),
 .UNSPECIFIED.);
#783=B_SPLINE_CURVE_WITH_KNOTS('',3,(#32640,#32641,#32642,#32643,#32644,
#32645,#32646,#32647,#32648,#32649),.UNSPECIFIED.,.F.,.F.,(4,2,2,2,4),(1.00000001324041E-6,
0.635035409735681,1.24983493879194,1.87121208677302,2.08467470935283),
 .UNSPECIFIED.);
#784=B_SPLINE_CURVE_WITH_KNOTS('',3,(#32742,#32743,#32744,#32745,#32746,
#32747),.UNSPECIFIED.,.F.,.F.,(4,2,4),(-3.04622791888176,-1.52235182247481,
-1.00000000191613E-6),.UNSPECIFIED.);
#785=B_SPLINE_CURVE_WITH_KNOTS('',3,(#32750,#32751,#32752,#32753,#32754,
#32755),.UNSPECIFIED.,.F.,.F.,(4,2,4),(-3.11031182561968,-1.55397466140411,
-1.00000000147205E-6),.UNSPECIFIED.);
#786=B_SPLINE_CURVE_WITH_KNOTS('',3,(#33029,#33030,#33031,#33032,#33033,
#33034,#33035,#33036,#33037,#33038,#33039,#33040,#33041,#33042,#33043,#33044,
#33045,#33046,#33047,#33048,#33049,#33050,#33051,#33052,#33053),
 .UNSPECIFIED.,.F.,.F.,(4,3,3,3,3,3,3,3,4),(0.169188754138552,0.21259195128669,
0.318887932838093,0.389751920511185,0.460615908147183,0.566911889469088,
0.637775876850632,0.708639855735204,0.737840512980669),.UNSPECIFIED.);
#787=B_SPLINE_CURVE_WITH_KNOTS('',3,(#33054,#33055,#33056,#33057,#33058,
#33059,#33060,#33061),.UNSPECIFIED.,.F.,.F.,(4,2,2,4),(9.75623641873708E-7,
1.95229904030299,2.9045389655587,3.79841482214538),.UNSPECIFIED.);
#788=B_SPLINE_CURVE_WITH_KNOTS('',3,(#33351,#33352,#33353,#33354,#33355,
#33356,#33357,#33358,#33359,#33360),.UNSPECIFIED.,.F.,.F.,(4,2,2,2,4),(9.99999995110559E-7,
0.975019787491179,2.07352620290794,3.13207699922824,4.16223065422311),
 .UNSPECIFIED.);
#789=B_SPLINE_CURVE_WITH_KNOTS('',3,(#33651,#33652,#33653,#33654,#33655,
#33656),.UNSPECIFIED.,.F.,.F.,(4,2,4),(-3.11031182562015,-1.55397466140411,
-1.00000000147205E-6),.UNSPECIFIED.);
#790=B_SPLINE_CURVE_WITH_KNOTS('',3,(#33658,#33659,#33660,#33661,#33662,
#33663,#33664,#33665,#33666,#33667),.UNSPECIFIED.,.F.,.F.,(4,2,2,2,4),(9.99999994354565E-7,
0.975020551048607,2.07352669960846,3.13207725037619,4.16223066592058),
 .UNSPECIFIED.);
#791=B_SPLINE_CURVE_WITH_KNOTS('',3,(#33668,#33669,#33670,#33671,#33672,
#33673,#33674,#33675,#33676,#33677,#33678,#33679,#33680,#33681,#33682,#33683,
#33684,#33685,#33686,#33687,#33688,#33689,#33690,#33691,#33692),
 .UNSPECIFIED.,.F.,.F.,(4,3,3,3,3,3,3,3,4),(0.169188762886294,0.212591956720561,
0.318887932838093,0.389751920511184,0.460615908147183,0.566911889469088,
0.637775876850632,0.708639855735204,0.737840512980669),.UNSPECIFIED.);
#792=B_SPLINE_CURVE_WITH_KNOTS('',3,(#33966,#33967,#33968,#33969,#33970,
#33971,#33972,#33973),.UNSPECIFIED.,.F.,.F.,(4,2,2,4),(9.64894431166974E-7,
1.95229904275442,2.90453896597694,3.79841482198892),.UNSPECIFIED.);
#793=B_SPLINE_CURVE_WITH_KNOTS('',3,(#33974,#33975,#33976,#33977,#33978,
#33979),.UNSPECIFIED.,.F.,.F.,(4,2,4),(-3.04622791888257,-1.52235182247559,
-1.00000000236022E-6),.UNSPECIFIED.);
#794=B_SPLINE_CURVE_WITH_KNOTS('',3,(#34362,#34363,#34364,#34365,#34366,
#34367),.UNSPECIFIED.,.F.,.F.,(4,2,4),(-3.11031182562014,-1.5539746614041,
-1.00000000236022E-6),.UNSPECIFIED.);
#795=B_SPLINE_CURVE_WITH_KNOTS('',3,(#34369,#34370,#34371,#34372,#34373,
#34374,#34375,#34376,#34377,#34378),.UNSPECIFIED.,.F.,.F.,(4,2,2,2,4),(9.99999995275062E-7,
0.975019785302907,2.07352619778517,3.13207700287578,4.16223066592084),
 .UNSPECIFIED.);
#796=B_SPLINE_CURVE_WITH_KNOTS('',3,(#34379,#34380,#34381,#34382,#34383,
#34384,#34385,#34386,#34387,#34388,#34389,#34390,#34391,#34392,#34393,#34394,
#34395,#34396,#34397,#34398,#34399,#34400,#34401,#34402,#34403),
 .UNSPECIFIED.,.F.,.F.,(4,3,3,3,3,3,3,3,4),(0.169188762886294,0.212591956720561,
0.318887932838093,0.389751920511184,0.460615908147183,0.566911889469088,
0.637775876850632,0.708639855735204,0.737840512980669),.UNSPECIFIED.);
#797=B_SPLINE_CURVE_WITH_KNOTS('',3,(#34677,#34678,#34679,#34680,#34681,
#34682,#34683,#34684),.UNSPECIFIED.,.F.,.F.,(4,2,2,4),(9.64894429904643E-7,
1.95229950803617,2.90453965820161,3.7984148219903),.UNSPECIFIED.);
#798=B_SPLINE_CURVE_WITH_KNOTS('',3,(#34685,#34686,#34687,#34688,#34689,
#34690),.UNSPECIFIED.,.F.,.F.,(4,2,4),(-3.0462279188826,-1.52235182247563,
-1.00000000236022E-6),.UNSPECIFIED.);
#799=B_SPLINE_CURVE_WITH_KNOTS('',3,(#35073,#35074,#35075,#35076,#35077,
#35078),.UNSPECIFIED.,.F.,.F.,(4,2,4),(-3.11031182562016,-1.55397466140411,
-1.00000000147205E-6),.UNSPECIFIED.);
#800=B_SPLINE_CURVE_WITH_KNOTS('',3,(#35080,#35081,#35082,#35083,#35084,
#35085,#35086,#35087,#35088,#35089),.UNSPECIFIED.,.F.,.F.,(4,2,2,2,4),(9.99999995037368E-7,
0.975020551048589,2.07352669960851,3.13207725037625,4.16223066592104),
 .UNSPECIFIED.);
#801=B_SPLINE_CURVE_WITH_KNOTS('',3,(#35090,#35091,#35092,#35093,#35094,
#35095,#35096,#35097,#35098,#35099,#35100,#35101,#35102,#35103,#35104,#35105,
#35106,#35107,#35108,#35109,#35110,#35111,#35112,#35113,#35114),
 .UNSPECIFIED.,.F.,.F.,(4,3,3,3,3,3,3,3,4),(0.169188762886294,0.212591956720561,
0.318887932838093,0.389751920511184,0.460615908147183,0.566911889469088,
0.637775876850632,0.708639855735204,0.737840512980669),.UNSPECIFIED.);
#802=B_SPLINE_CURVE_WITH_KNOTS('',3,(#35388,#35389,#35390,#35391,#35392,
#35393,#35394,#35395),.UNSPECIFIED.,.F.,.F.,(4,2,2,4),(9.64894429706047E-7,
1.95229950803846,2.90453965820592,3.7984148219965),.UNSPECIFIED.);
#803=B_SPLINE_CURVE_WITH_KNOTS('',3,(#35396,#35397,#35398,#35399,#35400,
#35401),.UNSPECIFIED.,.F.,.F.,(4,2,4),(-3.04622791888258,-1.52235182247565,
-1.00000000147205E-6),.UNSPECIFIED.);
#804=B_SPLINE_CURVE_WITH_KNOTS('',3,(#35783,#35784,#35785,#35786,#35787,
#35788),.UNSPECIFIED.,.F.,.F.,(4,2,4),(-3.11031182562014,-1.5539746614041,
-1.00000000191613E-6),.UNSPECIFIED.);
#805=B_SPLINE_CURVE_WITH_KNOTS('',3,(#35789,#35790,#35791,#35792,#35793,
#35794,#35795,#35796,#35797,#35798,#35799,#35800,#35801,#35802,#35803,#35804,
#35805,#35806,#35807,#35808,#35809,#35810,#35811,#35812,#35813),
 .UNSPECIFIED.,.F.,.F.,(4,3,3,3,3,3,3,3,4),(0.169188754745471,0.212591956720561,
0.318887932838093,0.389751920511185,0.460615908147183,0.566911889469088,
0.637775876850632,0.708639855735204,0.737840512980669),.UNSPECIFIED.);
#806=B_SPLINE_CURVE_WITH_KNOTS('',3,(#36086,#36087,#36088,#36089,#36090,
#36091),.UNSPECIFIED.,.F.,.F.,(4,2,4),(-3.04622791888258,-1.5223518224756,
-1.00000000191613E-6),.UNSPECIFIED.);
#807=B_SPLINE_CURVE_WITH_KNOTS('',3,(#36473,#36474,#36475,#36476,#36477,
#36478),.UNSPECIFIED.,.F.,.F.,(4,2,4),(-3.11031182562015,-1.55397466140411,
-1.00000000147205E-6),.UNSPECIFIED.);
#808=B_SPLINE_CURVE_WITH_KNOTS('',3,(#36480,#36481,#36482,#36483,#36484,
#36485,#36486,#36487,#36488,#36489),.UNSPECIFIED.,.F.,.F.,(4,2,2,2,4),(9.99999995076136E-7,
0.975019785302952,2.07352619778527,3.13207700287592,4.16223066592085),
 .UNSPECIFIED.);
#809=B_SPLINE_CURVE_WITH_KNOTS('',3,(#36490,#36491,#36492,#36493,#36494,
#36495,#36496,#36497,#36498,#36499,#36500,#36501,#36502,#36503,#36504,#36505,
#36506,#36507,#36508,#36509,#36510,#36511,#36512,#36513,#36514),
 .UNSPECIFIED.,.F.,.F.,(4,3,3,3,3,3,3,3,4),(0.169188762886294,0.212591956720561,
0.318887932838093,0.389751920511184,0.460615908147183,0.566911889469088,
0.637775876850632,0.708639855735204,0.737840512980669),.UNSPECIFIED.);
#810=B_SPLINE_CURVE_WITH_KNOTS('',3,(#36788,#36789,#36790,#36791,#36792,
#36793,#36794,#36795),.UNSPECIFIED.,.F.,.F.,(4,2,2,4),(9.64894430459731E-7,
1.95229950803543,2.90453965820021,3.79841482198824),.UNSPECIFIED.);
#811=B_SPLINE_CURVE_WITH_KNOTS('',3,(#36796,#36797,#36798,#36799,#36800,
#36801),.UNSPECIFIED.,.F.,.F.,(4,2,4),(-3.04622791888258,-1.52235182247563,
-1.00000000102796E-6),.UNSPECIFIED.);
#812=B_SPLINE_CURVE_WITH_KNOTS('',3,(#37184,#37185,#37186,#37187,#37188,
#37189),.UNSPECIFIED.,.F.,.F.,(4,2,4),(-3.11031182562016,-1.55397466140411,
-1.00000000102796E-6),.UNSPECIFIED.);
#813=B_SPLINE_CURVE_WITH_KNOTS('',3,(#37191,#37192,#37193,#37194,#37195,
#37196,#37197,#37198,#37199,#37200),.UNSPECIFIED.,.F.,.F.,(4,2,2,2,4),(9.99999995482632E-7,
0.975020551048628,2.07352669960854,3.13207725037628,4.16223066592066),
 .UNSPECIFIED.);
#814=B_SPLINE_CURVE_WITH_KNOTS('',3,(#37201,#37202,#37203,#37204,#37205,
#37206,#37207,#37208,#37209,#37210,#37211,#37212,#37213,#37214,#37215,#37216,
#37217,#37218,#37219,#37220,#37221,#37222,#37223,#37224,#37225),
 .UNSPECIFIED.,.F.,.F.,(4,3,3,3,3,3,3,3,4),(0.169188762886294,0.212591956720561,
0.318887932838093,0.389751920511185,0.460615908147183,0.566911889469088,
0.637775876850632,0.708639855735204,0.737840512980669),.UNSPECIFIED.);
#815=B_SPLINE_CURVE_WITH_KNOTS('',3,(#37499,#37500,#37501,#37502,#37503,
#37504,#37505,#37506),.UNSPECIFIED.,.F.,.F.,(4,2,2,4),(9.64894430661712E-7,
1.95229950804045,2.90453965820967,3.7984148220019),.UNSPECIFIED.);
#816=B_SPLINE_CURVE_WITH_KNOTS('',3,(#37507,#37508,#37509,#37510,#37511,
#37512),.UNSPECIFIED.,.F.,.F.,(4,2,4),(-3.04622791888259,-1.52235182247564,
-1.00000000147205E-6),.UNSPECIFIED.);
#817=CONICAL_SURFACE('',#11750,54.5,0.785398163397448);
#818=CONICAL_SURFACE('',#11761,54.5,0.785398163397448);
#819=CONICAL_SURFACE('',#11812,54.5,0.785398163397448);
#820=CONICAL_SURFACE('',#11898,48.4375,0.785398163397453);
#821=CONICAL_SURFACE('',#11922,48.4375,0.785398163397453);
#822=CONICAL_SURFACE('',#11927,54.5,0.785398163397448);
#823=CONICAL_SURFACE('',#11937,49.6875,0.785398163397442);
#824=CONICAL_SURFACE('',#11941,49.6875,0.785398163397442);
#825=CONICAL_SURFACE('',#11984,53.4375,0.785398163397454);
#826=CONICAL_SURFACE('',#12025,48.4375,0.785398163397453);
#827=CONICAL_SURFACE('',#12035,48.4375,0.785398163397453);
#828=CONICAL_SURFACE('',#12043,49.6875,0.785398163397442);
#829=CONICAL_SURFACE('',#12064,53.4375,0.785398163397454);
#830=CONICAL_SURFACE('',#12100,48.4375,0.785398163397453);
#831=CONICAL_SURFACE('',#12110,48.4375,0.785398163397453);
#832=CONICAL_SURFACE('',#12116,49.6875,0.785398163397442);
#833=CONICAL_SURFACE('',#12127,53.4375,0.785398163397454);
#834=CONICAL_SURFACE('',#12164,48.4375,0.785398163397453);
#835=CONICAL_SURFACE('',#12174,48.4375,0.785398163397453);
#836=CONICAL_SURFACE('',#12194,53.4375,0.785398163397454);
#837=TOROIDAL_SURFACE('',#11536,3.125,0.3125);
#838=TOROIDAL_SURFACE('',#11541,3.125,0.3125);
#839=TOROIDAL_SURFACE('',#11546,3.125,0.3125);
#840=TOROIDAL_SURFACE('',#11550,3.125,0.3125);
#841=TOROIDAL_SURFACE('',#11555,0.625,0.3125);
#842=TOROIDAL_SURFACE('',#11560,4.6875,0.3125);
#843=TOROIDAL_SURFACE('',#11565,1.25,0.3125);
#844=TOROIDAL_SURFACE('',#11570,4.0625,0.3125);
#845=TOROIDAL_SURFACE('',#11575,3.125,0.3125);
#846=TOROIDAL_SURFACE('',#11580,3.125,0.3125);
#847=TOROIDAL_SURFACE('',#11585,3.125,0.3125);
#848=TOROIDAL_SURFACE('',#11590,3.125,0.3125);
#849=TOROIDAL_SURFACE('',#11595,0.625,0.3125);
#850=TOROIDAL_SURFACE('',#11600,4.6875,0.3125);
#851=TOROIDAL_SURFACE('',#11605,1.25,0.3125);
#852=TOROIDAL_SURFACE('',#11610,4.0625,0.3125);
#853=TOROIDAL_SURFACE('',#11615,3.125,0.3125);
#854=TOROIDAL_SURFACE('',#11619,3.125,0.3125);
#855=TOROIDAL_SURFACE('',#11623,3.125,0.3125);
#856=TOROIDAL_SURFACE('',#11628,3.125,0.3125);
#857=TOROIDAL_SURFACE('',#11632,0.625,0.3125);
#858=TOROIDAL_SURFACE('',#11637,1.25,0.3125);
#859=TOROIDAL_SURFACE('',#11642,3.125,0.3125);
#860=TOROIDAL_SURFACE('',#11647,3.125,0.3125);
#861=TOROIDAL_SURFACE('',#11652,3.125,0.3125);
#862=TOROIDAL_SURFACE('',#11657,3.125,0.3125);
#863=TOROIDAL_SURFACE('',#11662,50.,0.3125);
#864=TOROIDAL_SURFACE('',#11667,50.,0.3125);
#865=TOROIDAL_SURFACE('',#11672,1.25,0.3125);
#866=TOROIDAL_SURFACE('',#11677,1.25,0.3125);
#867=TOROIDAL_SURFACE('',#11682,1.25,0.3125);
#868=TOROIDAL_SURFACE('',#11687,1.25,0.3125);
#869=TOROIDAL_SURFACE('',#11701,0.625,0.3125);
#870=TOROIDAL_SURFACE('',#11717,0.625,0.3125);
#871=TOROIDAL_SURFACE('',#11722,0.625,0.3125);
#872=TOROIDAL_SURFACE('',#11727,1.25,0.3125);
#873=TOROIDAL_SURFACE('',#12228,4.0625,0.3125);
#874=TOROIDAL_SURFACE('',#12230,1.25,0.3125);
#875=TOROIDAL_SURFACE('',#12236,1.25,0.3125);
#876=TOROIDAL_SURFACE('',#12238,1.25,0.3125);
#877=TOROIDAL_SURFACE('',#12240,54.6875,0.3125);
#878=TOROIDAL_SURFACE('',#12241,4.6875,0.3125);
#879=TOROIDAL_SURFACE('',#12243,0.625,0.3125);
#880=TOROIDAL_SURFACE('',#12249,0.625,0.3125);
#881=TOROIDAL_SURFACE('',#12251,0.625,0.3125);
#882=TOROIDAL_SURFACE('',#12253,55.3125,0.3125);
#883=TOROIDAL_SURFACE('',#12260,55.4955582617584,0.3125);
#884=TOROIDAL_SURFACE('',#12266,48.75,0.3125);
#885=TOROIDAL_SURFACE('',#12279,57.3169417382416,0.3125);
#886=TOROIDAL_SURFACE('',#12283,48.75,0.3125);
#887=TOROIDAL_SURFACE('',#12289,55.4955582617584,0.3125);
#888=TOROIDAL_SURFACE('',#12292,48.75,0.3125);
#889=TOROIDAL_SURFACE('',#12295,57.3169417382416,0.3125);
#890=TOROIDAL_SURFACE('',#12311,48.75,0.3125);
#891=TOROIDAL_SURFACE('',#12314,21.5625,0.3125);
#892=TOROIDAL_SURFACE('',#12318,48.75,0.3125);
#893=TOROIDAL_SURFACE('',#12321,57.3169417382416,0.3125);
#894=TOROIDAL_SURFACE('',#12329,55.4955582617584,0.3125);
#895=TOROIDAL_SURFACE('',#12334,57.3169417382416,0.3125);
#896=TOROIDAL_SURFACE('',#12338,48.75,0.3125);
#897=TOROIDAL_SURFACE('',#12348,48.125,0.3125);
#898=TOROIDAL_SURFACE('',#12357,55.4955582617584,0.3125);
#899=TOROIDAL_SURFACE('',#12363,48.75,0.3125);
#900=TOROIDAL_SURFACE('',#12366,0.625,0.3125);
#901=TOROIDAL_SURFACE('',#12368,21.5625,0.3125);
#902=TOROIDAL_SURFACE('',#12373,55.4955582617584,0.3125);
#903=TOROIDAL_SURFACE('',#12377,48.75,0.3125);
#904=TOROIDAL_SURFACE('',#12388,21.5625,0.3125);
#905=TOROIDAL_SURFACE('',#12392,0.625,0.3125);
#906=TOROIDAL_SURFACE('',#12399,57.3169417382416,0.3125);
#907=TOROIDAL_SURFACE('',#12403,48.75,0.3125);
#908=TOROIDAL_SURFACE('',#12407,21.5625,0.3125);
#909=TOROIDAL_SURFACE('',#12413,48.75,0.3125);
#910=TOROIDAL_SURFACE('',#12414,48.75,0.3125);
#911=TOROIDAL_SURFACE('',#12417,57.3169417382416,0.3125);
#912=TOROIDAL_SURFACE('',#12424,0.625,0.3125);
#913=TOROIDAL_SURFACE('',#12427,21.5625,0.3125);
#914=TOROIDAL_SURFACE('',#12431,48.125,0.3125);
#915=TOROIDAL_SURFACE('',#12439,55.4955582617584,0.3125);
#916=TOROIDAL_SURFACE('',#12442,0.625,0.3125);
#917=TOROIDAL_SURFACE('',#12453,48.125,0.3125);
#918=TOROIDAL_SURFACE('',#12461,48.75,0.3125);
#919=TOROIDAL_SURFACE('',#12464,0.625,0.3125);
#920=TOROIDAL_SURFACE('',#12469,55.4955582617584,0.3125);
#921=TOROIDAL_SURFACE('',#12473,48.75,0.3125);
#922=TOROIDAL_SURFACE('',#12476,21.5625,0.3125);
#923=TOROIDAL_SURFACE('',#12486,21.5625,0.3125);
#924=TOROIDAL_SURFACE('',#12489,57.3169417382416,0.3125);
#925=TOROIDAL_SURFACE('',#12498,48.125,0.3125);
#926=TOROIDAL_SURFACE('',#12501,21.5625,0.3125);
#927=TOROIDAL_SURFACE('',#12505,48.75,0.3125);
#928=TOROIDAL_SURFACE('',#12507,0.625,0.3125);
#929=TOROIDAL_SURFACE('',#12515,57.3169417382416,0.3125);
#930=TOROIDAL_SURFACE('',#12517,48.75,0.3125);
#931=TOROIDAL_SURFACE('',#12522,48.75,0.3125);
#932=TOROIDAL_SURFACE('',#12535,55.4955582617584,0.3125);
#933=TOROIDAL_SURFACE('',#12544,50.,0.3125);
#934=TOROIDAL_SURFACE('',#12546,50.8794417382416,0.3125);
#935=TOROIDAL_SURFACE('',#12556,1.25,0.3125);
#936=TOROIDAL_SURFACE('',#12559,50.,0.3125);
#937=TOROIDAL_SURFACE('',#12563,50.8794417382416,0.3125);
#938=TOROIDAL_SURFACE('',#12578,5.3125,0.3125);
#939=TOROIDAL_SURFACE('',#12584,54.6294417382416,0.3125);
#940=TOROIDAL_SURFACE('',#12592,50.8794417382416,0.3125);
#941=TOROIDAL_SURFACE('',#12600,1.25,0.3125);
#942=TOROIDAL_SURFACE('',#12602,5.3125,0.3125);
#943=TOROIDAL_SURFACE('',#12613,54.6294417382416,0.3125);
#944=TOROIDAL_SURFACE('',#12617,50.8794417382416,0.3125);
#945=TOROIDAL_SURFACE('',#12622,50.,0.3125);
#946=TOROIDAL_SURFACE('',#12630,5.3125,0.3125);
#947=TOROIDAL_SURFACE('',#12642,54.6294417382416,0.3125);
#948=TOROIDAL_SURFACE('',#12654,50.8794417382416,0.3125);
#949=TOROIDAL_SURFACE('',#12660,50.,0.3125);
#950=TOROIDAL_SURFACE('',#12663,5.3125,0.3125);
#951=TOROIDAL_SURFACE('',#12672,5.3125,0.3125);
#952=TOROIDAL_SURFACE('',#12681,54.6294417382416,0.3125);
#953=TOROIDAL_SURFACE('',#12685,50.,0.3125);
#954=TOROIDAL_SURFACE('',#12690,50.8794417382416,0.3125);
#955=TOROIDAL_SURFACE('',#12698,54.6294417382416,0.3125);
#956=TOROIDAL_SURFACE('',#12708,5.3125,0.3125);
#957=TOROIDAL_SURFACE('',#12716,50.,0.3125);
#958=TOROIDAL_SURFACE('',#12724,50.8794417382416,0.3125);
#959=TOROIDAL_SURFACE('',#12730,5.3125,0.3125);
#960=TOROIDAL_SURFACE('',#12737,1.25,0.3125);
#961=TOROIDAL_SURFACE('',#12743,54.6294417382416,0.3125);
#962=TOROIDAL_SURFACE('',#12748,50.8794417382416,0.3125);
#963=TOROIDAL_SURFACE('',#12754,54.6294417382416,0.3125);
#964=TOROIDAL_SURFACE('',#12757,5.3125,0.3125);
#965=TOROIDAL_SURFACE('',#12777,1.25,0.3125);
#966=TOROIDAL_SURFACE('',#12782,54.6294417382416,0.3125);
#967=TOROIDAL_SURFACE('',#12800,53.5669417382416,0.3125);
#968=TOROIDAL_SURFACE('',#12805,53.5669417382416,0.3125);
#969=TOROIDAL_SURFACE('',#12809,48.75,0.3125);
#970=TOROIDAL_SURFACE('',#12810,48.75,0.3125);
#971=TOROIDAL_SURFACE('',#12811,53.5669417382416,0.3125);
#972=TOROIDAL_SURFACE('',#12818,48.75,0.3125);
#973=TOROIDAL_SURFACE('',#12819,48.75,0.3125);
#974=TOROIDAL_SURFACE('',#12822,53.5669417382416,0.3125);
#975=TOROIDAL_SURFACE('',#12825,5.3125,0.3125);
#976=TOROIDAL_SURFACE('',#12832,5.3125,0.3125);
#977=TOROIDAL_SURFACE('',#12834,5.3125,0.3125);
#978=TOROIDAL_SURFACE('',#12840,5.3125,0.3125);
#979=TOROIDAL_SURFACE('',#12841,5.3125,0.3125);
#980=TOROIDAL_SURFACE('',#12848,5.3125,0.3125);
#981=TOROIDAL_SURFACE('',#12850,5.3125,0.3125);
#982=TOROIDAL_SURFACE('',#12856,5.3125,0.3125);
#983=TOROIDAL_SURFACE('',#12857,4.0625,0.3125);
#984=TOROIDAL_SURFACE('',#12859,1.25,0.3125);
#985=TOROIDAL_SURFACE('',#12866,1.25,0.3125);
#986=TOROIDAL_SURFACE('',#12868,1.25,0.3125);
#987=TOROIDAL_SURFACE('',#12870,54.6875,0.3125);
#988=TOROIDAL_SURFACE('',#12871,4.6875,0.3125);
#989=TOROIDAL_SURFACE('',#12873,0.625,0.3125);
#990=TOROIDAL_SURFACE('',#12880,0.625,0.3125);
#991=TOROIDAL_SURFACE('',#12882,0.625,0.3125);
#992=TOROIDAL_SURFACE('',#12884,55.3125,0.3125);
#993=TOROIDAL_SURFACE('',#12885,1.25,0.3125);
#994=TOROIDAL_SURFACE('',#12887,1.25,0.3125);
#995=TOROIDAL_SURFACE('',#12892,1.25,0.3125);
#996=TOROIDAL_SURFACE('',#12894,54.6875,0.3125);
#997=TOROIDAL_SURFACE('',#12895,0.625,0.3125);
#998=TOROIDAL_SURFACE('',#12897,0.625,0.3125);
#999=TOROIDAL_SURFACE('',#12902,0.625,0.3125);
#1000=TOROIDAL_SURFACE('',#12904,55.3125,0.3125);
#1001=TOROIDAL_SURFACE('',#12905,1.25,0.3125);
#1002=TOROIDAL_SURFACE('',#12907,1.25,0.3125);
#1003=TOROIDAL_SURFACE('',#12912,1.25,0.3125);
#1004=TOROIDAL_SURFACE('',#12914,54.6875,0.3125);
#1005=TOROIDAL_SURFACE('',#12915,0.625,0.3125);
#1006=TOROIDAL_SURFACE('',#12917,0.625,0.3125);
#1007=TOROIDAL_SURFACE('',#12922,0.625,0.3125);
#1008=TOROIDAL_SURFACE('',#12924,55.3125,0.3125);
#1009=TOROIDAL_SURFACE('',#12961,6.25,2.5);
#1010=TOROIDAL_SURFACE('',#12968,18.75,1.25);
#1011=TOROIDAL_SURFACE('',#12975,19.375,2.5);
#1012=FACE_OUTER_BOUND('',#1759,.T.);
#1013=FACE_OUTER_BOUND('',#1760,.T.);
#1014=FACE_OUTER_BOUND('',#1761,.T.);
#1015=FACE_OUTER_BOUND('',#1762,.T.);
#1016=FACE_OUTER_BOUND('',#1763,.T.);
#1017=FACE_OUTER_BOUND('',#1764,.T.);
#1018=FACE_OUTER_BOUND('',#1765,.T.);
#1019=FACE_OUTER_BOUND('',#1766,.T.);
#1020=FACE_OUTER_BOUND('',#1767,.T.);
#1021=FACE_OUTER_BOUND('',#1768,.T.);
#1022=FACE_OUTER_BOUND('',#1769,.T.);
#1023=FACE_OUTER_BOUND('',#1770,.T.);
#1024=FACE_OUTER_BOUND('',#1771,.T.);
#1025=FACE_OUTER_BOUND('',#1772,.T.);
#1026=FACE_OUTER_BOUND('',#1773,.T.);
#1027=FACE_OUTER_BOUND('',#1774,.T.);
#1028=FACE_OUTER_BOUND('',#1775,.T.);
#1029=FACE_OUTER_BOUND('',#1776,.T.);
#1030=FACE_OUTER_BOUND('',#1777,.T.);
#1031=FACE_OUTER_BOUND('',#1778,.T.);
#1032=FACE_OUTER_BOUND('',#1779,.T.);
#1033=FACE_OUTER_BOUND('',#1780,.T.);
#1034=FACE_OUTER_BOUND('',#1781,.T.);
#1035=FACE_OUTER_BOUND('',#1782,.T.);
#1036=FACE_OUTER_BOUND('',#1783,.T.);
#1037=FACE_OUTER_BOUND('',#1784,.T.);
#1038=FACE_OUTER_BOUND('',#1785,.T.);
#1039=FACE_OUTER_BOUND('',#1786,.T.);
#1040=FACE_OUTER_BOUND('',#1787,.T.);
#1041=FACE_OUTER_BOUND('',#1788,.T.);
#1042=FACE_OUTER_BOUND('',#1789,.T.);
#1043=FACE_OUTER_BOUND('',#1790,.T.);
#1044=FACE_OUTER_BOUND('',#1791,.T.);
#1045=FACE_OUTER_BOUND('',#1792,.T.);
#1046=FACE_OUTER_BOUND('',#1793,.T.);
#1047=FACE_OUTER_BOUND('',#1794,.T.);
#1048=FACE_OUTER_BOUND('',#1795,.T.);
#1049=FACE_OUTER_BOUND('',#1796,.T.);
#1050=FACE_OUTER_BOUND('',#1797,.T.);
#1051=FACE_OUTER_BOUND('',#1798,.T.);
#1052=FACE_OUTER_BOUND('',#1799,.T.);
#1053=FACE_OUTER_BOUND('',#1800,.T.);
#1054=FACE_OUTER_BOUND('',#1801,.T.);
#1055=FACE_OUTER_BOUND('',#1802,.T.);
#1056=FACE_OUTER_BOUND('',#1803,.T.);
#1057=FACE_OUTER_BOUND('',#1804,.T.);
#1058=FACE_OUTER_BOUND('',#1805,.T.);
#1059=FACE_OUTER_BOUND('',#1806,.T.);
#1060=FACE_OUTER_BOUND('',#1807,.T.);
#1061=FACE_OUTER_BOUND('',#1808,.T.);
#1062=FACE_OUTER_BOUND('',#1809,.T.);
#1063=FACE_OUTER_BOUND('',#1810,.T.);
#1064=FACE_OUTER_BOUND('',#1811,.T.);
#1065=FACE_OUTER_BOUND('',#1812,.T.);
#1066=FACE_OUTER_BOUND('',#1813,.T.);
#1067=FACE_OUTER_BOUND('',#1814,.T.);
#1068=FACE_OUTER_BOUND('',#1815,.T.);
#1069=FACE_OUTER_BOUND('',#1816,.T.);
#1070=FACE_OUTER_BOUND('',#1817,.T.);
#1071=FACE_OUTER_BOUND('',#1818,.T.);
#1072=FACE_OUTER_BOUND('',#1819,.T.);
#1073=FACE_OUTER_BOUND('',#1820,.T.);
#1074=FACE_OUTER_BOUND('',#1821,.T.);
#1075=FACE_OUTER_BOUND('',#1822,.T.);
#1076=FACE_OUTER_BOUND('',#1823,.T.);
#1077=FACE_OUTER_BOUND('',#1824,.T.);
#1078=FACE_OUTER_BOUND('',#1825,.T.);
#1079=FACE_OUTER_BOUND('',#1826,.T.);
#1080=FACE_OUTER_BOUND('',#1827,.T.);
#1081=FACE_OUTER_BOUND('',#1828,.T.);
#1082=FACE_OUTER_BOUND('',#1829,.T.);
#1083=FACE_OUTER_BOUND('',#1830,.T.);
#1084=FACE_OUTER_BOUND('',#1831,.T.);
#1085=FACE_OUTER_BOUND('',#1840,.T.);
#1086=FACE_OUTER_BOUND('',#1841,.T.);
#1087=FACE_OUTER_BOUND('',#1842,.T.);
#1088=FACE_OUTER_BOUND('',#1844,.T.);
#1089=FACE_OUTER_BOUND('',#1846,.T.);
#1090=FACE_OUTER_BOUND('',#1847,.T.);
#1091=FACE_OUTER_BOUND('',#1848,.T.);
#1092=FACE_OUTER_BOUND('',#1849,.T.);
#1093=FACE_OUTER_BOUND('',#1850,.T.);
#1094=FACE_OUTER_BOUND('',#1851,.T.);
#1095=FACE_OUTER_BOUND('',#1852,.T.);
#1096=FACE_OUTER_BOUND('',#1853,.T.);
#1097=FACE_OUTER_BOUND('',#1854,.T.);
#1098=FACE_OUTER_BOUND('',#1855,.T.);
#1099=FACE_OUTER_BOUND('',#1856,.T.);
#1100=FACE_OUTER_BOUND('',#1858,.T.);
#1101=FACE_OUTER_BOUND('',#1859,.T.);
#1102=FACE_OUTER_BOUND('',#1860,.T.);
#1103=FACE_OUTER_BOUND('',#1861,.T.);
#1104=FACE_OUTER_BOUND('',#1862,.T.);
#1105=FACE_OUTER_BOUND('',#1863,.T.);
#1106=FACE_OUTER_BOUND('',#1864,.T.);
#1107=FACE_OUTER_BOUND('',#1865,.T.);
#1108=FACE_OUTER_BOUND('',#1866,.T.);
#1109=FACE_OUTER_BOUND('',#1867,.T.);
#1110=FACE_OUTER_BOUND('',#1868,.T.);
#1111=FACE_OUTER_BOUND('',#1869,.T.);
#1112=FACE_OUTER_BOUND('',#1870,.T.);
#1113=FACE_OUTER_BOUND('',#1871,.T.);
#1114=FACE_OUTER_BOUND('',#1872,.T.);
#1115=FACE_OUTER_BOUND('',#1874,.T.);
#1116=FACE_OUTER_BOUND('',#1876,.T.);
#1117=FACE_OUTER_BOUND('',#1877,.T.);
#1118=FACE_OUTER_BOUND('',#1878,.T.);
#1119=FACE_OUTER_BOUND('',#1879,.T.);
#1120=FACE_OUTER_BOUND('',#1880,.T.);
#1121=FACE_OUTER_BOUND('',#1881,.T.);
#1122=FACE_OUTER_BOUND('',#1890,.T.);
#1123=FACE_OUTER_BOUND('',#1891,.T.);
#1124=FACE_OUTER_BOUND('',#1892,.T.);
#1125=FACE_OUTER_BOUND('',#1893,.T.);
#1126=FACE_OUTER_BOUND('',#1894,.T.);
#1127=FACE_OUTER_BOUND('',#1895,.T.);
#1128=FACE_OUTER_BOUND('',#1896,.T.);
#1129=FACE_OUTER_BOUND('',#1897,.T.);
#1130=FACE_OUTER_BOUND('',#1898,.T.);
#1131=FACE_OUTER_BOUND('',#1899,.T.);
#1132=FACE_OUTER_BOUND('',#1900,.T.);
#1133=FACE_OUTER_BOUND('',#1901,.T.);
#1134=FACE_OUTER_BOUND('',#1902,.T.);
#1135=FACE_OUTER_BOUND('',#1903,.T.);
#1136=FACE_OUTER_BOUND('',#1904,.T.);
#1137=FACE_OUTER_BOUND('',#1905,.T.);
#1138=FACE_OUTER_BOUND('',#1906,.T.);
#1139=FACE_OUTER_BOUND('',#1907,.T.);
#1140=FACE_OUTER_BOUND('',#1908,.T.);
#1141=FACE_OUTER_BOUND('',#1909,.T.);
#1142=FACE_OUTER_BOUND('',#1910,.T.);
#1143=FACE_OUTER_BOUND('',#1911,.T.);
#1144=FACE_OUTER_BOUND('',#1912,.T.);
#1145=FACE_OUTER_BOUND('',#1913,.T.);
#1146=FACE_OUTER_BOUND('',#1914,.T.);
#1147=FACE_OUTER_BOUND('',#1916,.T.);
#1148=FACE_OUTER_BOUND('',#1918,.T.);
#1149=FACE_OUTER_BOUND('',#1919,.T.);
#1150=FACE_OUTER_BOUND('',#1920,.T.);
#1151=FACE_OUTER_BOUND('',#1921,.T.);
#1152=FACE_OUTER_BOUND('',#1922,.T.);
#1153=FACE_OUTER_BOUND('',#1923,.T.);
#1154=FACE_OUTER_BOUND('',#1924,.T.);
#1155=FACE_OUTER_BOUND('',#1925,.T.);
#1156=FACE_OUTER_BOUND('',#1926,.T.);
#1157=FACE_OUTER_BOUND('',#1927,.T.);
#1158=FACE_OUTER_BOUND('',#1928,.T.);
#1159=FACE_OUTER_BOUND('',#1929,.T.);
#1160=FACE_OUTER_BOUND('',#1930,.T.);
#1161=FACE_OUTER_BOUND('',#1931,.T.);
#1162=FACE_OUTER_BOUND('',#1932,.T.);
#1163=FACE_OUTER_BOUND('',#1933,.T.);
#1164=FACE_OUTER_BOUND('',#1934,.T.);
#1165=FACE_OUTER_BOUND('',#1935,.T.);
#1166=FACE_OUTER_BOUND('',#1936,.T.);
#1167=FACE_OUTER_BOUND('',#1937,.T.);
#1168=FACE_OUTER_BOUND('',#1938,.T.);
#1169=FACE_OUTER_BOUND('',#1939,.T.);
#1170=FACE_OUTER_BOUND('',#1940,.T.);
#1171=FACE_OUTER_BOUND('',#1941,.T.);
#1172=FACE_OUTER_BOUND('',#1942,.T.);
#1173=FACE_OUTER_BOUND('',#1943,.T.);
#1174=FACE_OUTER_BOUND('',#1944,.T.);
#1175=FACE_OUTER_BOUND('',#1945,.T.);
#1176=FACE_OUTER_BOUND('',#1946,.T.);
#1177=FACE_OUTER_BOUND('',#1947,.T.);
#1178=FACE_OUTER_BOUND('',#1948,.T.);
#1179=FACE_OUTER_BOUND('',#1949,.T.);
#1180=FACE_OUTER_BOUND('',#1950,.T.);
#1181=FACE_OUTER_BOUND('',#1951,.T.);
#1182=FACE_OUTER_BOUND('',#1952,.T.);
#1183=FACE_OUTER_BOUND('',#1953,.T.);
#1184=FACE_OUTER_BOUND('',#1954,.T.);
#1185=FACE_OUTER_BOUND('',#1955,.T.);
#1186=FACE_OUTER_BOUND('',#1956,.T.);
#1187=FACE_OUTER_BOUND('',#1957,.T.);
#1188=FACE_OUTER_BOUND('',#1958,.T.);
#1189=FACE_OUTER_BOUND('',#1959,.T.);
#1190=FACE_OUTER_BOUND('',#1960,.T.);
#1191=FACE_OUTER_BOUND('',#1961,.T.);
#1192=FACE_OUTER_BOUND('',#1962,.T.);
#1193=FACE_OUTER_BOUND('',#1963,.T.);
#1194=FACE_OUTER_BOUND('',#1964,.T.);
#1195=FACE_OUTER_BOUND('',#1965,.T.);
#1196=FACE_OUTER_BOUND('',#1966,.T.);
#1197=FACE_OUTER_BOUND('',#1967,.T.);
#1198=FACE_OUTER_BOUND('',#1968,.T.);
#1199=FACE_OUTER_BOUND('',#1970,.T.);
#1200=FACE_OUTER_BOUND('',#1972,.T.);
#1201=FACE_OUTER_BOUND('',#1973,.T.);
#1202=FACE_OUTER_BOUND('',#1974,.T.);
#1203=FACE_OUTER_BOUND('',#1975,.T.);
#1204=FACE_OUTER_BOUND('',#1976,.T.);
#1205=FACE_OUTER_BOUND('',#1977,.T.);
#1206=FACE_OUTER_BOUND('',#1978,.T.);
#1207=FACE_OUTER_BOUND('',#1979,.T.);
#1208=FACE_OUTER_BOUND('',#1980,.T.);
#1209=FACE_OUTER_BOUND('',#1981,.T.);
#1210=FACE_OUTER_BOUND('',#1982,.T.);
#1211=FACE_OUTER_BOUND('',#1983,.T.);
#1212=FACE_OUTER_BOUND('',#1984,.T.);
#1213=FACE_OUTER_BOUND('',#1985,.T.);
#1214=FACE_OUTER_BOUND('',#1986,.T.);
#1215=FACE_OUTER_BOUND('',#1987,.T.);
#1216=FACE_OUTER_BOUND('',#1988,.T.);
#1217=FACE_OUTER_BOUND('',#1989,.T.);
#1218=FACE_OUTER_BOUND('',#1990,.T.);
#1219=FACE_OUTER_BOUND('',#1991,.T.);
#1220=FACE_OUTER_BOUND('',#1992,.T.);
#1221=FACE_OUTER_BOUND('',#1993,.T.);
#1222=FACE_OUTER_BOUND('',#1994,.T.);
#1223=FACE_OUTER_BOUND('',#1995,.T.);
#1224=FACE_OUTER_BOUND('',#1996,.T.);
#1225=FACE_OUTER_BOUND('',#1997,.T.);
#1226=FACE_OUTER_BOUND('',#1998,.T.);
#1227=FACE_OUTER_BOUND('',#1999,.T.);
#1228=FACE_OUTER_BOUND('',#2000,.T.);
#1229=FACE_OUTER_BOUND('',#2001,.T.);
#1230=FACE_OUTER_BOUND('',#2002,.T.);
#1231=FACE_OUTER_BOUND('',#2003,.T.);
#1232=FACE_OUTER_BOUND('',#2004,.T.);
#1233=FACE_OUTER_BOUND('',#2005,.T.);
#1234=FACE_OUTER_BOUND('',#2006,.T.);
#1235=FACE_OUTER_BOUND('',#2007,.T.);
#1236=FACE_OUTER_BOUND('',#2008,.T.);
#1237=FACE_OUTER_BOUND('',#2009,.T.);
#1238=FACE_OUTER_BOUND('',#2010,.T.);
#1239=FACE_OUTER_BOUND('',#2011,.T.);
#1240=FACE_OUTER_BOUND('',#2012,.T.);
#1241=FACE_OUTER_BOUND('',#2013,.T.);
#1242=FACE_OUTER_BOUND('',#2014,.T.);
#1243=FACE_OUTER_BOUND('',#2015,.T.);
#1244=FACE_OUTER_BOUND('',#2016,.T.);
#1245=FACE_OUTER_BOUND('',#2017,.T.);
#1246=FACE_OUTER_BOUND('',#2018,.T.);
#1247=FACE_OUTER_BOUND('',#2019,.T.);
#1248=FACE_OUTER_BOUND('',#2020,.T.);
#1249=FACE_OUTER_BOUND('',#2021,.T.);
#1250=FACE_OUTER_BOUND('',#2022,.T.);
#1251=FACE_OUTER_BOUND('',#2023,.T.);
#1252=FACE_OUTER_BOUND('',#2024,.T.);
#1253=FACE_OUTER_BOUND('',#2025,.T.);
#1254=FACE_OUTER_BOUND('',#2026,.T.);
#1255=FACE_OUTER_BOUND('',#2027,.T.);
#1256=FACE_OUTER_BOUND('',#2028,.T.);
#1257=FACE_OUTER_BOUND('',#2029,.T.);
#1258=FACE_OUTER_BOUND('',#2030,.T.);
#1259=FACE_OUTER_BOUND('',#2031,.T.);
#1260=FACE_OUTER_BOUND('',#2032,.T.);
#1261=FACE_OUTER_BOUND('',#2033,.T.);
#1262=FACE_OUTER_BOUND('',#2034,.T.);
#1263=FACE_OUTER_BOUND('',#2035,.T.);
#1264=FACE_OUTER_BOUND('',#2036,.T.);
#1265=FACE_OUTER_BOUND('',#2037,.T.);
#1266=FACE_OUTER_BOUND('',#2038,.T.);
#1267=FACE_OUTER_BOUND('',#2039,.T.);
#1268=FACE_OUTER_BOUND('',#2040,.T.);
#1269=FACE_OUTER_BOUND('',#2041,.T.);
#1270=FACE_OUTER_BOUND('',#2042,.T.);
#1271=FACE_OUTER_BOUND('',#2043,.T.);
#1272=FACE_OUTER_BOUND('',#2044,.T.);
#1273=FACE_OUTER_BOUND('',#2045,.T.);
#1274=FACE_OUTER_BOUND('',#2046,.T.);
#1275=FACE_OUTER_BOUND('',#2047,.T.);
#1276=FACE_OUTER_BOUND('',#2048,.T.);
#1277=FACE_OUTER_BOUND('',#2049,.T.);
#1278=FACE_OUTER_BOUND('',#2050,.T.);
#1279=FACE_OUTER_BOUND('',#2051,.T.);
#1280=FACE_OUTER_BOUND('',#2052,.T.);
#1281=FACE_OUTER_BOUND('',#2053,.T.);
#1282=FACE_OUTER_BOUND('',#2054,.T.);
#1283=FACE_OUTER_BOUND('',#2055,.T.);
#1284=FACE_OUTER_BOUND('',#2056,.T.);
#1285=FACE_OUTER_BOUND('',#2057,.T.);
#1286=FACE_OUTER_BOUND('',#2058,.T.);
#1287=FACE_OUTER_BOUND('',#2059,.T.);
#1288=FACE_OUTER_BOUND('',#2060,.T.);
#1289=FACE_OUTER_BOUND('',#2061,.T.);
#1290=FACE_OUTER_BOUND('',#2062,.T.);
#1291=FACE_OUTER_BOUND('',#2063,.T.);
#1292=FACE_OUTER_BOUND('',#2064,.T.);
#1293=FACE_OUTER_BOUND('',#2065,.T.);
#1294=FACE_OUTER_BOUND('',#2066,.T.);
#1295=FACE_OUTER_BOUND('',#2067,.T.);
#1296=FACE_OUTER_BOUND('',#2068,.T.);
#1297=FACE_OUTER_BOUND('',#2069,.T.);
#1298=FACE_OUTER_BOUND('',#2070,.T.);
#1299=FACE_OUTER_BOUND('',#2071,.T.);
#1300=FACE_OUTER_BOUND('',#2072,.T.);
#1301=FACE_OUTER_BOUND('',#2073,.T.);
#1302=FACE_OUTER_BOUND('',#2074,.T.);
#1303=FACE_OUTER_BOUND('',#2075,.T.);
#1304=FACE_OUTER_BOUND('',#2076,.T.);
#1305=FACE_OUTER_BOUND('',#2077,.T.);
#1306=FACE_OUTER_BOUND('',#2078,.T.);
#1307=FACE_OUTER_BOUND('',#2079,.T.);
#1308=FACE_OUTER_BOUND('',#2080,.T.);
#1309=FACE_OUTER_BOUND('',#2081,.T.);
#1310=FACE_OUTER_BOUND('',#2082,.T.);
#1311=FACE_OUTER_BOUND('',#2083,.T.);
#1312=FACE_OUTER_BOUND('',#2084,.T.);
#1313=FACE_OUTER_BOUND('',#2085,.T.);
#1314=FACE_OUTER_BOUND('',#2086,.T.);
#1315=FACE_OUTER_BOUND('',#2087,.T.);
#1316=FACE_OUTER_BOUND('',#2088,.T.);
#1317=FACE_OUTER_BOUND('',#2089,.T.);
#1318=FACE_OUTER_BOUND('',#2090,.T.);
#1319=FACE_OUTER_BOUND('',#2091,.T.);
#1320=FACE_OUTER_BOUND('',#2092,.T.);
#1321=FACE_OUTER_BOUND('',#2093,.T.);
#1322=FACE_OUTER_BOUND('',#2094,.T.);
#1323=FACE_OUTER_BOUND('',#2095,.T.);
#1324=FACE_OUTER_BOUND('',#2096,.T.);
#1325=FACE_OUTER_BOUND('',#2097,.T.);
#1326=FACE_OUTER_BOUND('',#2098,.T.);
#1327=FACE_OUTER_BOUND('',#2099,.T.);
#1328=FACE_OUTER_BOUND('',#2100,.T.);
#1329=FACE_OUTER_BOUND('',#2101,.T.);
#1330=FACE_OUTER_BOUND('',#2102,.T.);
#1331=FACE_OUTER_BOUND('',#2103,.T.);
#1332=FACE_OUTER_BOUND('',#2104,.T.);
#1333=FACE_OUTER_BOUND('',#2105,.T.);
#1334=FACE_OUTER_BOUND('',#2106,.T.);
#1335=FACE_OUTER_BOUND('',#2107,.T.);
#1336=FACE_OUTER_BOUND('',#2108,.T.);
#1337=FACE_OUTER_BOUND('',#2109,.T.);
#1338=FACE_OUTER_BOUND('',#2110,.T.);
#1339=FACE_OUTER_BOUND('',#2111,.T.);
#1340=FACE_OUTER_BOUND('',#2112,.T.);
#1341=FACE_OUTER_BOUND('',#2113,.T.);
#1342=FACE_OUTER_BOUND('',#2114,.T.);
#1343=FACE_OUTER_BOUND('',#2115,.T.);
#1344=FACE_OUTER_BOUND('',#2116,.T.);
#1345=FACE_OUTER_BOUND('',#2117,.T.);
#1346=FACE_OUTER_BOUND('',#2118,.T.);
#1347=FACE_OUTER_BOUND('',#2119,.T.);
#1348=FACE_OUTER_BOUND('',#2120,.T.);
#1349=FACE_OUTER_BOUND('',#2121,.T.);
#1350=FACE_OUTER_BOUND('',#2122,.T.);
#1351=FACE_OUTER_BOUND('',#2123,.T.);
#1352=FACE_OUTER_BOUND('',#2124,.T.);
#1353=FACE_OUTER_BOUND('',#2125,.T.);
#1354=FACE_OUTER_BOUND('',#2126,.T.);
#1355=FACE_OUTER_BOUND('',#2127,.T.);
#1356=FACE_OUTER_BOUND('',#2128,.T.);
#1357=FACE_OUTER_BOUND('',#2129,.T.);
#1358=FACE_OUTER_BOUND('',#2130,.T.);
#1359=FACE_OUTER_BOUND('',#2131,.T.);
#1360=FACE_OUTER_BOUND('',#2132,.T.);
#1361=FACE_OUTER_BOUND('',#2133,.T.);
#1362=FACE_OUTER_BOUND('',#2134,.T.);
#1363=FACE_OUTER_BOUND('',#2135,.T.);
#1364=FACE_OUTER_BOUND('',#2136,.T.);
#1365=FACE_OUTER_BOUND('',#2137,.T.);
#1366=FACE_OUTER_BOUND('',#2138,.T.);
#1367=FACE_OUTER_BOUND('',#2139,.T.);
#1368=FACE_OUTER_BOUND('',#2140,.T.);
#1369=FACE_OUTER_BOUND('',#2141,.T.);
#1370=FACE_OUTER_BOUND('',#2142,.T.);
#1371=FACE_OUTER_BOUND('',#2143,.T.);
#1372=FACE_OUTER_BOUND('',#2144,.T.);
#1373=FACE_OUTER_BOUND('',#2145,.T.);
#1374=FACE_OUTER_BOUND('',#2146,.T.);
#1375=FACE_OUTER_BOUND('',#2147,.T.);
#1376=FACE_OUTER_BOUND('',#2148,.T.);
#1377=FACE_OUTER_BOUND('',#2149,.T.);
#1378=FACE_OUTER_BOUND('',#2150,.T.);
#1379=FACE_OUTER_BOUND('',#2151,.T.);
#1380=FACE_OUTER_BOUND('',#2152,.T.);
#1381=FACE_OUTER_BOUND('',#2153,.T.);
#1382=FACE_OUTER_BOUND('',#2154,.T.);
#1383=FACE_OUTER_BOUND('',#2155,.T.);
#1384=FACE_OUTER_BOUND('',#2156,.T.);
#1385=FACE_OUTER_BOUND('',#2157,.T.);
#1386=FACE_OUTER_BOUND('',#2158,.T.);
#1387=FACE_OUTER_BOUND('',#2159,.T.);
#1388=FACE_OUTER_BOUND('',#2160,.T.);
#1389=FACE_OUTER_BOUND('',#2161,.T.);
#1390=FACE_OUTER_BOUND('',#2162,.T.);
#1391=FACE_OUTER_BOUND('',#2163,.T.);
#1392=FACE_OUTER_BOUND('',#2164,.T.);
#1393=FACE_OUTER_BOUND('',#2165,.T.);
#1394=FACE_OUTER_BOUND('',#2166,.T.);
#1395=FACE_OUTER_BOUND('',#2167,.T.);
#1396=FACE_OUTER_BOUND('',#2168,.T.);
#1397=FACE_OUTER_BOUND('',#2169,.T.);
#1398=FACE_OUTER_BOUND('',#2170,.T.);
#1399=FACE_OUTER_BOUND('',#2171,.T.);
#1400=FACE_OUTER_BOUND('',#2172,.T.);
#1401=FACE_OUTER_BOUND('',#2173,.T.);
#1402=FACE_OUTER_BOUND('',#2174,.T.);
#1403=FACE_OUTER_BOUND('',#2175,.T.);
#1404=FACE_OUTER_BOUND('',#2176,.T.);
#1405=FACE_OUTER_BOUND('',#2177,.T.);
#1406=FACE_OUTER_BOUND('',#2178,.T.);
#1407=FACE_OUTER_BOUND('',#2179,.T.);
#1408=FACE_OUTER_BOUND('',#2180,.T.);
#1409=FACE_OUTER_BOUND('',#2181,.T.);
#1410=FACE_OUTER_BOUND('',#2182,.T.);
#1411=FACE_OUTER_BOUND('',#2183,.T.);
#1412=FACE_OUTER_BOUND('',#2184,.T.);
#1413=FACE_OUTER_BOUND('',#2185,.T.);
#1414=FACE_OUTER_BOUND('',#2186,.T.);
#1415=FACE_OUTER_BOUND('',#2187,.T.);
#1416=FACE_OUTER_BOUND('',#2188,.T.);
#1417=FACE_OUTER_BOUND('',#2189,.T.);
#1418=FACE_OUTER_BOUND('',#2190,.T.);
#1419=FACE_OUTER_BOUND('',#2191,.T.);
#1420=FACE_OUTER_BOUND('',#2192,.T.);
#1421=FACE_OUTER_BOUND('',#2193,.T.);
#1422=FACE_OUTER_BOUND('',#2194,.T.);
#1423=FACE_OUTER_BOUND('',#2195,.T.);
#1424=FACE_OUTER_BOUND('',#2196,.T.);
#1425=FACE_OUTER_BOUND('',#2197,.T.);
#1426=FACE_OUTER_BOUND('',#2198,.T.);
#1427=FACE_OUTER_BOUND('',#2199,.T.);
#1428=FACE_OUTER_BOUND('',#2200,.T.);
#1429=FACE_OUTER_BOUND('',#2201,.T.);
#1430=FACE_OUTER_BOUND('',#2202,.T.);
#1431=FACE_OUTER_BOUND('',#2203,.T.);
#1432=FACE_OUTER_BOUND('',#2204,.T.);
#1433=FACE_OUTER_BOUND('',#2205,.T.);
#1434=FACE_OUTER_BOUND('',#2206,.T.);
#1435=FACE_OUTER_BOUND('',#2207,.T.);
#1436=FACE_OUTER_BOUND('',#2208,.T.);
#1437=FACE_OUTER_BOUND('',#2209,.T.);
#1438=FACE_OUTER_BOUND('',#2210,.T.);
#1439=FACE_OUTER_BOUND('',#2211,.T.);
#1440=FACE_OUTER_BOUND('',#2212,.T.);
#1441=FACE_OUTER_BOUND('',#2213,.T.);
#1442=FACE_OUTER_BOUND('',#2214,.T.);
#1443=FACE_OUTER_BOUND('',#2215,.T.);
#1444=FACE_OUTER_BOUND('',#2216,.T.);
#1445=FACE_OUTER_BOUND('',#2217,.T.);
#1446=FACE_OUTER_BOUND('',#2218,.T.);
#1447=FACE_OUTER_BOUND('',#2219,.T.);
#1448=FACE_OUTER_BOUND('',#2220,.T.);
#1449=FACE_OUTER_BOUND('',#2221,.T.);
#1450=FACE_OUTER_BOUND('',#2222,.T.);
#1451=FACE_OUTER_BOUND('',#2223,.T.);
#1452=FACE_OUTER_BOUND('',#2224,.T.);
#1453=FACE_OUTER_BOUND('',#2225,.T.);
#1454=FACE_OUTER_BOUND('',#2226,.T.);
#1455=FACE_OUTER_BOUND('',#2227,.T.);
#1456=FACE_OUTER_BOUND('',#2228,.T.);
#1457=FACE_OUTER_BOUND('',#2229,.T.);
#1458=FACE_OUTER_BOUND('',#2230,.T.);
#1459=FACE_OUTER_BOUND('',#2231,.T.);
#1460=FACE_OUTER_BOUND('',#2232,.T.);
#1461=FACE_OUTER_BOUND('',#2233,.T.);
#1462=FACE_OUTER_BOUND('',#2234,.T.);
#1463=FACE_OUTER_BOUND('',#2235,.T.);
#1464=FACE_OUTER_BOUND('',#2236,.T.);
#1465=FACE_OUTER_BOUND('',#2237,.T.);
#1466=FACE_OUTER_BOUND('',#2238,.T.);
#1467=FACE_OUTER_BOUND('',#2239,.T.);
#1468=FACE_OUTER_BOUND('',#2240,.T.);
#1469=FACE_OUTER_BOUND('',#2241,.T.);
#1470=FACE_OUTER_BOUND('',#2242,.T.);
#1471=FACE_OUTER_BOUND('',#2243,.T.);
#1472=FACE_OUTER_BOUND('',#2244,.T.);
#1473=FACE_OUTER_BOUND('',#2245,.T.);
#1474=FACE_OUTER_BOUND('',#2246,.T.);
#1475=FACE_OUTER_BOUND('',#2247,.T.);
#1476=FACE_OUTER_BOUND('',#2248,.T.);
#1477=FACE_OUTER_BOUND('',#2249,.T.);
#1478=FACE_OUTER_BOUND('',#2250,.T.);
#1479=FACE_OUTER_BOUND('',#2251,.T.);
#1480=FACE_OUTER_BOUND('',#2252,.T.);
#1481=FACE_OUTER_BOUND('',#2253,.T.);
#1482=FACE_OUTER_BOUND('',#2254,.T.);
#1483=FACE_OUTER_BOUND('',#2255,.T.);
#1484=FACE_OUTER_BOUND('',#2256,.T.);
#1485=FACE_OUTER_BOUND('',#2257,.T.);
#1486=FACE_OUTER_BOUND('',#2258,.T.);
#1487=FACE_OUTER_BOUND('',#2259,.T.);
#1488=FACE_OUTER_BOUND('',#2260,.T.);
#1489=FACE_OUTER_BOUND('',#2261,.T.);
#1490=FACE_OUTER_BOUND('',#2262,.T.);
#1491=FACE_OUTER_BOUND('',#2263,.T.);
#1492=FACE_OUTER_BOUND('',#2264,.T.);
#1493=FACE_OUTER_BOUND('',#2265,.T.);
#1494=FACE_OUTER_BOUND('',#2266,.T.);
#1495=FACE_OUTER_BOUND('',#2267,.T.);
#1496=FACE_OUTER_BOUND('',#2268,.T.);
#1497=FACE_OUTER_BOUND('',#2269,.T.);
#1498=FACE_OUTER_BOUND('',#2270,.T.);
#1499=FACE_OUTER_BOUND('',#2271,.T.);
#1500=FACE_OUTER_BOUND('',#2272,.T.);
#1501=FACE_OUTER_BOUND('',#2273,.T.);
#1502=FACE_OUTER_BOUND('',#2274,.T.);
#1503=FACE_OUTER_BOUND('',#2275,.T.);
#1504=FACE_OUTER_BOUND('',#2276,.T.);
#1505=FACE_OUTER_BOUND('',#2277,.T.);
#1506=FACE_OUTER_BOUND('',#2278,.T.);
#1507=FACE_OUTER_BOUND('',#2279,.T.);
#1508=FACE_OUTER_BOUND('',#2280,.T.);
#1509=FACE_OUTER_BOUND('',#2281,.T.);
#1510=FACE_OUTER_BOUND('',#2282,.T.);
#1511=FACE_OUTER_BOUND('',#2283,.T.);
#1512=FACE_OUTER_BOUND('',#2284,.T.);
#1513=FACE_OUTER_BOUND('',#2285,.T.);
#1514=FACE_OUTER_BOUND('',#2286,.T.);
#1515=FACE_OUTER_BOUND('',#2287,.T.);
#1516=FACE_OUTER_BOUND('',#2288,.T.);
#1517=FACE_OUTER_BOUND('',#2289,.T.);
#1518=FACE_OUTER_BOUND('',#2290,.T.);
#1519=FACE_OUTER_BOUND('',#2291,.T.);
#1520=FACE_OUTER_BOUND('',#2292,.T.);
#1521=FACE_OUTER_BOUND('',#2293,.T.);
#1522=FACE_OUTER_BOUND('',#2294,.T.);
#1523=FACE_OUTER_BOUND('',#2295,.T.);
#1524=FACE_OUTER_BOUND('',#2296,.T.);
#1525=FACE_OUTER_BOUND('',#2297,.T.);
#1526=FACE_OUTER_BOUND('',#2298,.T.);
#1527=FACE_OUTER_BOUND('',#2299,.T.);
#1528=FACE_OUTER_BOUND('',#2300,.T.);
#1529=FACE_OUTER_BOUND('',#2301,.T.);
#1530=FACE_OUTER_BOUND('',#2302,.T.);
#1531=FACE_OUTER_BOUND('',#2303,.T.);
#1532=FACE_OUTER_BOUND('',#2304,.T.);
#1533=FACE_OUTER_BOUND('',#2305,.T.);
#1534=FACE_OUTER_BOUND('',#2306,.T.);
#1535=FACE_OUTER_BOUND('',#2307,.T.);
#1536=FACE_OUTER_BOUND('',#2308,.T.);
#1537=FACE_OUTER_BOUND('',#2309,.T.);
#1538=FACE_OUTER_BOUND('',#2310,.T.);
#1539=FACE_OUTER_BOUND('',#2311,.T.);
#1540=FACE_OUTER_BOUND('',#2312,.T.);
#1541=FACE_OUTER_BOUND('',#2313,.T.);
#1542=FACE_OUTER_BOUND('',#2314,.T.);
#1543=FACE_OUTER_BOUND('',#2315,.T.);
#1544=FACE_OUTER_BOUND('',#2316,.T.);
#1545=FACE_OUTER_BOUND('',#2317,.T.);
#1546=FACE_OUTER_BOUND('',#2318,.T.);
#1547=FACE_OUTER_BOUND('',#2319,.T.);
#1548=FACE_OUTER_BOUND('',#2320,.T.);
#1549=FACE_OUTER_BOUND('',#2321,.T.);
#1550=FACE_OUTER_BOUND('',#2322,.T.);
#1551=FACE_OUTER_BOUND('',#2323,.T.);
#1552=FACE_OUTER_BOUND('',#2324,.T.);
#1553=FACE_OUTER_BOUND('',#2325,.T.);
#1554=FACE_OUTER_BOUND('',#2326,.T.);
#1555=FACE_OUTER_BOUND('',#2327,.T.);
#1556=FACE_OUTER_BOUND('',#2328,.T.);
#1557=FACE_OUTER_BOUND('',#2329,.T.);
#1558=FACE_OUTER_BOUND('',#2330,.T.);
#1559=FACE_OUTER_BOUND('',#2331,.T.);
#1560=FACE_OUTER_BOUND('',#2332,.T.);
#1561=FACE_OUTER_BOUND('',#2333,.T.);
#1562=FACE_OUTER_BOUND('',#2334,.T.);
#1563=FACE_OUTER_BOUND('',#2335,.T.);
#1564=FACE_OUTER_BOUND('',#2336,.T.);
#1565=FACE_OUTER_BOUND('',#2337,.T.);
#1566=FACE_OUTER_BOUND('',#2338,.T.);
#1567=FACE_OUTER_BOUND('',#2339,.T.);
#1568=FACE_OUTER_BOUND('',#2340,.T.);
#1569=FACE_OUTER_BOUND('',#2341,.T.);
#1570=FACE_OUTER_BOUND('',#2342,.T.);
#1571=FACE_OUTER_BOUND('',#2343,.T.);
#1572=FACE_OUTER_BOUND('',#2344,.T.);
#1573=FACE_OUTER_BOUND('',#2345,.T.);
#1574=FACE_OUTER_BOUND('',#2346,.T.);
#1575=FACE_OUTER_BOUND('',#2347,.T.);
#1576=FACE_OUTER_BOUND('',#2348,.T.);
#1577=FACE_OUTER_BOUND('',#2349,.T.);
#1578=FACE_OUTER_BOUND('',#2350,.T.);
#1579=FACE_OUTER_BOUND('',#2351,.T.);
#1580=FACE_OUTER_BOUND('',#2352,.T.);
#1581=FACE_OUTER_BOUND('',#2353,.T.);
#1582=FACE_OUTER_BOUND('',#2354,.T.);
#1583=FACE_OUTER_BOUND('',#2355,.T.);
#1584=FACE_OUTER_BOUND('',#2356,.T.);
#1585=FACE_OUTER_BOUND('',#2357,.T.);
#1586=FACE_OUTER_BOUND('',#2358,.T.);
#1587=FACE_OUTER_BOUND('',#2359,.T.);
#1588=FACE_OUTER_BOUND('',#2360,.T.);
#1589=FACE_OUTER_BOUND('',#2361,.T.);
#1590=FACE_OUTER_BOUND('',#2362,.T.);
#1591=FACE_OUTER_BOUND('',#2363,.T.);
#1592=FACE_OUTER_BOUND('',#2364,.T.);
#1593=FACE_OUTER_BOUND('',#2365,.T.);
#1594=FACE_OUTER_BOUND('',#2366,.T.);
#1595=FACE_OUTER_BOUND('',#2367,.T.);
#1596=FACE_OUTER_BOUND('',#2368,.T.);
#1597=FACE_OUTER_BOUND('',#2369,.T.);
#1598=FACE_OUTER_BOUND('',#2370,.T.);
#1599=FACE_OUTER_BOUND('',#2371,.T.);
#1600=FACE_OUTER_BOUND('',#2372,.T.);
#1601=FACE_OUTER_BOUND('',#2373,.T.);
#1602=FACE_OUTER_BOUND('',#2374,.T.);
#1603=FACE_OUTER_BOUND('',#2375,.T.);
#1604=FACE_OUTER_BOUND('',#2376,.T.);
#1605=FACE_OUTER_BOUND('',#2377,.T.);
#1606=FACE_OUTER_BOUND('',#2378,.T.);
#1607=FACE_OUTER_BOUND('',#2379,.T.);
#1608=FACE_OUTER_BOUND('',#2380,.T.);
#1609=FACE_OUTER_BOUND('',#2381,.T.);
#1610=FACE_OUTER_BOUND('',#2382,.T.);
#1611=FACE_OUTER_BOUND('',#2383,.T.);
#1612=FACE_OUTER_BOUND('',#2384,.T.);
#1613=FACE_OUTER_BOUND('',#2385,.T.);
#1614=FACE_OUTER_BOUND('',#2386,.T.);
#1615=FACE_OUTER_BOUND('',#2387,.T.);
#1616=FACE_OUTER_BOUND('',#2388,.T.);
#1617=FACE_OUTER_BOUND('',#2389,.T.);
#1618=FACE_OUTER_BOUND('',#2390,.T.);
#1619=FACE_OUTER_BOUND('',#2391,.T.);
#1620=FACE_OUTER_BOUND('',#2392,.T.);
#1621=FACE_OUTER_BOUND('',#2393,.T.);
#1622=FACE_OUTER_BOUND('',#2394,.T.);
#1623=FACE_OUTER_BOUND('',#2395,.T.);
#1624=FACE_OUTER_BOUND('',#2396,.T.);
#1625=FACE_OUTER_BOUND('',#2397,.T.);
#1626=FACE_OUTER_BOUND('',#2398,.T.);
#1627=FACE_OUTER_BOUND('',#2399,.T.);
#1628=FACE_OUTER_BOUND('',#2400,.T.);
#1629=FACE_OUTER_BOUND('',#2401,.T.);
#1630=FACE_OUTER_BOUND('',#2402,.T.);
#1631=FACE_OUTER_BOUND('',#2403,.T.);
#1632=FACE_OUTER_BOUND('',#2404,.T.);
#1633=FACE_OUTER_BOUND('',#2405,.T.);
#1634=FACE_OUTER_BOUND('',#2406,.T.);
#1635=FACE_OUTER_BOUND('',#2407,.T.);
#1636=FACE_OUTER_BOUND('',#2408,.T.);
#1637=FACE_OUTER_BOUND('',#2409,.T.);
#1638=FACE_OUTER_BOUND('',#2410,.T.);
#1639=FACE_OUTER_BOUND('',#2411,.T.);
#1640=FACE_OUTER_BOUND('',#2412,.T.);
#1641=FACE_OUTER_BOUND('',#2413,.T.);
#1642=FACE_OUTER_BOUND('',#2414,.T.);
#1643=FACE_OUTER_BOUND('',#2415,.T.);
#1644=FACE_OUTER_BOUND('',#2416,.T.);
#1645=FACE_OUTER_BOUND('',#2417,.T.);
#1646=FACE_OUTER_BOUND('',#2418,.T.);
#1647=FACE_OUTER_BOUND('',#2419,.T.);
#1648=FACE_OUTER_BOUND('',#2420,.T.);
#1649=FACE_OUTER_BOUND('',#2421,.T.);
#1650=FACE_OUTER_BOUND('',#2422,.T.);
#1651=FACE_OUTER_BOUND('',#2423,.T.);
#1652=FACE_OUTER_BOUND('',#2424,.T.);
#1653=FACE_OUTER_BOUND('',#2425,.T.);
#1654=FACE_OUTER_BOUND('',#2426,.T.);
#1655=FACE_OUTER_BOUND('',#2427,.T.);
#1656=FACE_OUTER_BOUND('',#2428,.T.);
#1657=FACE_OUTER_BOUND('',#2429,.T.);
#1658=FACE_OUTER_BOUND('',#2430,.T.);
#1659=FACE_OUTER_BOUND('',#2431,.T.);
#1660=FACE_OUTER_BOUND('',#2432,.T.);
#1661=FACE_OUTER_BOUND('',#2433,.T.);
#1662=FACE_OUTER_BOUND('',#2434,.T.);
#1663=FACE_OUTER_BOUND('',#2435,.T.);
#1664=FACE_OUTER_BOUND('',#2436,.T.);
#1665=FACE_OUTER_BOUND('',#2437,.T.);
#1666=FACE_OUTER_BOUND('',#2438,.T.);
#1667=FACE_OUTER_BOUND('',#2439,.T.);
#1668=FACE_OUTER_BOUND('',#2440,.T.);
#1669=FACE_OUTER_BOUND('',#2441,.T.);
#1670=FACE_OUTER_BOUND('',#2442,.T.);
#1671=FACE_OUTER_BOUND('',#2443,.T.);
#1672=FACE_OUTER_BOUND('',#2444,.T.);
#1673=FACE_OUTER_BOUND('',#2445,.T.);
#1674=FACE_OUTER_BOUND('',#2446,.T.);
#1675=FACE_OUTER_BOUND('',#2447,.T.);
#1676=FACE_OUTER_BOUND('',#2448,.T.);
#1677=FACE_OUTER_BOUND('',#2449,.T.);
#1678=FACE_OUTER_BOUND('',#2450,.T.);
#1679=FACE_OUTER_BOUND('',#2451,.T.);
#1680=FACE_OUTER_BOUND('',#2452,.T.);
#1681=FACE_OUTER_BOUND('',#2453,.T.);
#1682=FACE_OUTER_BOUND('',#2454,.T.);
#1683=FACE_OUTER_BOUND('',#2455,.T.);
#1684=FACE_OUTER_BOUND('',#2456,.T.);
#1685=FACE_OUTER_BOUND('',#2457,.T.);
#1686=FACE_OUTER_BOUND('',#2458,.T.);
#1687=FACE_OUTER_BOUND('',#2459,.T.);
#1688=FACE_OUTER_BOUND('',#2460,.T.);
#1689=FACE_OUTER_BOUND('',#2461,.T.);
#1690=FACE_OUTER_BOUND('',#2462,.T.);
#1691=FACE_OUTER_BOUND('',#2463,.T.);
#1692=FACE_OUTER_BOUND('',#2464,.T.);
#1693=FACE_OUTER_BOUND('',#2465,.T.);
#1694=FACE_OUTER_BOUND('',#2466,.T.);
#1695=FACE_OUTER_BOUND('',#2467,.T.);
#1696=FACE_OUTER_BOUND('',#2468,.T.);
#1697=FACE_OUTER_BOUND('',#2469,.T.);
#1698=FACE_OUTER_BOUND('',#2470,.T.);
#1699=FACE_OUTER_BOUND('',#2472,.T.);
#1700=FACE_OUTER_BOUND('',#2474,.T.);
#1701=FACE_OUTER_BOUND('',#2476,.T.);
#1702=FACE_OUTER_BOUND('',#2477,.T.);
#1703=FACE_OUTER_BOUND('',#2478,.T.);
#1704=FACE_OUTER_BOUND('',#2479,.T.);
#1705=FACE_OUTER_BOUND('',#2480,.T.);
#1706=FACE_OUTER_BOUND('',#2481,.T.);
#1707=FACE_OUTER_BOUND('',#2482,.T.);
#1708=FACE_OUTER_BOUND('',#2483,.T.);
#1709=FACE_OUTER_BOUND('',#2484,.T.);
#1710=FACE_OUTER_BOUND('',#2485,.T.);
#1711=FACE_OUTER_BOUND('',#2486,.T.);
#1712=FACE_OUTER_BOUND('',#2487,.T.);
#1713=FACE_OUTER_BOUND('',#2488,.T.);
#1714=FACE_OUTER_BOUND('',#2489,.T.);
#1715=FACE_OUTER_BOUND('',#2490,.T.);
#1716=FACE_OUTER_BOUND('',#2491,.T.);
#1717=FACE_OUTER_BOUND('',#2492,.T.);
#1718=FACE_OUTER_BOUND('',#2493,.T.);
#1719=FACE_OUTER_BOUND('',#2494,.T.);
#1720=FACE_OUTER_BOUND('',#2495,.T.);
#1721=FACE_OUTER_BOUND('',#2496,.T.);
#1722=FACE_OUTER_BOUND('',#2497,.T.);
#1723=FACE_OUTER_BOUND('',#2498,.T.);
#1724=FACE_OUTER_BOUND('',#2499,.T.);
#1725=FACE_OUTER_BOUND('',#2500,.T.);
#1726=FACE_OUTER_BOUND('',#2501,.T.);
#1727=FACE_OUTER_BOUND('',#2502,.T.);
#1728=FACE_OUTER_BOUND('',#2503,.T.);
#1729=FACE_OUTER_BOUND('',#2504,.T.);
#1730=FACE_OUTER_BOUND('',#2505,.T.);
#1731=FACE_OUTER_BOUND('',#2506,.T.);
#1732=FACE_OUTER_BOUND('',#2507,.T.);
#1733=FACE_OUTER_BOUND('',#2508,.T.);
#1734=FACE_OUTER_BOUND('',#2509,.T.);
#1735=FACE_OUTER_BOUND('',#2510,.T.);
#1736=FACE_OUTER_BOUND('',#2511,.T.);
#1737=FACE_OUTER_BOUND('',#2512,.T.);
#1738=FACE_OUTER_BOUND('',#2513,.T.);
#1739=FACE_OUTER_BOUND('',#2514,.T.);
#1740=FACE_OUTER_BOUND('',#2515,.T.);
#1741=FACE_OUTER_BOUND('',#2516,.T.);
#1742=FACE_OUTER_BOUND('',#2517,.T.);
#1743=FACE_OUTER_BOUND('',#2518,.T.);
#1744=FACE_OUTER_BOUND('',#2519,.T.);
#1745=FACE_OUTER_BOUND('',#2520,.T.);
#1746=FACE_OUTER_BOUND('',#2521,.T.);
#1747=FACE_OUTER_BOUND('',#2522,.T.);
#1748=FACE_OUTER_BOUND('',#2523,.T.);
#1749=FACE_OUTER_BOUND('',#2524,.T.);
#1750=FACE_OUTER_BOUND('',#2526,.T.);
#1751=FACE_OUTER_BOUND('',#2527,.T.);
#1752=FACE_OUTER_BOUND('',#2528,.T.);
#1753=FACE_OUTER_BOUND('',#2529,.T.);
#1754=FACE_OUTER_BOUND('',#2530,.T.);
#1755=FACE_OUTER_BOUND('',#2531,.T.);
#1756=FACE_OUTER_BOUND('',#2532,.T.);
#1757=FACE_OUTER_BOUND('',#2534,.T.);
#1758=FACE_OUTER_BOUND('',#2536,.T.);
#1759=EDGE_LOOP('',(#7051,#7052,#7053,#7054));
#1760=EDGE_LOOP('',(#7055,#7056,#7057,#7058));
#1761=EDGE_LOOP('',(#7059,#7060,#7061,#7062));
#1762=EDGE_LOOP('',(#7063,#7064,#7065,#7066));
#1763=EDGE_LOOP('',(#7067,#7068,#7069,#7070,#7071));
#1764=EDGE_LOOP('',(#7072,#7073,#7074,#7075,#7076));
#1765=EDGE_LOOP('',(#7077,#7078,#7079,#7080));
#1766=EDGE_LOOP('',(#7081,#7082,#7083,#7084,#7085));
#1767=EDGE_LOOP('',(#7086,#7087,#7088,#7089));
#1768=EDGE_LOOP('',(#7090,#7091,#7092,#7093));
#1769=EDGE_LOOP('',(#7094,#7095,#7096,#7097));
#1770=EDGE_LOOP('',(#7098,#7099,#7100,#7101));
#1771=EDGE_LOOP('',(#7102,#7103,#7104,#7105,#7106));
#1772=EDGE_LOOP('',(#7107,#7108,#7109,#7110,#7111));
#1773=EDGE_LOOP('',(#7112,#7113,#7114,#7115,#7116));
#1774=EDGE_LOOP('',(#7117,#7118,#7119,#7120,#7121));
#1775=EDGE_LOOP('',(#7122,#7123,#7124,#7125));
#1776=EDGE_LOOP('',(#7126,#7127,#7128,#7129));
#1777=EDGE_LOOP('',(#7130,#7131,#7132,#7133));
#1778=EDGE_LOOP('',(#7134,#7135,#7136,#7137));
#1779=EDGE_LOOP('',(#7138,#7139,#7140,#7141));
#1780=EDGE_LOOP('',(#7142,#7143,#7144,#7145));
#1781=EDGE_LOOP('',(#7146,#7147,#7148,#7149,#7150));
#1782=EDGE_LOOP('',(#7151,#7152,#7153,#7154));
#1783=EDGE_LOOP('',(#7155,#7156,#7157,#7158));
#1784=EDGE_LOOP('',(#7159,#7160,#7161,#7162));
#1785=EDGE_LOOP('',(#7163,#7164,#7165,#7166,#7167));
#1786=EDGE_LOOP('',(#7168,#7169,#7170,#7171,#7172));
#1787=EDGE_LOOP('',(#7173,#7174,#7175,#7176,#7177));
#1788=EDGE_LOOP('',(#7178,#7179,#7180,#7181,#7182));
#1789=EDGE_LOOP('',(#7183,#7184,#7185,#7186));
#1790=EDGE_LOOP('',(#7187,#7188,#7189,#7190));
#1791=EDGE_LOOP('',(#7191,#7192,#7193,#7194));
#1792=EDGE_LOOP('',(#7195,#7196,#7197,#7198));
#1793=EDGE_LOOP('',(#7199,#7200,#7201,#7202));
#1794=EDGE_LOOP('',(#7203,#7204,#7205,#7206));
#1795=EDGE_LOOP('',(#7207,#7208,#7209,#7210));
#1796=EDGE_LOOP('',(#7211,#7212,#7213,#7214));
#1797=EDGE_LOOP('',(#7215,#7216,#7217,#7218));
#1798=EDGE_LOOP('',(#7219,#7220,#7221,#7222));
#1799=EDGE_LOOP('',(#7223,#7224,#7225,#7226));
#1800=EDGE_LOOP('',(#7227,#7228,#7229,#7230));
#1801=EDGE_LOOP('',(#7231,#7232,#7233,#7234));
#1802=EDGE_LOOP('',(#7235,#7236,#7237,#7238));
#1803=EDGE_LOOP('',(#7239,#7240,#7241,#7242));
#1804=EDGE_LOOP('',(#7243,#7244,#7245,#7246));
#1805=EDGE_LOOP('',(#7247,#7248,#7249,#7250));
#1806=EDGE_LOOP('',(#7251,#7252,#7253,#7254));
#1807=EDGE_LOOP('',(#7255,#7256,#7257,#7258));
#1808=EDGE_LOOP('',(#7259,#7260,#7261,#7262,#7263,#7264));
#1809=EDGE_LOOP('',(#7265,#7266,#7267,#7268,#7269,#7270));
#1810=EDGE_LOOP('',(#7271,#7272,#7273,#7274));
#1811=EDGE_LOOP('',(#7275,#7276,#7277,#7278));
#1812=EDGE_LOOP('',(#7279,#7280,#7281,#7282));
#1813=EDGE_LOOP('',(#7283,#7284,#7285,#7286));
#1814=EDGE_LOOP('',(#7287,#7288,#7289,#7290,#7291));
#1815=EDGE_LOOP('',(#7292,#7293,#7294,#7295,#7296,#7297,#7298));
#1816=EDGE_LOOP('',(#7299,#7300,#7301,#7302));
#1817=EDGE_LOOP('',(#7303,#7304,#7305,#7306));
#1818=EDGE_LOOP('',(#7307,#7308,#7309,#7310));
#1819=EDGE_LOOP('',(#7311,#7312,#7313,#7314,#7315,#7316));
#1820=EDGE_LOOP('',(#7317,#7318,#7319,#7320,#7321,#7322));
#1821=EDGE_LOOP('',(#7323,#7324,#7325,#7326,#7327,#7328,#7329));
#1822=EDGE_LOOP('',(#7330,#7331,#7332,#7333));
#1823=EDGE_LOOP('',(#7334,#7335,#7336,#7337));
#1824=EDGE_LOOP('',(#7338,#7339,#7340,#7341));
#1825=EDGE_LOOP('',(#7342,#7343,#7344,#7345,#7346,#7347,#7348,#7349,#7350,
#7351,#7352,#7353,#7354,#7355,#7356,#7357,#7358,#7359,#7360,#7361,#7362,
#7363,#7364,#7365,#7366,#7367,#7368,#7369,#7370,#7371,#7372,#7373,#7374,
#7375,#7376,#7377,#7378,#7379,#7380,#7381,#7382,#7383,#7384,#7385,#7386,
#7387,#7388,#7389,#7390,#7391,#7392,#7393,#7394,#7395,#7396,#7397,#7398,
#7399,#7400,#7401,#7402,#7403,#7404,#7405,#7406,#7407,#7408,#7409,#7410,
#7411,#7412,#7413,#7414,#7415));
#1826=EDGE_LOOP('',(#7416,#7417,#7418,#7419,#7420,#7421));
#1827=EDGE_LOOP('',(#7422,#7423,#7424,#7425,#7426));
#1828=EDGE_LOOP('',(#7427,#7428,#7429,#7430,#7431,#7432,#7433));
#1829=EDGE_LOOP('',(#7434,#7435,#7436,#7437));
#1830=EDGE_LOOP('',(#7438,#7439,#7440,#7441));
#1831=EDGE_LOOP('',(#7442,#7443,#7444,#7445,#7446,#7447,#7448,#7449,#7450,
#7451,#7452,#7453,#7454,#7455,#7456,#7457,#7458,#7459,#7460,#7461,#7462,
#7463));
#1832=EDGE_LOOP('',(#7464));
#1833=EDGE_LOOP('',(#7465,#7466,#7467,#7468,#7469,#7470,#7471,#7472));
#1834=EDGE_LOOP('',(#7473));
#1835=EDGE_LOOP('',(#7474));
#1836=EDGE_LOOP('',(#7475,#7476,#7477,#7478,#7479,#7480,#7481,#7482));
#1837=EDGE_LOOP('',(#7483,#7484,#7485,#7486,#7487,#7488,#7489,#7490));
#1838=EDGE_LOOP('',(#7491));
#1839=EDGE_LOOP('',(#7492,#7493,#7494,#7495,#7496,#7497,#7498,#7499,#7500,
#7501,#7502,#7503,#7504,#7505,#7506,#7507));
#1840=EDGE_LOOP('',(#7508,#7509,#7510,#7511));
#1841=EDGE_LOOP('',(#7512,#7513,#7514,#7515));
#1842=EDGE_LOOP('',(#7516,#7517,#7518,#7519,#7520,#7521,#7522,#7523,#7524,
#7525,#7526,#7527,#7528,#7529,#7530,#7531,#7532,#7533));
#1843=EDGE_LOOP('',(#7534));
#1844=EDGE_LOOP('',(#7535,#7536,#7537,#7538,#7539,#7540,#7541,#7542,#7543,
#7544,#7545,#7546,#7547,#7548,#7549,#7550));
#1845=EDGE_LOOP('',(#7551));
#1846=EDGE_LOOP('',(#7552,#7553,#7554,#7555));
#1847=EDGE_LOOP('',(#7556,#7557,#7558,#7559));
#1848=EDGE_LOOP('',(#7560,#7561,#7562,#7563));
#1849=EDGE_LOOP('',(#7564,#7565,#7566,#7567));
#1850=EDGE_LOOP('',(#7568,#7569,#7570,#7571));
#1851=EDGE_LOOP('',(#7572,#7573,#7574,#7575));
#1852=EDGE_LOOP('',(#7576,#7577,#7578,#7579));
#1853=EDGE_LOOP('',(#7580,#7581,#7582,#7583));
#1854=EDGE_LOOP('',(#7584,#7585,#7586,#7587));
#1855=EDGE_LOOP('',(#7588,#7589,#7590,#7591));
#1856=EDGE_LOOP('',(#7592,#7593,#7594,#7595,#7596));
#1857=EDGE_LOOP('',(#7597));
#1858=EDGE_LOOP('',(#7598,#7599,#7600,#7601,#7602));
#1859=EDGE_LOOP('',(#7603,#7604,#7605,#7606,#7607));
#1860=EDGE_LOOP('',(#7608,#7609,#7610,#7611,#7612));
#1861=EDGE_LOOP('',(#7613,#7614,#7615,#7616,#7617));
#1862=EDGE_LOOP('',(#7618,#7619,#7620,#7621,#7622,#7623,#7624));
#1863=EDGE_LOOP('',(#7625,#7626,#7627,#7628,#7629,#7630,#7631,#7632,#7633,
#7634,#7635,#7636,#7637,#7638,#7639,#7640,#7641,#7642,#7643,#7644,#7645,
#7646,#7647,#7648,#7649,#7650,#7651,#7652));
#1864=EDGE_LOOP('',(#7653,#7654,#7655,#7656,#7657,#7658,#7659));
#1865=EDGE_LOOP('',(#7660,#7661,#7662,#7663,#7664,#7665,#7666));
#1866=EDGE_LOOP('',(#7667,#7668,#7669,#7670,#7671,#7672,#7673));
#1867=EDGE_LOOP('',(#7674,#7675,#7676,#7677,#7678,#7679));
#1868=EDGE_LOOP('',(#7680,#7681,#7682,#7683));
#1869=EDGE_LOOP('',(#7684,#7685,#7686,#7687));
#1870=EDGE_LOOP('',(#7688,#7689,#7690,#7691,#7692,#7693));
#1871=EDGE_LOOP('',(#7694,#7695,#7696,#7697,#7698,#7699));
#1872=EDGE_LOOP('',(#7700,#7701,#7702,#7703,#7704,#7705,#7706,#7707));
#1873=EDGE_LOOP('',(#7708));
#1874=EDGE_LOOP('',(#7709,#7710,#7711,#7712,#7713,#7714,#7715,#7716));
#1875=EDGE_LOOP('',(#7717));
#1876=EDGE_LOOP('',(#7718,#7719,#7720,#7721,#7722,#7723,#7724,#7725));
#1877=EDGE_LOOP('',(#7726,#7727,#7728,#7729,#7730,#7731,#7732,#7733));
#1878=EDGE_LOOP('',(#7734,#7735,#7736,#7737));
#1879=EDGE_LOOP('',(#7738,#7739,#7740,#7741,#7742,#7743,#7744,#7745));
#1880=EDGE_LOOP('',(#7746,#7747,#7748,#7749,#7750,#7751,#7752,#7753));
#1881=EDGE_LOOP('',(#7754,#7755,#7756,#7757,#7758,#7759,#7760,#7761,#7762,
#7763,#7764,#7765,#7766,#7767,#7768,#7769,#7770,#7771,#7772,#7773,#7774,
#7775,#7776,#7777,#7778,#7779,#7780,#7781,#7782,#7783,#7784));
#1882=EDGE_LOOP('',(#7785));
#1883=EDGE_LOOP('',(#7786));
#1884=EDGE_LOOP('',(#7787,#7788,#7789,#7790,#7791,#7792,#7793,#7794,#7795,
#7796,#7797));
#1885=EDGE_LOOP('',(#7798));
#1886=EDGE_LOOP('',(#7799));
#1887=EDGE_LOOP('',(#7800,#7801,#7802,#7803,#7804,#7805,#7806,#7807,#7808,
#7809,#7810));
#1888=EDGE_LOOP('',(#7811,#7812,#7813,#7814,#7815,#7816,#7817,#7818,#7819,
#7820,#7821));
#1889=EDGE_LOOP('',(#7822));
#1890=EDGE_LOOP('',(#7823,#7824,#7825,#7826));
#1891=EDGE_LOOP('',(#7827,#7828,#7829,#7830));
#1892=EDGE_LOOP('',(#7831,#7832,#7833,#7834,#7835));
#1893=EDGE_LOOP('',(#7836,#7837,#7838,#7839,#7840));
#1894=EDGE_LOOP('',(#7841,#7842,#7843,#7844,#7845,#7846));
#1895=EDGE_LOOP('',(#7847,#7848,#7849,#7850,#7851,#7852));
#1896=EDGE_LOOP('',(#7853,#7854,#7855,#7856));
#1897=EDGE_LOOP('',(#7857,#7858,#7859,#7860));
#1898=EDGE_LOOP('',(#7861,#7862,#7863));
#1899=EDGE_LOOP('',(#7864,#7865,#7866,#7867));
#1900=EDGE_LOOP('',(#7868,#7869,#7870));
#1901=EDGE_LOOP('',(#7871,#7872,#7873,#7874));
#1902=EDGE_LOOP('',(#7875,#7876,#7877,#7878));
#1903=EDGE_LOOP('',(#7879,#7880,#7881,#7882));
#1904=EDGE_LOOP('',(#7883,#7884,#7885,#7886,#7887,#7888,#7889,#7890));
#1905=EDGE_LOOP('',(#7891,#7892,#7893,#7894));
#1906=EDGE_LOOP('',(#7895,#7896,#7897,#7898));
#1907=EDGE_LOOP('',(#7899,#7900,#7901,#7902));
#1908=EDGE_LOOP('',(#7903,#7904,#7905,#7906,#7907,#7908,#7909));
#1909=EDGE_LOOP('',(#7910,#7911,#7912,#7913,#7914,#7915,#7916));
#1910=EDGE_LOOP('',(#7917,#7918,#7919,#7920,#7921,#7922,#7923));
#1911=EDGE_LOOP('',(#7924,#7925,#7926,#7927,#7928,#7929,#7930));
#1912=EDGE_LOOP('',(#7931,#7932,#7933,#7934));
#1913=EDGE_LOOP('',(#7935,#7936,#7937,#7938,#7939,#7940));
#1914=EDGE_LOOP('',(#7941,#7942,#7943,#7944,#7945,#7946,#7947,#7948));
#1915=EDGE_LOOP('',(#7949));
#1916=EDGE_LOOP('',(#7950,#7951,#7952,#7953,#7954,#7955,#7956,#7957));
#1917=EDGE_LOOP('',(#7958));
#1918=EDGE_LOOP('',(#7959,#7960,#7961,#7962,#7963,#7964,#7965,#7966));
#1919=EDGE_LOOP('',(#7967,#7968,#7969,#7970));
#1920=EDGE_LOOP('',(#7971,#7972,#7973,#7974,#7975,#7976,#7977,#7978));
#1921=EDGE_LOOP('',(#7979,#7980,#7981,#7982));
#1922=EDGE_LOOP('',(#7983,#7984,#7985,#7986));
#1923=EDGE_LOOP('',(#7987,#7988,#7989,#7990,#7991));
#1924=EDGE_LOOP('',(#7992,#7993,#7994,#7995,#7996,#7997));
#1925=EDGE_LOOP('',(#7998,#7999,#8000,#8001,#8002,#8003));
#1926=EDGE_LOOP('',(#8004,#8005,#8006,#8007));
#1927=EDGE_LOOP('',(#8008,#8009,#8010,#8011));
#1928=EDGE_LOOP('',(#8012,#8013,#8014));
#1929=EDGE_LOOP('',(#8015,#8016,#8017,#8018));
#1930=EDGE_LOOP('',(#8019,#8020,#8021));
#1931=EDGE_LOOP('',(#8022,#8023,#8024,#8025));
#1932=EDGE_LOOP('',(#8026,#8027,#8028,#8029));
#1933=EDGE_LOOP('',(#8030,#8031,#8032,#8033));
#1934=EDGE_LOOP('',(#8034,#8035,#8036,#8037,#8038,#8039,#8040,#8041));
#1935=EDGE_LOOP('',(#8042,#8043,#8044,#8045));
#1936=EDGE_LOOP('',(#8046,#8047,#8048,#8049));
#1937=EDGE_LOOP('',(#8050,#8051,#8052,#8053));
#1938=EDGE_LOOP('',(#8054,#8055,#8056,#8057,#8058,#8059,#8060));
#1939=EDGE_LOOP('',(#8061,#8062,#8063,#8064,#8065,#8066,#8067));
#1940=EDGE_LOOP('',(#8068,#8069,#8070,#8071,#8072,#8073,#8074));
#1941=EDGE_LOOP('',(#8075,#8076,#8077,#8078,#8079,#8080,#8081));
#1942=EDGE_LOOP('',(#8082,#8083,#8084,#8085));
#1943=EDGE_LOOP('',(#8086,#8087,#8088,#8089,#8090,#8091));
#1944=EDGE_LOOP('',(#8092,#8093,#8094,#8095,#8096,#8097,#8098,#8099));
#1945=EDGE_LOOP('',(#8100,#8101,#8102,#8103));
#1946=EDGE_LOOP('',(#8104,#8105,#8106,#8107,#8108,#8109,#8110,#8111));
#1947=EDGE_LOOP('',(#8112,#8113,#8114,#8115));
#1948=EDGE_LOOP('',(#8116,#8117,#8118,#8119));
#1949=EDGE_LOOP('',(#8120,#8121,#8122,#8123,#8124));
#1950=EDGE_LOOP('',(#8125,#8126,#8127,#8128,#8129,#8130));
#1951=EDGE_LOOP('',(#8131,#8132,#8133,#8134,#8135,#8136));
#1952=EDGE_LOOP('',(#8137,#8138,#8139,#8140));
#1953=EDGE_LOOP('',(#8141,#8142,#8143,#8144));
#1954=EDGE_LOOP('',(#8145,#8146,#8147));
#1955=EDGE_LOOP('',(#8148,#8149,#8150,#8151));
#1956=EDGE_LOOP('',(#8152,#8153,#8154));
#1957=EDGE_LOOP('',(#8155,#8156,#8157,#8158));
#1958=EDGE_LOOP('',(#8159,#8160,#8161,#8162));
#1959=EDGE_LOOP('',(#8163,#8164,#8165,#8166));
#1960=EDGE_LOOP('',(#8167,#8168,#8169,#8170,#8171,#8172,#8173,#8174,#8175,
#8176,#8177,#8178));
#1961=EDGE_LOOP('',(#8179,#8180,#8181,#8182));
#1962=EDGE_LOOP('',(#8183,#8184,#8185,#8186));
#1963=EDGE_LOOP('',(#8187,#8188,#8189,#8190));
#1964=EDGE_LOOP('',(#8191,#8192,#8193,#8194,#8195,#8196,#8197));
#1965=EDGE_LOOP('',(#8198,#8199,#8200,#8201,#8202,#8203,#8204));
#1966=EDGE_LOOP('',(#8205,#8206,#8207,#8208,#8209,#8210,#8211));
#1967=EDGE_LOOP('',(#8212,#8213,#8214,#8215,#8216,#8217,#8218));
#1968=EDGE_LOOP('',(#8219,#8220,#8221,#8222,#8223,#8224,#8225,#8226));
#1969=EDGE_LOOP('',(#8227));
#1970=EDGE_LOOP('',(#8228,#8229,#8230,#8231,#8232,#8233,#8234,#8235));
#1971=EDGE_LOOP('',(#8236));
#1972=EDGE_LOOP('',(#8237,#8238,#8239,#8240));
#1973=EDGE_LOOP('',(#8241,#8242,#8243,#8244));
#1974=EDGE_LOOP('',(#8245,#8246,#8247,#8248));
#1975=EDGE_LOOP('',(#8249,#8250,#8251,#8252,#8253,#8254));
#1976=EDGE_LOOP('',(#8255,#8256,#8257,#8258,#8259,#8260));
#1977=EDGE_LOOP('',(#8261,#8262,#8263,#8264));
#1978=EDGE_LOOP('',(#8265,#8266,#8267,#8268));
#1979=EDGE_LOOP('',(#8269,#8270,#8271));
#1980=EDGE_LOOP('',(#8272,#8273,#8274,#8275));
#1981=EDGE_LOOP('',(#8276,#8277,#8278));
#1982=EDGE_LOOP('',(#8279,#8280,#8281,#8282));
#1983=EDGE_LOOP('',(#8283,#8284,#8285,#8286));
#1984=EDGE_LOOP('',(#8287,#8288,#8289,#8290));
#1985=EDGE_LOOP('',(#8291,#8292,#8293,#8294,#8295,#8296,#8297,#8298));
#1986=EDGE_LOOP('',(#8299,#8300,#8301,#8302));
#1987=EDGE_LOOP('',(#8303,#8304,#8305,#8306));
#1988=EDGE_LOOP('',(#8307,#8308,#8309,#8310));
#1989=EDGE_LOOP('',(#8311,#8312,#8313,#8314));
#1990=EDGE_LOOP('',(#8315,#8316,#8317,#8318));
#1991=EDGE_LOOP('',(#8319,#8320,#8321,#8322));
#1992=EDGE_LOOP('',(#8323,#8324,#8325,#8326));
#1993=EDGE_LOOP('',(#8327,#8328,#8329,#8330));
#1994=EDGE_LOOP('',(#8331,#8332,#8333,#8334));
#1995=EDGE_LOOP('',(#8335,#8336,#8337,#8338));
#1996=EDGE_LOOP('',(#8339,#8340,#8341,#8342));
#1997=EDGE_LOOP('',(#8343,#8344,#8345,#8346));
#1998=EDGE_LOOP('',(#8347,#8348,#8349,#8350));
#1999=EDGE_LOOP('',(#8351,#8352,#8353,#8354));
#2000=EDGE_LOOP('',(#8355,#8356,#8357,#8358));
#2001=EDGE_LOOP('',(#8359,#8360,#8361,#8362));
#2002=EDGE_LOOP('',(#8363,#8364,#8365,#8366));
#2003=EDGE_LOOP('',(#8367,#8368,#8369,#8370));
#2004=EDGE_LOOP('',(#8371,#8372,#8373,#8374));
#2005=EDGE_LOOP('',(#8375,#8376,#8377,#8378));
#2006=EDGE_LOOP('',(#8379,#8380,#8381,#8382));
#2007=EDGE_LOOP('',(#8383,#8384,#8385,#8386));
#2008=EDGE_LOOP('',(#8387,#8388,#8389,#8390));
#2009=EDGE_LOOP('',(#8391,#8392,#8393,#8394));
#2010=EDGE_LOOP('',(#8395,#8396,#8397,#8398));
#2011=EDGE_LOOP('',(#8399,#8400,#8401,#8402));
#2012=EDGE_LOOP('',(#8403,#8404,#8405,#8406));
#2013=EDGE_LOOP('',(#8407,#8408,#8409,#8410));
#2014=EDGE_LOOP('',(#8411,#8412,#8413,#8414));
#2015=EDGE_LOOP('',(#8415,#8416,#8417,#8418));
#2016=EDGE_LOOP('',(#8419,#8420,#8421,#8422));
#2017=EDGE_LOOP('',(#8423,#8424,#8425,#8426));
#2018=EDGE_LOOP('',(#8427,#8428,#8429,#8430));
#2019=EDGE_LOOP('',(#8431,#8432,#8433,#8434));
#2020=EDGE_LOOP('',(#8435,#8436,#8437,#8438));
#2021=EDGE_LOOP('',(#8439,#8440,#8441,#8442));
#2022=EDGE_LOOP('',(#8443,#8444,#8445,#8446));
#2023=EDGE_LOOP('',(#8447,#8448,#8449,#8450));
#2024=EDGE_LOOP('',(#8451,#8452,#8453,#8454));
#2025=EDGE_LOOP('',(#8455,#8456,#8457,#8458));
#2026=EDGE_LOOP('',(#8459,#8460,#8461,#8462));
#2027=EDGE_LOOP('',(#8463,#8464,#8465,#8466));
#2028=EDGE_LOOP('',(#8467,#8468,#8469,#8470));
#2029=EDGE_LOOP('',(#8471,#8472,#8473,#8474,#8475));
#2030=EDGE_LOOP('',(#8476,#8477,#8478,#8479,#8480));
#2031=EDGE_LOOP('',(#8481,#8482,#8483,#8484,#8485));
#2032=EDGE_LOOP('',(#8486,#8487,#8488,#8489));
#2033=EDGE_LOOP('',(#8490,#8491,#8492,#8493));
#2034=EDGE_LOOP('',(#8494,#8495,#8496));
#2035=EDGE_LOOP('',(#8497,#8498,#8499,#8500));
#2036=EDGE_LOOP('',(#8501,#8502,#8503));
#2037=EDGE_LOOP('',(#8504,#8505,#8506,#8507));
#2038=EDGE_LOOP('',(#8508,#8509,#8510,#8511));
#2039=EDGE_LOOP('',(#8512,#8513,#8514,#8515));
#2040=EDGE_LOOP('',(#8516,#8517,#8518,#8519));
#2041=EDGE_LOOP('',(#8520,#8521,#8522,#8523));
#2042=EDGE_LOOP('',(#8524,#8525,#8526,#8527));
#2043=EDGE_LOOP('',(#8528,#8529,#8530,#8531));
#2044=EDGE_LOOP('',(#8532,#8533,#8534,#8535));
#2045=EDGE_LOOP('',(#8536,#8537,#8538,#8539));
#2046=EDGE_LOOP('',(#8540,#8541,#8542,#8543));
#2047=EDGE_LOOP('',(#8544,#8545,#8546,#8547));
#2048=EDGE_LOOP('',(#8548,#8549,#8550,#8551,#8552));
#2049=EDGE_LOOP('',(#8553,#8554,#8555,#8556));
#2050=EDGE_LOOP('',(#8557,#8558,#8559,#8560));
#2051=EDGE_LOOP('',(#8561,#8562,#8563,#8564));
#2052=EDGE_LOOP('',(#8565,#8566,#8567,#8568));
#2053=EDGE_LOOP('',(#8569,#8570,#8571,#8572));
#2054=EDGE_LOOP('',(#8573,#8574,#8575));
#2055=EDGE_LOOP('',(#8576,#8577,#8578));
#2056=EDGE_LOOP('',(#8579,#8580,#8581,#8582));
#2057=EDGE_LOOP('',(#8583,#8584,#8585,#8586));
#2058=EDGE_LOOP('',(#8587,#8588,#8589,#8590,#8591));
#2059=EDGE_LOOP('',(#8592,#8593,#8594,#8595,#8596));
#2060=EDGE_LOOP('',(#8597,#8598,#8599,#8600,#8601));
#2061=EDGE_LOOP('',(#8602,#8603,#8604,#8605));
#2062=EDGE_LOOP('',(#8606,#8607,#8608,#8609));
#2063=EDGE_LOOP('',(#8610,#8611,#8612,#8613));
#2064=EDGE_LOOP('',(#8614,#8615,#8616,#8617));
#2065=EDGE_LOOP('',(#8618,#8619,#8620,#8621));
#2066=EDGE_LOOP('',(#8622,#8623,#8624,#8625));
#2067=EDGE_LOOP('',(#8626,#8627,#8628,#8629));
#2068=EDGE_LOOP('',(#8630,#8631,#8632,#8633));
#2069=EDGE_LOOP('',(#8634,#8635,#8636,#8637));
#2070=EDGE_LOOP('',(#8638,#8639,#8640,#8641));
#2071=EDGE_LOOP('',(#8642,#8643,#8644,#8645));
#2072=EDGE_LOOP('',(#8646,#8647,#8648,#8649));
#2073=EDGE_LOOP('',(#8650,#8651,#8652,#8653));
#2074=EDGE_LOOP('',(#8654,#8655,#8656,#8657));
#2075=EDGE_LOOP('',(#8658,#8659,#8660,#8661));
#2076=EDGE_LOOP('',(#8662,#8663,#8664,#8665));
#2077=EDGE_LOOP('',(#8666,#8667,#8668,#8669));
#2078=EDGE_LOOP('',(#8670,#8671,#8672,#8673));
#2079=EDGE_LOOP('',(#8674,#8675,#8676,#8677));
#2080=EDGE_LOOP('',(#8678,#8679,#8680,#8681));
#2081=EDGE_LOOP('',(#8682,#8683,#8684,#8685));
#2082=EDGE_LOOP('',(#8686,#8687,#8688,#8689));
#2083=EDGE_LOOP('',(#8690,#8691,#8692,#8693,#8694));
#2084=EDGE_LOOP('',(#8695,#8696,#8697));
#2085=EDGE_LOOP('',(#8698,#8699,#8700));
#2086=EDGE_LOOP('',(#8701,#8702,#8703,#8704));
#2087=EDGE_LOOP('',(#8705,#8706,#8707,#8708));
#2088=EDGE_LOOP('',(#8709,#8710,#8711,#8712));
#2089=EDGE_LOOP('',(#8713,#8714,#8715,#8716));
#2090=EDGE_LOOP('',(#8717,#8718,#8719,#8720));
#2091=EDGE_LOOP('',(#8721,#8722,#8723,#8724));
#2092=EDGE_LOOP('',(#8725,#8726,#8727,#8728));
#2093=EDGE_LOOP('',(#8729,#8730,#8731,#8732));
#2094=EDGE_LOOP('',(#8733,#8734,#8735,#8736));
#2095=EDGE_LOOP('',(#8737,#8738,#8739,#8740));
#2096=EDGE_LOOP('',(#8741,#8742,#8743,#8744));
#2097=EDGE_LOOP('',(#8745,#8746,#8747,#8748));
#2098=EDGE_LOOP('',(#8749,#8750,#8751,#8752));
#2099=EDGE_LOOP('',(#8753,#8754,#8755,#8756));
#2100=EDGE_LOOP('',(#8757,#8758,#8759,#8760));
#2101=EDGE_LOOP('',(#8761,#8762,#8763,#8764));
#2102=EDGE_LOOP('',(#8765,#8766,#8767,#8768));
#2103=EDGE_LOOP('',(#8769,#8770,#8771,#8772));
#2104=EDGE_LOOP('',(#8773,#8774,#8775,#8776));
#2105=EDGE_LOOP('',(#8777,#8778,#8779,#8780));
#2106=EDGE_LOOP('',(#8781,#8782,#8783,#8784));
#2107=EDGE_LOOP('',(#8785,#8786,#8787,#8788,#8789));
#2108=EDGE_LOOP('',(#8790,#8791,#8792,#8793,#8794));
#2109=EDGE_LOOP('',(#8795,#8796,#8797,#8798,#8799));
#2110=EDGE_LOOP('',(#8800,#8801,#8802,#8803));
#2111=EDGE_LOOP('',(#8804,#8805,#8806,#8807));
#2112=EDGE_LOOP('',(#8808,#8809,#8810));
#2113=EDGE_LOOP('',(#8811,#8812,#8813));
#2114=EDGE_LOOP('',(#8814,#8815,#8816,#8817));
#2115=EDGE_LOOP('',(#8818,#8819,#8820,#8821));
#2116=EDGE_LOOP('',(#8822,#8823,#8824,#8825));
#2117=EDGE_LOOP('',(#8826,#8827,#8828,#8829));
#2118=EDGE_LOOP('',(#8830,#8831,#8832));
#2119=EDGE_LOOP('',(#8833,#8834,#8835));
#2120=EDGE_LOOP('',(#8836,#8837,#8838,#8839));
#2121=EDGE_LOOP('',(#8840,#8841,#8842,#8843));
#2122=EDGE_LOOP('',(#8844,#8845,#8846,#8847));
#2123=EDGE_LOOP('',(#8848,#8849,#8850,#8851));
#2124=EDGE_LOOP('',(#8852,#8853,#8854,#8855));
#2125=EDGE_LOOP('',(#8856,#8857,#8858,#8859));
#2126=EDGE_LOOP('',(#8860,#8861,#8862,#8863));
#2127=EDGE_LOOP('',(#8864,#8865,#8866,#8867));
#2128=EDGE_LOOP('',(#8868,#8869,#8870,#8871));
#2129=EDGE_LOOP('',(#8872,#8873,#8874,#8875));
#2130=EDGE_LOOP('',(#8876,#8877,#8878,#8879));
#2131=EDGE_LOOP('',(#8880,#8881,#8882,#8883));
#2132=EDGE_LOOP('',(#8884,#8885,#8886,#8887,#8888));
#2133=EDGE_LOOP('',(#8889,#8890,#8891,#8892));
#2134=EDGE_LOOP('',(#8893,#8894,#8895,#8896));
#2135=EDGE_LOOP('',(#8897,#8898,#8899,#8900));
#2136=EDGE_LOOP('',(#8901,#8902,#8903,#8904));
#2137=EDGE_LOOP('',(#8905,#8906,#8907,#8908));
#2138=EDGE_LOOP('',(#8909,#8910,#8911,#8912));
#2139=EDGE_LOOP('',(#8913,#8914,#8915,#8916));
#2140=EDGE_LOOP('',(#8917,#8918,#8919,#8920));
#2141=EDGE_LOOP('',(#8921,#8922,#8923,#8924));
#2142=EDGE_LOOP('',(#8925,#8926,#8927,#8928));
#2143=EDGE_LOOP('',(#8929,#8930,#8931,#8932));
#2144=EDGE_LOOP('',(#8933,#8934,#8935,#8936));
#2145=EDGE_LOOP('',(#8937,#8938,#8939,#8940));
#2146=EDGE_LOOP('',(#8941,#8942,#8943,#8944));
#2147=EDGE_LOOP('',(#8945,#8946,#8947,#8948));
#2148=EDGE_LOOP('',(#8949,#8950,#8951,#8952));
#2149=EDGE_LOOP('',(#8953,#8954,#8955,#8956));
#2150=EDGE_LOOP('',(#8957,#8958,#8959,#8960));
#2151=EDGE_LOOP('',(#8961,#8962,#8963,#8964));
#2152=EDGE_LOOP('',(#8965,#8966,#8967,#8968));
#2153=EDGE_LOOP('',(#8969,#8970,#8971,#8972));
#2154=EDGE_LOOP('',(#8973,#8974,#8975,#8976));
#2155=EDGE_LOOP('',(#8977,#8978,#8979));
#2156=EDGE_LOOP('',(#8980,#8981,#8982));
#2157=EDGE_LOOP('',(#8983,#8984,#8985,#8986));
#2158=EDGE_LOOP('',(#8987,#8988,#8989,#8990));
#2159=EDGE_LOOP('',(#8991,#8992,#8993,#8994));
#2160=EDGE_LOOP('',(#8995,#8996,#8997,#8998));
#2161=EDGE_LOOP('',(#8999,#9000,#9001,#9002));
#2162=EDGE_LOOP('',(#9003,#9004,#9005,#9006));
#2163=EDGE_LOOP('',(#9007,#9008,#9009,#9010));
#2164=EDGE_LOOP('',(#9011,#9012,#9013,#9014));
#2165=EDGE_LOOP('',(#9015,#9016,#9017,#9018));
#2166=EDGE_LOOP('',(#9019,#9020,#9021,#9022));
#2167=EDGE_LOOP('',(#9023,#9024,#9025));
#2168=EDGE_LOOP('',(#9026,#9027,#9028,#9029));
#2169=EDGE_LOOP('',(#9030,#9031,#9032,#9033));
#2170=EDGE_LOOP('',(#9034,#9035,#9036,#9037));
#2171=EDGE_LOOP('',(#9038,#9039,#9040,#9041));
#2172=EDGE_LOOP('',(#9042,#9043,#9044,#9045));
#2173=EDGE_LOOP('',(#9046,#9047,#9048,#9049));
#2174=EDGE_LOOP('',(#9050,#9051,#9052,#9053));
#2175=EDGE_LOOP('',(#9054,#9055,#9056,#9057));
#2176=EDGE_LOOP('',(#9058,#9059,#9060));
#2177=EDGE_LOOP('',(#9061,#9062,#9063,#9064));
#2178=EDGE_LOOP('',(#9065,#9066,#9067,#9068));
#2179=EDGE_LOOP('',(#9069,#9070,#9071,#9072));
#2180=EDGE_LOOP('',(#9073,#9074,#9075,#9076));
#2181=EDGE_LOOP('',(#9077,#9078,#9079,#9080));
#2182=EDGE_LOOP('',(#9081,#9082,#9083,#9084));
#2183=EDGE_LOOP('',(#9085,#9086,#9087,#9088));
#2184=EDGE_LOOP('',(#9089,#9090,#9091,#9092));
#2185=EDGE_LOOP('',(#9093,#9094,#9095,#9096));
#2186=EDGE_LOOP('',(#9097,#9098,#9099,#9100));
#2187=EDGE_LOOP('',(#9101,#9102,#9103,#9104));
#2188=EDGE_LOOP('',(#9105,#9106,#9107,#9108));
#2189=EDGE_LOOP('',(#9109,#9110,#9111,#9112));
#2190=EDGE_LOOP('',(#9113,#9114,#9115,#9116));
#2191=EDGE_LOOP('',(#9117,#9118,#9119,#9120));
#2192=EDGE_LOOP('',(#9121,#9122,#9123,#9124,#9125));
#2193=EDGE_LOOP('',(#9126,#9127,#9128,#9129,#9130));
#2194=EDGE_LOOP('',(#9131,#9132,#9133,#9134,#9135));
#2195=EDGE_LOOP('',(#9136,#9137,#9138,#9139));
#2196=EDGE_LOOP('',(#9140,#9141,#9142,#9143));
#2197=EDGE_LOOP('',(#9144,#9145,#9146,#9147));
#2198=EDGE_LOOP('',(#9148,#9149,#9150,#9151));
#2199=EDGE_LOOP('',(#9152,#9153,#9154,#9155));
#2200=EDGE_LOOP('',(#9156,#9157,#9158,#9159));
#2201=EDGE_LOOP('',(#9160,#9161,#9162,#9163));
#2202=EDGE_LOOP('',(#9164,#9165,#9166,#9167,#9168));
#2203=EDGE_LOOP('',(#9169,#9170,#9171,#9172));
#2204=EDGE_LOOP('',(#9173,#9174,#9175,#9176));
#2205=EDGE_LOOP('',(#9177,#9178,#9179,#9180));
#2206=EDGE_LOOP('',(#9181,#9182,#9183,#9184));
#2207=EDGE_LOOP('',(#9185,#9186,#9187,#9188));
#2208=EDGE_LOOP('',(#9189,#9190,#9191));
#2209=EDGE_LOOP('',(#9192,#9193,#9194,#9195));
#2210=EDGE_LOOP('',(#9196,#9197,#9198,#9199));
#2211=EDGE_LOOP('',(#9200,#9201,#9202,#9203));
#2212=EDGE_LOOP('',(#9204,#9205,#9206,#9207));
#2213=EDGE_LOOP('',(#9208,#9209,#9210));
#2214=EDGE_LOOP('',(#9211,#9212,#9213,#9214));
#2215=EDGE_LOOP('',(#9215,#9216,#9217,#9218));
#2216=EDGE_LOOP('',(#9219,#9220,#9221,#9222));
#2217=EDGE_LOOP('',(#9223,#9224,#9225));
#2218=EDGE_LOOP('',(#9226,#9227,#9228));
#2219=EDGE_LOOP('',(#9229,#9230,#9231,#9232));
#2220=EDGE_LOOP('',(#9233,#9234,#9235,#9236));
#2221=EDGE_LOOP('',(#9237,#9238,#9239,#9240));
#2222=EDGE_LOOP('',(#9241,#9242,#9243));
#2223=EDGE_LOOP('',(#9244,#9245,#9246));
#2224=EDGE_LOOP('',(#9247,#9248,#9249,#9250));
#2225=EDGE_LOOP('',(#9251,#9252,#9253,#9254));
#2226=EDGE_LOOP('',(#9255,#9256,#9257,#9258));
#2227=EDGE_LOOP('',(#9259,#9260,#9261,#9262));
#2228=EDGE_LOOP('',(#9263,#9264,#9265,#9266));
#2229=EDGE_LOOP('',(#9267,#9268,#9269,#9270));
#2230=EDGE_LOOP('',(#9271,#9272,#9273,#9274));
#2231=EDGE_LOOP('',(#9275,#9276,#9277,#9278));
#2232=EDGE_LOOP('',(#9279,#9280,#9281,#9282));
#2233=EDGE_LOOP('',(#9283,#9284,#9285));
#2234=EDGE_LOOP('',(#9286,#9287,#9288));
#2235=EDGE_LOOP('',(#9289,#9290,#9291));
#2236=EDGE_LOOP('',(#9292,#9293,#9294,#9295));
#2237=EDGE_LOOP('',(#9296,#9297,#9298,#9299));
#2238=EDGE_LOOP('',(#9300,#9301,#9302));
#2239=EDGE_LOOP('',(#9303,#9304,#9305,#9306));
#2240=EDGE_LOOP('',(#9307,#9308,#9309,#9310));
#2241=EDGE_LOOP('',(#9311,#9312,#9313,#9314));
#2242=EDGE_LOOP('',(#9315,#9316,#9317,#9318));
#2243=EDGE_LOOP('',(#9319,#9320,#9321,#9322));
#2244=EDGE_LOOP('',(#9323,#9324,#9325,#9326));
#2245=EDGE_LOOP('',(#9327,#9328,#9329,#9330));
#2246=EDGE_LOOP('',(#9331,#9332,#9333,#9334));
#2247=EDGE_LOOP('',(#9335,#9336,#9337,#9338));
#2248=EDGE_LOOP('',(#9339,#9340,#9341));
#2249=EDGE_LOOP('',(#9342,#9343,#9344,#9345));
#2250=EDGE_LOOP('',(#9346,#9347,#9348,#9349));
#2251=EDGE_LOOP('',(#9350,#9351,#9352,#9353));
#2252=EDGE_LOOP('',(#9354,#9355,#9356));
#2253=EDGE_LOOP('',(#9357,#9358,#9359,#9360));
#2254=EDGE_LOOP('',(#9361,#9362,#9363,#9364));
#2255=EDGE_LOOP('',(#9365,#9366,#9367,#9368,#9369));
#2256=EDGE_LOOP('',(#9370,#9371,#9372,#9373));
#2257=EDGE_LOOP('',(#9374,#9375,#9376,#9377));
#2258=EDGE_LOOP('',(#9378,#9379,#9380,#9381));
#2259=EDGE_LOOP('',(#9382,#9383,#9384,#9385));
#2260=EDGE_LOOP('',(#9386,#9387,#9388,#9389));
#2261=EDGE_LOOP('',(#9390,#9391,#9392,#9393));
#2262=EDGE_LOOP('',(#9394,#9395,#9396,#9397));
#2263=EDGE_LOOP('',(#9398,#9399,#9400,#9401));
#2264=EDGE_LOOP('',(#9402,#9403,#9404,#9405));
#2265=EDGE_LOOP('',(#9406,#9407,#9408));
#2266=EDGE_LOOP('',(#9409,#9410,#9411,#9412));
#2267=EDGE_LOOP('',(#9413,#9414,#9415,#9416));
#2268=EDGE_LOOP('',(#9417,#9418,#9419));
#2269=EDGE_LOOP('',(#9420,#9421,#9422,#9423));
#2270=EDGE_LOOP('',(#9424,#9425,#9426,#9427));
#2271=EDGE_LOOP('',(#9428,#9429,#9430));
#2272=EDGE_LOOP('',(#9431,#9432,#9433));
#2273=EDGE_LOOP('',(#9434,#9435,#9436,#9437));
#2274=EDGE_LOOP('',(#9438,#9439,#9440,#9441));
#2275=EDGE_LOOP('',(#9442,#9443,#9444,#9445));
#2276=EDGE_LOOP('',(#9446,#9447,#9448,#9449));
#2277=EDGE_LOOP('',(#9450,#9451,#9452,#9453));
#2278=EDGE_LOOP('',(#9454,#9455,#9456,#9457));
#2279=EDGE_LOOP('',(#9458,#9459,#9460,#9461));
#2280=EDGE_LOOP('',(#9462,#9463,#9464,#9465));
#2281=EDGE_LOOP('',(#9466,#9467,#9468,#9469));
#2282=EDGE_LOOP('',(#9470,#9471,#9472,#9473));
#2283=EDGE_LOOP('',(#9474,#9475,#9476,#9477));
#2284=EDGE_LOOP('',(#9478,#9479,#9480,#9481));
#2285=EDGE_LOOP('',(#9482,#9483,#9484,#9485));
#2286=EDGE_LOOP('',(#9486,#9487,#9488));
#2287=EDGE_LOOP('',(#9489,#9490,#9491));
#2288=EDGE_LOOP('',(#9492,#9493,#9494,#9495));
#2289=EDGE_LOOP('',(#9496,#9497,#9498,#9499));
#2290=EDGE_LOOP('',(#9500,#9501,#9502));
#2291=EDGE_LOOP('',(#9503,#9504,#9505));
#2292=EDGE_LOOP('',(#9506,#9507,#9508,#9509,#9510));
#2293=EDGE_LOOP('',(#9511,#9512,#9513,#9514));
#2294=EDGE_LOOP('',(#9515,#9516,#9517,#9518));
#2295=EDGE_LOOP('',(#9519,#9520,#9521,#9522));
#2296=EDGE_LOOP('',(#9523,#9524,#9525,#9526));
#2297=EDGE_LOOP('',(#9527,#9528,#9529,#9530));
#2298=EDGE_LOOP('',(#9531,#9532,#9533,#9534));
#2299=EDGE_LOOP('',(#9535,#9536,#9537,#9538));
#2300=EDGE_LOOP('',(#9539,#9540,#9541,#9542));
#2301=EDGE_LOOP('',(#9543,#9544,#9545,#9546));
#2302=EDGE_LOOP('',(#9547,#9548,#9549,#9550));
#2303=EDGE_LOOP('',(#9551,#9552,#9553,#9554));
#2304=EDGE_LOOP('',(#9555,#9556,#9557,#9558));
#2305=EDGE_LOOP('',(#9559,#9560,#9561,#9562));
#2306=EDGE_LOOP('',(#9563,#9564,#9565,#9566));
#2307=EDGE_LOOP('',(#9567,#9568,#9569));
#2308=EDGE_LOOP('',(#9570,#9571,#9572));
#2309=EDGE_LOOP('',(#9573,#9574,#9575));
#2310=EDGE_LOOP('',(#9576,#9577,#9578,#9579));
#2311=EDGE_LOOP('',(#9580,#9581,#9582,#9583));
#2312=EDGE_LOOP('',(#9584,#9585,#9586));
#2313=EDGE_LOOP('',(#9587,#9588,#9589,#9590));
#2314=EDGE_LOOP('',(#9591,#9592,#9593,#9594));
#2315=EDGE_LOOP('',(#9595,#9596,#9597,#9598));
#2316=EDGE_LOOP('',(#9599,#9600,#9601,#9602));
#2317=EDGE_LOOP('',(#9603,#9604,#9605,#9606));
#2318=EDGE_LOOP('',(#9607,#9608,#9609,#9610));
#2319=EDGE_LOOP('',(#9611,#9612,#9613,#9614));
#2320=EDGE_LOOP('',(#9615,#9616,#9617,#9618));
#2321=EDGE_LOOP('',(#9619,#9620,#9621,#9622));
#2322=EDGE_LOOP('',(#9623,#9624,#9625,#9626));
#2323=EDGE_LOOP('',(#9627,#9628,#9629,#9630));
#2324=EDGE_LOOP('',(#9631,#9632,#9633,#9634));
#2325=EDGE_LOOP('',(#9635,#9636,#9637));
#2326=EDGE_LOOP('',(#9638,#9639,#9640,#9641));
#2327=EDGE_LOOP('',(#9642,#9643,#9644));
#2328=EDGE_LOOP('',(#9645,#9646,#9647,#9648));
#2329=EDGE_LOOP('',(#9649,#9650,#9651,#9652));
#2330=EDGE_LOOP('',(#9653,#9654,#9655,#9656));
#2331=EDGE_LOOP('',(#9657,#9658,#9659,#9660));
#2332=EDGE_LOOP('',(#9661,#9662,#9663,#9664));
#2333=EDGE_LOOP('',(#9665,#9666,#9667,#9668));
#2334=EDGE_LOOP('',(#9669,#9670,#9671,#9672));
#2335=EDGE_LOOP('',(#9673,#9674,#9675,#9676));
#2336=EDGE_LOOP('',(#9677,#9678,#9679,#9680));
#2337=EDGE_LOOP('',(#9681,#9682,#9683,#9684));
#2338=EDGE_LOOP('',(#9685,#9686,#9687,#9688));
#2339=EDGE_LOOP('',(#9689,#9690,#9691,#9692));
#2340=EDGE_LOOP('',(#9693,#9694,#9695));
#2341=EDGE_LOOP('',(#9696,#9697,#9698));
#2342=EDGE_LOOP('',(#9699,#9700,#9701));
#2343=EDGE_LOOP('',(#9702,#9703,#9704));
#2344=EDGE_LOOP('',(#9705,#9706,#9707,#9708,#9709));
#2345=EDGE_LOOP('',(#9710,#9711,#9712,#9713));
#2346=EDGE_LOOP('',(#9714,#9715,#9716,#9717));
#2347=EDGE_LOOP('',(#9718,#9719,#9720,#9721));
#2348=EDGE_LOOP('',(#9722,#9723,#9724,#9725));
#2349=EDGE_LOOP('',(#9726,#9727,#9728,#9729));
#2350=EDGE_LOOP('',(#9730,#9731,#9732,#9733));
#2351=EDGE_LOOP('',(#9734,#9735,#9736,#9737));
#2352=EDGE_LOOP('',(#9738,#9739,#9740));
#2353=EDGE_LOOP('',(#9741,#9742,#9743));
#2354=EDGE_LOOP('',(#9744,#9745,#9746,#9747));
#2355=EDGE_LOOP('',(#9748,#9749,#9750,#9751));
#2356=EDGE_LOOP('',(#9752,#9753,#9754,#9755));
#2357=EDGE_LOOP('',(#9756,#9757,#9758));
#2358=EDGE_LOOP('',(#9759,#9760,#9761));
#2359=EDGE_LOOP('',(#9762,#9763,#9764,#9765));
#2360=EDGE_LOOP('',(#9766,#9767,#9768,#9769));
#2361=EDGE_LOOP('',(#9770,#9771,#9772,#9773));
#2362=EDGE_LOOP('',(#9774,#9775,#9776,#9777));
#2363=EDGE_LOOP('',(#9778,#9779,#9780,#9781));
#2364=EDGE_LOOP('',(#9782,#9783,#9784,#9785));
#2365=EDGE_LOOP('',(#9786,#9787,#9788,#9789));
#2366=EDGE_LOOP('',(#9790,#9791,#9792,#9793));
#2367=EDGE_LOOP('',(#9794,#9795,#9796,#9797));
#2368=EDGE_LOOP('',(#9798,#9799,#9800,#9801));
#2369=EDGE_LOOP('',(#9802,#9803,#9804,#9805));
#2370=EDGE_LOOP('',(#9806,#9807,#9808,#9809));
#2371=EDGE_LOOP('',(#9810,#9811,#9812,#9813));
#2372=EDGE_LOOP('',(#9814,#9815,#9816,#9817));
#2373=EDGE_LOOP('',(#9818,#9819,#9820,#9821));
#2374=EDGE_LOOP('',(#9822,#9823,#9824,#9825));
#2375=EDGE_LOOP('',(#9826,#9827,#9828,#9829));
#2376=EDGE_LOOP('',(#9830,#9831,#9832,#9833));
#2377=EDGE_LOOP('',(#9834,#9835,#9836,#9837));
#2378=EDGE_LOOP('',(#9838,#9839,#9840,#9841));
#2379=EDGE_LOOP('',(#9842,#9843,#9844,#9845));
#2380=EDGE_LOOP('',(#9846,#9847,#9848,#9849));
#2381=EDGE_LOOP('',(#9850,#9851,#9852,#9853));
#2382=EDGE_LOOP('',(#9854,#9855,#9856,#9857));
#2383=EDGE_LOOP('',(#9858,#9859,#9860,#9861,#9862));
#2384=EDGE_LOOP('',(#9863,#9864,#9865,#9866,#9867));
#2385=EDGE_LOOP('',(#9868,#9869,#9870,#9871));
#2386=EDGE_LOOP('',(#9872,#9873,#9874,#9875));
#2387=EDGE_LOOP('',(#9876,#9877,#9878,#9879));
#2388=EDGE_LOOP('',(#9880,#9881,#9882,#9883));
#2389=EDGE_LOOP('',(#9884,#9885,#9886,#9887));
#2390=EDGE_LOOP('',(#9888,#9889,#9890,#9891));
#2391=EDGE_LOOP('',(#9892,#9893,#9894,#9895));
#2392=EDGE_LOOP('',(#9896,#9897,#9898,#9899,#9900));
#2393=EDGE_LOOP('',(#9901,#9902,#9903,#9904,#9905,#9906));
#2394=EDGE_LOOP('',(#9907,#9908,#9909,#9910,#9911,#9912));
#2395=EDGE_LOOP('',(#9913,#9914,#9915,#9916,#9917));
#2396=EDGE_LOOP('',(#9918,#9919,#9920,#9921,#9922));
#2397=EDGE_LOOP('',(#9923,#9924,#9925,#9926));
#2398=EDGE_LOOP('',(#9927,#9928,#9929,#9930));
#2399=EDGE_LOOP('',(#9931,#9932,#9933,#9934,#9935));
#2400=EDGE_LOOP('',(#9936,#9937,#9938,#9939));
#2401=EDGE_LOOP('',(#9940,#9941,#9942,#9943));
#2402=EDGE_LOOP('',(#9944,#9945,#9946,#9947));
#2403=EDGE_LOOP('',(#9948,#9949,#9950,#9951));
#2404=EDGE_LOOP('',(#9952,#9953,#9954,#9955,#9956,#9957));
#2405=EDGE_LOOP('',(#9958,#9959,#9960,#9961,#9962,#9963));
#2406=EDGE_LOOP('',(#9964,#9965,#9966,#9967,#9968));
#2407=EDGE_LOOP('',(#9969,#9970,#9971,#9972));
#2408=EDGE_LOOP('',(#9973,#9974,#9975,#9976));
#2409=EDGE_LOOP('',(#9977,#9978,#9979,#9980));
#2410=EDGE_LOOP('',(#9981,#9982,#9983,#9984));
#2411=EDGE_LOOP('',(#9985,#9986,#9987,#9988,#9989));
#2412=EDGE_LOOP('',(#9990,#9991,#9992,#9993));
#2413=EDGE_LOOP('',(#9994,#9995,#9996,#9997));
#2414=EDGE_LOOP('',(#9998,#9999,#10000,#10001));
#2415=EDGE_LOOP('',(#10002,#10003,#10004,#10005));
#2416=EDGE_LOOP('',(#10006,#10007,#10008,#10009));
#2417=EDGE_LOOP('',(#10010,#10011,#10012,#10013));
#2418=EDGE_LOOP('',(#10014,#10015,#10016,#10017));
#2419=EDGE_LOOP('',(#10018,#10019,#10020,#10021));
#2420=EDGE_LOOP('',(#10022,#10023,#10024,#10025));
#2421=EDGE_LOOP('',(#10026,#10027,#10028,#10029));
#2422=EDGE_LOOP('',(#10030,#10031,#10032,#10033));
#2423=EDGE_LOOP('',(#10034,#10035,#10036,#10037));
#2424=EDGE_LOOP('',(#10038,#10039,#10040,#10041));
#2425=EDGE_LOOP('',(#10042,#10043,#10044,#10045));
#2426=EDGE_LOOP('',(#10046,#10047,#10048,#10049));
#2427=EDGE_LOOP('',(#10050,#10051,#10052,#10053));
#2428=EDGE_LOOP('',(#10054,#10055,#10056,#10057));
#2429=EDGE_LOOP('',(#10058,#10059,#10060,#10061));
#2430=EDGE_LOOP('',(#10062,#10063,#10064,#10065));
#2431=EDGE_LOOP('',(#10066,#10067,#10068,#10069));
#2432=EDGE_LOOP('',(#10070,#10071,#10072,#10073));
#2433=EDGE_LOOP('',(#10074,#10075,#10076,#10077));
#2434=EDGE_LOOP('',(#10078,#10079,#10080,#10081));
#2435=EDGE_LOOP('',(#10082,#10083,#10084,#10085));
#2436=EDGE_LOOP('',(#10086,#10087,#10088,#10089));
#2437=EDGE_LOOP('',(#10090,#10091,#10092,#10093));
#2438=EDGE_LOOP('',(#10094,#10095,#10096,#10097));
#2439=EDGE_LOOP('',(#10098,#10099,#10100,#10101));
#2440=EDGE_LOOP('',(#10102,#10103,#10104,#10105));
#2441=EDGE_LOOP('',(#10106,#10107,#10108,#10109));
#2442=EDGE_LOOP('',(#10110,#10111,#10112,#10113));
#2443=EDGE_LOOP('',(#10114,#10115,#10116,#10117));
#2444=EDGE_LOOP('',(#10118,#10119,#10120,#10121));
#2445=EDGE_LOOP('',(#10122,#10123,#10124,#10125));
#2446=EDGE_LOOP('',(#10126,#10127,#10128,#10129));
#2447=EDGE_LOOP('',(#10130,#10131,#10132,#10133));
#2448=EDGE_LOOP('',(#10134,#10135,#10136,#10137));
#2449=EDGE_LOOP('',(#10138,#10139,#10140,#10141));
#2450=EDGE_LOOP('',(#10142,#10143,#10144,#10145));
#2451=EDGE_LOOP('',(#10146,#10147,#10148,#10149));
#2452=EDGE_LOOP('',(#10150,#10151,#10152,#10153));
#2453=EDGE_LOOP('',(#10154,#10155,#10156,#10157));
#2454=EDGE_LOOP('',(#10158,#10159,#10160,#10161));
#2455=EDGE_LOOP('',(#10162,#10163,#10164,#10165));
#2456=EDGE_LOOP('',(#10166,#10167,#10168,#10169));
#2457=EDGE_LOOP('',(#10170,#10171,#10172,#10173));
#2458=EDGE_LOOP('',(#10174,#10175,#10176,#10177));
#2459=EDGE_LOOP('',(#10178,#10179,#10180,#10181));
#2460=EDGE_LOOP('',(#10182,#10183,#10184,#10185));
#2461=EDGE_LOOP('',(#10186,#10187,#10188,#10189));
#2462=EDGE_LOOP('',(#10190,#10191,#10192,#10193));
#2463=EDGE_LOOP('',(#10194,#10195,#10196,#10197));
#2464=EDGE_LOOP('',(#10198,#10199,#10200,#10201));
#2465=EDGE_LOOP('',(#10202,#10203,#10204,#10205));
#2466=EDGE_LOOP('',(#10206,#10207,#10208,#10209));
#2467=EDGE_LOOP('',(#10210,#10211,#10212,#10213));
#2468=EDGE_LOOP('',(#10214,#10215,#10216,#10217,#10218,#10219,#10220,#10221,
#10222,#10223));
#2469=EDGE_LOOP('',(#10224,#10225,#10226,#10227));
#2470=EDGE_LOOP('',(#10228));
#2471=EDGE_LOOP('',(#10229));
#2472=EDGE_LOOP('',(#10230));
#2473=EDGE_LOOP('',(#10231));
#2474=EDGE_LOOP('',(#10232));
#2475=EDGE_LOOP('',(#10233));
#2476=EDGE_LOOP('',(#10234,#10235,#10236,#10237,#10238,#10239,#10240,#10241));
#2477=EDGE_LOOP('',(#10242,#10243,#10244,#10245,#10246,#10247,#10248,#10249));
#2478=EDGE_LOOP('',(#10250,#10251,#10252,#10253));
#2479=EDGE_LOOP('',(#10254,#10255,#10256,#10257,#10258,#10259));
#2480=EDGE_LOOP('',(#10260,#10261,#10262,#10263,#10264));
#2481=EDGE_LOOP('',(#10265,#10266,#10267,#10268,#10269,#10270));
#2482=EDGE_LOOP('',(#10271,#10272,#10273,#10274));
#2483=EDGE_LOOP('',(#10275,#10276,#10277,#10278));
#2484=EDGE_LOOP('',(#10279,#10280,#10281,#10282,#10283,#10284));
#2485=EDGE_LOOP('',(#10285,#10286,#10287,#10288));
#2486=EDGE_LOOP('',(#10289,#10290,#10291,#10292,#10293,#10294));
#2487=EDGE_LOOP('',(#10295,#10296,#10297,#10298));
#2488=EDGE_LOOP('',(#10299,#10300,#10301,#10302,#10303,#10304,#10305));
#2489=EDGE_LOOP('',(#10306,#10307,#10308,#10309,#10310,#10311));
#2490=EDGE_LOOP('',(#10312,#10313,#10314,#10315));
#2491=EDGE_LOOP('',(#10316,#10317,#10318,#10319,#10320,#10321,#10322));
#2492=EDGE_LOOP('',(#10323,#10324,#10325,#10326));
#2493=EDGE_LOOP('',(#10327,#10328,#10329,#10330));
#2494=EDGE_LOOP('',(#10331,#10332,#10333,#10334,#10335,#10336,#10337,#10338,
#10339,#10340,#10341,#10342,#10343,#10344,#10345,#10346,#10347,#10348,#10349,
#10350,#10351,#10352,#10353,#10354,#10355,#10356,#10357));
#2495=EDGE_LOOP('',(#10358,#10359,#10360,#10361));
#2496=EDGE_LOOP('',(#10362,#10363,#10364,#10365));
#2497=EDGE_LOOP('',(#10366,#10367,#10368,#10369));
#2498=EDGE_LOOP('',(#10370,#10371,#10372,#10373));
#2499=EDGE_LOOP('',(#10374,#10375,#10376));
#2500=EDGE_LOOP('',(#10377,#10378,#10379,#10380,#10381,#10382,#10383,#10384,
#10385,#10386,#10387,#10388,#10389,#10390,#10391,#10392,#10393,#10394,#10395,
#10396,#10397,#10398,#10399,#10400,#10401,#10402,#10403,#10404,#10405,#10406,
#10407,#10408,#10409));
#2501=EDGE_LOOP('',(#10410,#10411,#10412));
#2502=EDGE_LOOP('',(#10413,#10414,#10415,#10416));
#2503=EDGE_LOOP('',(#10417,#10418,#10419,#10420,#10421));
#2504=EDGE_LOOP('',(#10422,#10423,#10424,#10425,#10426));
#2505=EDGE_LOOP('',(#10427,#10428,#10429,#10430,#10431,#10432));
#2506=EDGE_LOOP('',(#10433,#10434,#10435,#10436,#10437,#10438));
#2507=EDGE_LOOP('',(#10439,#10440,#10441,#10442));
#2508=EDGE_LOOP('',(#10443,#10444,#10445,#10446,#10447));
#2509=EDGE_LOOP('',(#10448,#10449,#10450,#10451,#10452));
#2510=EDGE_LOOP('',(#10453,#10454,#10455,#10456));
#2511=EDGE_LOOP('',(#10457,#10458,#10459,#10460,#10461));
#2512=EDGE_LOOP('',(#10462,#10463,#10464,#10465,#10466));
#2513=EDGE_LOOP('',(#10467,#10468,#10469,#10470));
#2514=EDGE_LOOP('',(#10471,#10472,#10473,#10474,#10475));
#2515=EDGE_LOOP('',(#10476,#10477,#10478,#10479,#10480));
#2516=EDGE_LOOP('',(#10481,#10482,#10483,#10484));
#2517=EDGE_LOOP('',(#10485,#10486,#10487,#10488,#10489));
#2518=EDGE_LOOP('',(#10490,#10491,#10492,#10493,#10494));
#2519=EDGE_LOOP('',(#10495,#10496,#10497,#10498));
#2520=EDGE_LOOP('',(#10499,#10500,#10501,#10502,#10503));
#2521=EDGE_LOOP('',(#10504,#10505,#10506,#10507,#10508));
#2522=EDGE_LOOP('',(#10509,#10510,#10511,#10512));
#2523=EDGE_LOOP('',(#10513));
#2524=EDGE_LOOP('',(#10514));
#2525=EDGE_LOOP('',(#10515));
#2526=EDGE_LOOP('',(#10516,#10517,#10518));
#2527=EDGE_LOOP('',(#10519,#10520,#10521));
#2528=EDGE_LOOP('',(#10522,#10523,#10524));
#2529=EDGE_LOOP('',(#10525,#10526,#10527));
#2530=EDGE_LOOP('',(#10528,#10529,#10530));
#2531=EDGE_LOOP('',(#10531,#10532,#10533));
#2532=EDGE_LOOP('',(#10534));
#2533=EDGE_LOOP('',(#10535));
#2534=EDGE_LOOP('',(#10536));
#2535=EDGE_LOOP('',(#10537));
#2536=EDGE_LOOP('',(#10538));
#2537=LINE('',#16379,#2975);
#2538=LINE('',#16385,#2976);
#2539=LINE('',#16391,#2977);
#2540=LINE('',#16397,#2978);
#2541=LINE('',#16668,#2979);
#2542=LINE('',#16671,#2980);
#2543=LINE('',#16677,#2981);
#2544=LINE('',#16680,#2982);
#2545=LINE('',#16686,#2983);
#2546=LINE('',#16689,#2984);
#2547=LINE('',#16701,#2985);
#2548=LINE('',#16704,#2986);
#2549=LINE('',#16710,#2987);
#2550=LINE('',#16713,#2988);
#2551=LINE('',#16719,#2989);
#2552=LINE('',#16722,#2990);
#2553=LINE('',#16728,#2991);
#2554=LINE('',#16731,#2992);
#2555=LINE('',#16764,#2993);
#2556=LINE('',#16767,#2994);
#2557=LINE('',#16771,#2995);
#2558=LINE('',#16774,#2996);
#2559=LINE('',#16776,#2997);
#2560=LINE('',#16778,#2998);
#2561=LINE('',#16781,#2999);
#2562=LINE('',#16784,#3000);
#2563=LINE('',#16790,#3001);
#2564=LINE('',#16793,#3002);
#2565=LINE('',#16798,#3003);
#2566=LINE('',#16800,#3004);
#2567=LINE('',#16802,#3005);
#2568=LINE('',#16804,#3006);
#2569=LINE('',#16851,#3007);
#2570=LINE('',#16854,#3008);
#2571=LINE('',#16860,#3009);
#2572=LINE('',#16863,#3010);
#2573=LINE('',#16865,#3011);
#2574=LINE('',#16866,#3012);
#2575=LINE('',#16868,#3013);
#2576=LINE('',#16870,#3014);
#2577=LINE('',#16922,#3015);
#2578=LINE('',#16923,#3016);
#2579=LINE('',#16925,#3017);
#2580=LINE('',#16926,#3018);
#2581=LINE('',#16928,#3019);
#2582=LINE('',#16929,#3020);
#2583=LINE('',#16945,#3021);
#2584=LINE('',#16998,#3022);
#2585=LINE('',#17002,#3023);
#2586=LINE('',#17073,#3024);
#2587=LINE('',#17175,#3025);
#2588=LINE('',#17247,#3026);
#2589=LINE('',#17251,#3027);
#2590=LINE('',#17352,#3028);
#2591=LINE('',#17356,#3029);
#2592=LINE('',#17428,#3030);
#2593=LINE('',#17530,#3031);
#2594=LINE('',#17601,#3032);
#2595=LINE('',#17605,#3033);
#2596=LINE('',#17665,#3034);
#2597=LINE('',#17667,#3035);
#2598=LINE('',#17719,#3036);
#2599=LINE('',#17720,#3037);
#2600=LINE('',#17726,#3038);
#2601=LINE('',#17729,#3039);
#2602=LINE('',#17733,#3040);
#2603=LINE('',#17735,#3041);
#2604=LINE('',#17737,#3042);
#2605=LINE('',#17738,#3043);
#2606=LINE('',#17744,#3044);
#2607=LINE('',#17752,#3045);
#2608=LINE('',#17754,#3046);
#2609=LINE('',#17756,#3047);
#2610=LINE('',#17758,#3048);
#2611=LINE('',#17762,#3049);
#2612=LINE('',#17766,#3050);
#2613=LINE('',#17770,#3051);
#2614=LINE('',#17778,#3052);
#2615=LINE('',#17783,#3053);
#2616=LINE('',#17790,#3054);
#2617=LINE('',#17794,#3055);
#2618=LINE('',#17798,#3056);
#2619=LINE('',#17803,#3057);
#2620=LINE('',#17827,#3058);
#2621=LINE('',#17871,#3059);
#2622=LINE('',#17904,#3060);
#2623=LINE('',#17947,#3061);
#2624=LINE('',#17951,#3062);
#2625=LINE('',#17953,#3063);
#2626=LINE('',#17955,#3064);
#2627=LINE('',#17956,#3065);
#2628=LINE('',#17960,#3066);
#2629=LINE('',#17962,#3067);
#2630=LINE('',#17964,#3068);
#2631=LINE('',#17965,#3069);
#2632=LINE('',#17969,#3070);
#2633=LINE('',#17971,#3071);
#2634=LINE('',#17973,#3072);
#2635=LINE('',#17975,#3073);
#2636=LINE('',#17977,#3074);
#2637=LINE('',#17979,#3075);
#2638=LINE('',#17981,#3076);
#2639=LINE('',#17985,#3077);
#2640=LINE('',#17989,#3078);
#2641=LINE('',#17993,#3079);
#2642=LINE('',#17997,#3080);
#2643=LINE('',#17999,#3081);
#2644=LINE('',#18001,#3082);
#2645=LINE('',#18002,#3083);
#2646=LINE('',#18006,#3084);
#2647=LINE('',#18008,#3085);
#2648=LINE('',#18012,#3086);
#2649=LINE('',#18015,#3087);
#2650=LINE('',#18017,#3088);
#2651=LINE('',#18021,#3089);
#2652=LINE('',#18023,#3090);
#2653=LINE('',#18025,#3091);
#2654=LINE('',#18027,#3092);
#2655=LINE('',#18029,#3093);
#2656=LINE('',#18031,#3094);
#2657=LINE('',#18032,#3095);
#2658=LINE('',#18036,#3096);
#2659=LINE('',#18037,#3097);
#2660=LINE('',#18038,#3098);
#2661=LINE('',#18039,#3099);
#2662=LINE('',#18049,#3100);
#2663=LINE('',#18060,#3101);
#2664=LINE('',#18064,#3102);
#2665=LINE('',#18066,#3103);
#2666=LINE('',#18068,#3104);
#2667=LINE('',#18069,#3105);
#2668=LINE('',#18074,#3106);
#2669=LINE('',#18081,#3107);
#2670=LINE('',#18085,#3108);
#2671=LINE('',#18091,#3109);
#2672=LINE('',#18092,#3110);
#2673=LINE('',#18132,#3111);
#2674=LINE('',#18209,#3112);
#2675=LINE('',#18289,#3113);
#2676=LINE('',#18363,#3114);
#2677=LINE('',#18474,#3115);
#2678=LINE('',#18475,#3116);
#2679=LINE('',#18481,#3117);
#2680=LINE('',#18485,#3118);
#2681=LINE('',#18491,#3119);
#2682=LINE('',#18495,#3120);
#2683=LINE('',#18501,#3121);
#2684=LINE('',#18504,#3122);
#2685=LINE('',#18508,#3123);
#2686=LINE('',#18512,#3124);
#2687=LINE('',#18513,#3125);
#2688=LINE('',#18515,#3126);
#2689=LINE('',#18522,#3127);
#2690=LINE('',#18523,#3128);
#2691=LINE('',#18560,#3129);
#2692=LINE('',#18563,#3130);
#2693=LINE('',#18567,#3131);
#2694=LINE('',#18569,#3132);
#2695=LINE('',#18571,#3133);
#2696=LINE('',#18573,#3134);
#2697=LINE('',#18577,#3135);
#2698=LINE('',#18781,#3136);
#2699=LINE('',#18785,#3137);
#2700=LINE('',#18793,#3138);
#2701=LINE('',#18797,#3139);
#2702=LINE('',#18833,#3140);
#2703=LINE('',#18837,#3141);
#2704=LINE('',#18885,#3142);
#2705=LINE('',#18889,#3143);
#2706=LINE('',#18892,#3144);
#2707=LINE('',#18894,#3145);
#2708=LINE('',#18899,#3146);
#2709=LINE('',#18903,#3147);
#2710=LINE('',#18907,#3148);
#2711=LINE('',#18911,#3149);
#2712=LINE('',#18936,#3150);
#2713=LINE('',#18938,#3151);
#2714=LINE('',#18940,#3152);
#2715=LINE('',#18942,#3153);
#2716=LINE('',#18944,#3154);
#2717=LINE('',#19029,#3155);
#2718=LINE('',#19031,#3156);
#2719=LINE('',#19150,#3157);
#2720=LINE('',#19152,#3158);
#2721=LINE('',#19153,#3159);
#2722=LINE('',#19160,#3160);
#2723=LINE('',#19162,#3161);
#2724=LINE('',#19227,#3162);
#2725=LINE('',#19229,#3163);
#2726=LINE('',#19230,#3164);
#2727=LINE('',#19248,#3165);
#2728=LINE('',#19250,#3166);
#2729=LINE('',#19252,#3167);
#2730=LINE('',#19254,#3168);
#2731=LINE('',#19256,#3169);
#2732=LINE('',#19293,#3170);
#2733=LINE('',#19295,#3171);
#2734=LINE('',#19297,#3172);
#2735=LINE('',#19299,#3173);
#2736=LINE('',#19301,#3174);
#2737=LINE('',#19303,#3175);
#2738=LINE('',#19383,#3176);
#2739=LINE('',#19452,#3177);
#2740=LINE('',#19457,#3178);
#2741=LINE('',#19459,#3179);
#2742=LINE('',#19461,#3180);
#2743=LINE('',#19463,#3181);
#2744=LINE('',#19465,#3182);
#2745=LINE('',#19466,#3183);
#2746=LINE('',#19470,#3184);
#2747=LINE('',#19474,#3185);
#2748=LINE('',#19478,#3186);
#2749=LINE('',#19540,#3187);
#2750=LINE('',#19546,#3188);
#2751=LINE('',#19629,#3189);
#2752=LINE('',#19698,#3190);
#2753=LINE('',#19701,#3191);
#2754=LINE('',#19784,#3192);
#2755=LINE('',#19799,#3193);
#2756=LINE('',#19882,#3194);
#2757=LINE('',#19950,#3195);
#2758=LINE('',#20017,#3196);
#2759=LINE('',#20091,#3197);
#2760=LINE('',#20139,#3198);
#2761=LINE('',#20141,#3199);
#2762=LINE('',#20142,#3200);
#2763=LINE('',#20145,#3201);
#2764=LINE('',#20154,#3202);
#2765=LINE('',#20156,#3203);
#2766=LINE('',#20157,#3204);
#2767=LINE('',#20161,#3205);
#2768=LINE('',#20165,#3206);
#2769=LINE('',#20170,#3207);
#2770=LINE('',#20174,#3208);
#2771=LINE('',#20179,#3209);
#2772=LINE('',#20188,#3210);
#2773=LINE('',#20192,#3211);
#2774=LINE('',#20196,#3212);
#2775=LINE('',#20201,#3213);
#2776=LINE('',#20207,#3214);
#2777=LINE('',#20212,#3215);
#2778=LINE('',#20217,#3216);
#2779=LINE('',#20218,#3217);
#2780=LINE('',#20219,#3218);
#2781=LINE('',#20223,#3219);
#2782=LINE('',#20225,#3220);
#2783=LINE('',#20227,#3221);
#2784=LINE('',#20228,#3222);
#2785=LINE('',#20232,#3223);
#2786=LINE('',#20238,#3224);
#2787=LINE('',#20321,#3225);
#2788=LINE('',#20323,#3226);
#2789=LINE('',#20325,#3227);
#2790=LINE('',#20362,#3228);
#2791=LINE('',#20365,#3229);
#2792=LINE('',#20368,#3230);
#2793=LINE('',#20370,#3231);
#2794=LINE('',#20372,#3232);
#2795=LINE('',#20376,#3233);
#2796=LINE('',#20534,#3234);
#2797=LINE('',#20538,#3235);
#2798=LINE('',#20543,#3236);
#2799=LINE('',#20547,#3237);
#2800=LINE('',#20595,#3238);
#2801=LINE('',#20599,#3239);
#2802=LINE('',#20602,#3240);
#2803=LINE('',#20604,#3241);
#2804=LINE('',#20609,#3242);
#2805=LINE('',#20613,#3243);
#2806=LINE('',#20617,#3244);
#2807=LINE('',#20621,#3245);
#2808=LINE('',#20626,#3246);
#2809=LINE('',#20628,#3247);
#2810=LINE('',#20630,#3248);
#2811=LINE('',#20632,#3249);
#2812=LINE('',#20634,#3250);
#2813=LINE('',#20742,#3251);
#2814=LINE('',#20744,#3252);
#2815=LINE('',#20746,#3253);
#2816=LINE('',#20811,#3254);
#2817=LINE('',#20812,#3255);
#2818=LINE('',#20879,#3256);
#2819=LINE('',#20925,#3257);
#2820=LINE('',#20927,#3258);
#2821=LINE('',#20929,#3259);
#2822=LINE('',#20930,#3260);
#2823=LINE('',#20933,#3261);
#2824=LINE('',#20941,#3262);
#2825=LINE('',#20942,#3263);
#2826=LINE('',#20945,#3264);
#2827=LINE('',#20951,#3265);
#2828=LINE('',#20955,#3266);
#2829=LINE('',#20960,#3267);
#2830=LINE('',#20969,#3268);
#2831=LINE('',#20973,#3269);
#2832=LINE('',#20977,#3270);
#2833=LINE('',#20982,#3271);
#2834=LINE('',#20988,#3272);
#2835=LINE('',#20991,#3273);
#2836=LINE('',#20996,#3274);
#2837=LINE('',#20997,#3275);
#2838=LINE('',#20998,#3276);
#2839=LINE('',#21000,#3277);
#2840=LINE('',#21002,#3278);
#2841=LINE('',#21004,#3279);
#2842=LINE('',#21005,#3280);
#2843=LINE('',#21010,#3281);
#2844=LINE('',#21015,#3282);
#2845=LINE('',#21097,#3283);
#2846=LINE('',#21099,#3284);
#2847=LINE('',#21101,#3285);
#2848=LINE('',#21103,#3286);
#2849=LINE('',#21140,#3287);
#2850=LINE('',#21145,#3288);
#2851=LINE('',#21147,#3289);
#2852=LINE('',#21149,#3290);
#2853=LINE('',#21151,#3291);
#2854=LINE('',#21155,#3292);
#2855=LINE('',#21311,#3293);
#2856=LINE('',#21312,#3294);
#2857=LINE('',#21315,#3295);
#2858=LINE('',#21317,#3296);
#2859=LINE('',#21385,#3297);
#2860=LINE('',#21387,#3298);
#2861=LINE('',#21389,#3299);
#2862=LINE('',#21391,#3300);
#2863=LINE('',#21393,#3301);
#2864=LINE('',#21481,#3302);
#2865=LINE('',#21483,#3303);
#2866=LINE('',#21548,#3304);
#2867=LINE('',#21550,#3305);
#2868=LINE('',#21551,#3306);
#2869=LINE('',#21618,#3307);
#2870=LINE('',#21664,#3308);
#2871=LINE('',#21666,#3309);
#2872=LINE('',#21668,#3310);
#2873=LINE('',#21669,#3311);
#2874=LINE('',#21672,#3312);
#2875=LINE('',#21681,#3313);
#2876=LINE('',#21683,#3314);
#2877=LINE('',#21684,#3315);
#2878=LINE('',#21688,#3316);
#2879=LINE('',#21694,#3317);
#2880=LINE('',#21698,#3318);
#2881=LINE('',#21703,#3319);
#2882=LINE('',#21712,#3320);
#2883=LINE('',#21716,#3321);
#2884=LINE('',#21720,#3322);
#2885=LINE('',#21728,#3323);
#2886=LINE('',#21733,#3324);
#2887=LINE('',#21737,#3325);
#2888=LINE('',#21739,#3326);
#2889=LINE('',#21740,#3327);
#2890=LINE('',#21744,#3328);
#2891=LINE('',#21746,#3329);
#2892=LINE('',#21748,#3330);
#2893=LINE('',#21749,#3331);
#2894=LINE('',#21753,#3332);
#2895=LINE('',#21755,#3333);
#2896=LINE('',#21763,#3334);
#2897=LINE('',#21768,#3335);
#2898=LINE('',#21769,#3336);
#2899=LINE('',#21849,#3337);
#2900=LINE('',#21851,#3338);
#2901=LINE('',#21888,#3339);
#2902=LINE('',#21891,#3340);
#2903=LINE('',#21895,#3341);
#2904=LINE('',#21896,#3342);
#2905=LINE('',#21898,#3343);
#2906=LINE('',#21902,#3344);
#2907=LINE('',#22060,#3345);
#2908=LINE('',#22064,#3346);
#2909=LINE('',#22068,#3347);
#2910=LINE('',#22072,#3348);
#2911=LINE('',#22077,#3349);
#2912=LINE('',#22081,#3350);
#2913=LINE('',#22084,#3351);
#2914=LINE('',#22086,#3352);
#2915=LINE('',#22126,#3353);
#2916=LINE('',#22128,#3354);
#2917=LINE('',#22130,#3355);
#2918=LINE('',#22131,#3356);
#2919=LINE('',#22134,#3357);
#2920=LINE('',#22143,#3358);
#2921=LINE('',#22145,#3359);
#2922=LINE('',#22146,#3360);
#2923=LINE('',#22153,#3361);
#2924=LINE('',#22157,#3362);
#2925=LINE('',#22161,#3363);
#2926=LINE('',#22172,#3364);
#2927=LINE('',#22176,#3365);
#2928=LINE('',#22181,#3366);
#2929=LINE('',#22187,#3367);
#2930=LINE('',#22192,#3368);
#2931=LINE('',#22197,#3369);
#2932=LINE('',#22198,#3370);
#2933=LINE('',#22199,#3371);
#2934=LINE('',#22203,#3372);
#2935=LINE('',#22204,#3373);
#2936=LINE('',#22205,#3374);
#2937=LINE('',#22206,#3375);
#2938=LINE('',#22213,#3376);
#2939=LINE('',#22220,#3377);
#2940=LINE('',#32144,#3378);
#2941=LINE('',#32145,#3379);
#2942=LINE('',#32147,#3380);
#2943=LINE('',#32148,#3381);
#2944=LINE('',#32150,#3382);
#2945=LINE('',#32151,#3383);
#2946=LINE('',#32153,#3384);
#2947=LINE('',#32154,#3385);
#2948=LINE('',#32161,#3386);
#2949=LINE('',#32162,#3387);
#2950=LINE('',#32165,#3388);
#2951=LINE('',#32166,#3389);
#2952=LINE('',#32169,#3390);
#2953=LINE('',#32170,#3391);
#2954=LINE('',#32172,#3392);
#2955=LINE('',#32174,#3393);
#2956=LINE('',#32176,#3394);
#2957=LINE('',#32178,#3395);
#2958=LINE('',#32182,#3396);
#2959=LINE('',#32184,#3397);
#2960=LINE('',#32186,#3398);
#2961=LINE('',#32188,#3399);
#2962=LINE('',#32190,#3400);
#2963=LINE('',#32192,#3401);
#2964=LINE('',#32200,#3402);
#2965=LINE('',#32361,#3403);
#2966=LINE('',#32381,#3404);
#2967=LINE('',#32391,#3405);
#2968=LINE('',#32407,#3406);
#2969=LINE('',#32749,#3407);
#2970=LINE('',#34071,#3408);
#2971=LINE('',#34782,#3409);
#2972=LINE('',#35493,#3410);
#2973=LINE('',#36893,#3411);
#2974=LINE('',#37604,#3412);
#2975=VECTOR('',#13001,2.1875);
#2976=VECTOR('',#13008,2.5625);
#2977=VECTOR('',#13015,3.4375);
#2978=VECTOR('',#13022,1.3125);
#2979=VECTOR('',#13341,1000.);
#2980=VECTOR('',#13344,1000.);
#2981=VECTOR('',#13349,1000.);
#2982=VECTOR('',#13352,1000.);
#2983=VECTOR('',#13357,1000.);
#2984=VECTOR('',#13360,1000.);
#2985=VECTOR('',#13373,1000.);
#2986=VECTOR('',#13376,1000.);
#2987=VECTOR('',#13381,1000.);
#2988=VECTOR('',#13384,1000.);
#2989=VECTOR('',#13389,1000.);
#2990=VECTOR('',#13392,1000.);
#2991=VECTOR('',#13397,1000.);
#2992=VECTOR('',#13400,1000.);
#2993=VECTOR('',#13435,1000.);
#2994=VECTOR('',#13438,1000.);
#2995=VECTOR('',#13443,1000.);
#2996=VECTOR('',#13446,1000.);
#2997=VECTOR('',#13449,2.8125);
#2998=VECTOR('',#13452,2.8125);
#2999=VECTOR('',#13455,1000.);
#3000=VECTOR('',#13458,1000.);
#3001=VECTOR('',#13463,1000.);
#3002=VECTOR('',#13466,1000.);
#3003=VECTOR('',#13471,1000.);
#3004=VECTOR('',#13474,1000.);
#3005=VECTOR('',#13477,2.8125);
#3006=VECTOR('',#13480,2.8125);
#3007=VECTOR('',#13489,1000.);
#3008=VECTOR('',#13492,1000.);
#3009=VECTOR('',#13497,1000.);
#3010=VECTOR('',#13500,1000.);
#3011=VECTOR('',#13503,1000.);
#3012=VECTOR('',#13504,1000.);
#3013=VECTOR('',#13507,2.8125);
#3014=VECTOR('',#13510,2.8125);
#3015=VECTOR('',#13523,1000.);
#3016=VECTOR('',#13524,1000.);
#3017=VECTOR('',#13527,1000.);
#3018=VECTOR('',#13528,1000.);
#3019=VECTOR('',#13531,1000.);
#3020=VECTOR('',#13532,1000.);
#3021=VECTOR('',#13547,48.4375);
#3022=VECTOR('',#13552,1000.);
#3023=VECTOR('',#13555,1000.);
#3024=VECTOR('',#13558,1000.);
#3025=VECTOR('',#13569,1000.);
#3026=VECTOR('',#13574,1000.);
#3027=VECTOR('',#13577,1000.);
#3028=VECTOR('',#13586,1000.);
#3029=VECTOR('',#13589,1000.);
#3030=VECTOR('',#13594,1000.);
#3031=VECTOR('',#13605,1000.);
#3032=VECTOR('',#13608,1000.);
#3033=VECTOR('',#13611,1000.);
#3034=VECTOR('',#13630,2.8125);
#3035=VECTOR('',#13633,2.8125);
#3036=VECTOR('',#13646,1000.);
#3037=VECTOR('',#13647,1000.);
#3038=VECTOR('',#13652,1000.);
#3039=VECTOR('',#13655,1000.);
#3040=VECTOR('',#13658,1000.);
#3041=VECTOR('',#13659,1000.);
#3042=VECTOR('',#13660,1000.);
#3043=VECTOR('',#13661,1000.);
#3044=VECTOR('',#13666,1000.);
#3045=VECTOR('',#13673,1000.);
#3046=VECTOR('',#13674,1000.);
#3047=VECTOR('',#13675,1000.);
#3048=VECTOR('',#13676,1000.);
#3049=VECTOR('',#13679,1000.);
#3050=VECTOR('',#13682,1000.);
#3051=VECTOR('',#13685,1000.);
#3052=VECTOR('',#13692,1000.);
#3053=VECTOR('',#13697,1000.);
#3054=VECTOR('',#13704,1000.);
#3055=VECTOR('',#13709,1000.);
#3056=VECTOR('',#13712,1000.);
#3057=VECTOR('',#13717,1000.);
#3058=VECTOR('',#13722,1000.);
#3059=VECTOR('',#13725,1000.);
#3060=VECTOR('',#13728,1000.);
#3061=VECTOR('',#13731,1000.);
#3062=VECTOR('',#13734,1000.);
#3063=VECTOR('',#13735,1000.);
#3064=VECTOR('',#13736,1000.);
#3065=VECTOR('',#13737,1000.);
#3066=VECTOR('',#13740,1000.);
#3067=VECTOR('',#13741,1000.);
#3068=VECTOR('',#13742,1000.);
#3069=VECTOR('',#13743,1000.);
#3070=VECTOR('',#13746,1000.);
#3071=VECTOR('',#13747,1000.);
#3072=VECTOR('',#13748,1000.);
#3073=VECTOR('',#13749,1000.);
#3074=VECTOR('',#13750,1000.);
#3075=VECTOR('',#13751,1000.);
#3076=VECTOR('',#13752,1000.);
#3077=VECTOR('',#13755,1000.);
#3078=VECTOR('',#13758,1000.);
#3079=VECTOR('',#13761,1000.);
#3080=VECTOR('',#13764,1000.);
#3081=VECTOR('',#13765,1000.);
#3082=VECTOR('',#13766,1000.);
#3083=VECTOR('',#13767,1000.);
#3084=VECTOR('',#13770,1000.);
#3085=VECTOR('',#13771,1000.);
#3086=VECTOR('',#13774,1000.);
#3087=VECTOR('',#13777,1000.);
#3088=VECTOR('',#13778,1000.);
#3089=VECTOR('',#13781,1000.);
#3090=VECTOR('',#13782,1000.);
#3091=VECTOR('',#13783,1000.);
#3092=VECTOR('',#13784,1000.);
#3093=VECTOR('',#13785,1000.);
#3094=VECTOR('',#13786,1000.);
#3095=VECTOR('',#13787,1000.);
#3096=VECTOR('',#13790,1000.);
#3097=VECTOR('',#13791,1000.);
#3098=VECTOR('',#13792,1000.);
#3099=VECTOR('',#13793,1000.);
#3100=VECTOR('',#13808,1000.);
#3101=VECTOR('',#13827,1000.);
#3102=VECTOR('',#13830,1000.);
#3103=VECTOR('',#13831,1000.);
#3104=VECTOR('',#13832,1000.);
#3105=VECTOR('',#13833,1000.);
#3106=VECTOR('',#13838,1000.);
#3107=VECTOR('',#13847,1000.);
#3108=VECTOR('',#13850,1000.);
#3109=VECTOR('',#13855,1000.);
#3110=VECTOR('',#13856,1000.);
#3111=VECTOR('',#13863,1000.);
#3112=VECTOR('',#13870,1000.);
#3113=VECTOR('',#13877,1000.);
#3114=VECTOR('',#13884,1000.);
#3115=VECTOR('',#13899,1000.);
#3116=VECTOR('',#13900,1000.);
#3117=VECTOR('',#13905,1000.);
#3118=VECTOR('',#13908,1000.);
#3119=VECTOR('',#13913,1000.);
#3120=VECTOR('',#13916,1000.);
#3121=VECTOR('',#13921,1000.);
#3122=VECTOR('',#13924,1000.);
#3123=VECTOR('',#13927,1000.);
#3124=VECTOR('',#13930,1000.);
#3125=VECTOR('',#13931,1000.);
#3126=VECTOR('',#13932,1000.);
#3127=VECTOR('',#13939,1000.);
#3128=VECTOR('',#13940,1000.);
#3129=VECTOR('',#13941,1000.);
#3130=VECTOR('',#13944,1000.);
#3131=VECTOR('',#13947,1000.);
#3132=VECTOR('',#13948,1000.);
#3133=VECTOR('',#13949,1000.);
#3134=VECTOR('',#13950,1000.);
#3135=VECTOR('',#13953,1000.);
#3136=VECTOR('',#13974,1000.);
#3137=VECTOR('',#13977,1000.);
#3138=VECTOR('',#13988,10.);
#3139=VECTOR('',#13991,10.);
#3140=VECTOR('',#13998,10.);
#3141=VECTOR('',#14001,10.);
#3142=VECTOR('',#14008,1000.);
#3143=VECTOR('',#14011,1000.);
#3144=VECTOR('',#14014,1000.);
#3145=VECTOR('',#14015,1000.);
#3146=VECTOR('',#14020,1000.);
#3147=VECTOR('',#14023,1000.);
#3148=VECTOR('',#14026,1000.);
#3149=VECTOR('',#14029,1000.);
#3150=VECTOR('',#14034,1000.);
#3151=VECTOR('',#14035,1000.);
#3152=VECTOR('',#14036,1000.);
#3153=VECTOR('',#14037,1000.);
#3154=VECTOR('',#14038,1000.);
#3155=VECTOR('',#14041,1000.);
#3156=VECTOR('',#14042,1000.);
#3157=VECTOR('',#14043,1000.);
#3158=VECTOR('',#14044,1000.);
#3159=VECTOR('',#14045,1000.);
#3160=VECTOR('',#14054,1000.);
#3161=VECTOR('',#14055,1000.);
#3162=VECTOR('',#14056,1000.);
#3163=VECTOR('',#14057,1000.);
#3164=VECTOR('',#14058,1000.);
#3165=VECTOR('',#14061,1000.);
#3166=VECTOR('',#14062,1000.);
#3167=VECTOR('',#14063,1000.);
#3168=VECTOR('',#14064,1000.);
#3169=VECTOR('',#14065,1000.);
#3170=VECTOR('',#14068,1000.);
#3171=VECTOR('',#14069,1000.);
#3172=VECTOR('',#14070,1000.);
#3173=VECTOR('',#14071,1000.);
#3174=VECTOR('',#14072,1000.);
#3175=VECTOR('',#14073,1000.);
#3176=VECTOR('',#14076,1000.);
#3177=VECTOR('',#14079,1000.);
#3178=VECTOR('',#14084,1000.);
#3179=VECTOR('',#14085,1000.);
#3180=VECTOR('',#14086,1000.);
#3181=VECTOR('',#14087,1000.);
#3182=VECTOR('',#14088,1000.);
#3183=VECTOR('',#14089,1000.);
#3184=VECTOR('',#14092,1000.);
#3185=VECTOR('',#14095,1000.);
#3186=VECTOR('',#14098,1000.);
#3187=VECTOR('',#14103,1000.);
#3188=VECTOR('',#14108,1000.);
#3189=VECTOR('',#14111,1000.);
#3190=VECTOR('',#14114,1000.);
#3191=VECTOR('',#14117,1000.);
#3192=VECTOR('',#14120,1000.);
#3193=VECTOR('',#14125,1000.);
#3194=VECTOR('',#14128,1000.);
#3195=VECTOR('',#14131,1000.);
#3196=VECTOR('',#14148,1000.);
#3197=VECTOR('',#14155,1000.);
#3198=VECTOR('',#14160,1000.);
#3199=VECTOR('',#14161,1000.);
#3200=VECTOR('',#14162,10.);
#3201=VECTOR('',#14165,1000.);
#3202=VECTOR('',#14166,1000.);
#3203=VECTOR('',#14167,10.);
#3204=VECTOR('',#14168,1000.);
#3205=VECTOR('',#14171,1000.);
#3206=VECTOR('',#14174,1000.);
#3207=VECTOR('',#14179,1000.);
#3208=VECTOR('',#14182,1000.);
#3209=VECTOR('',#14187,1000.);
#3210=VECTOR('',#14188,1000.);
#3211=VECTOR('',#14191,1000.);
#3212=VECTOR('',#14194,1000.);
#3213=VECTOR('',#14199,1000.);
#3214=VECTOR('',#14200,1000.);
#3215=VECTOR('',#14205,1000.);
#3216=VECTOR('',#14210,1000.);
#3217=VECTOR('',#14211,1000.);
#3218=VECTOR('',#14212,1000.);
#3219=VECTOR('',#14215,1000.);
#3220=VECTOR('',#14216,1000.);
#3221=VECTOR('',#14217,1000.);
#3222=VECTOR('',#14218,1000.);
#3223=VECTOR('',#14223,1000.);
#3224=VECTOR('',#14228,1000.);
#3225=VECTOR('',#14263,1000.);
#3226=VECTOR('',#14264,1000.);
#3227=VECTOR('',#14265,1000.);
#3228=VECTOR('',#14266,1000.);
#3229=VECTOR('',#14269,1000.);
#3230=VECTOR('',#14272,1000.);
#3231=VECTOR('',#14273,1000.);
#3232=VECTOR('',#14274,1000.);
#3233=VECTOR('',#14277,1000.);
#3234=VECTOR('',#14290,1000.);
#3235=VECTOR('',#14293,1000.);
#3236=VECTOR('',#14298,10.);
#3237=VECTOR('',#14301,10.);
#3238=VECTOR('',#14308,1000.);
#3239=VECTOR('',#14311,1000.);
#3240=VECTOR('',#14314,1000.);
#3241=VECTOR('',#14315,1000.);
#3242=VECTOR('',#14320,1000.);
#3243=VECTOR('',#14323,1000.);
#3244=VECTOR('',#14326,1000.);
#3245=VECTOR('',#14329,1000.);
#3246=VECTOR('',#14334,1000.);
#3247=VECTOR('',#14335,1000.);
#3248=VECTOR('',#14336,1000.);
#3249=VECTOR('',#14337,1000.);
#3250=VECTOR('',#14338,1000.);
#3251=VECTOR('',#14347,1000.);
#3252=VECTOR('',#14348,1000.);
#3253=VECTOR('',#14349,1000.);
#3254=VECTOR('',#14350,1000.);
#3255=VECTOR('',#14351,1000.);
#3256=VECTOR('',#14368,1000.);
#3257=VECTOR('',#14373,1000.);
#3258=VECTOR('',#14374,1000.);
#3259=VECTOR('',#14375,10.);
#3260=VECTOR('',#14376,1000.);
#3261=VECTOR('',#14379,1000.);
#3262=VECTOR('',#14380,10.);
#3263=VECTOR('',#14381,1000.);
#3264=VECTOR('',#14384,1000.);
#3265=VECTOR('',#14391,1000.);
#3266=VECTOR('',#14394,1000.);
#3267=VECTOR('',#14399,1000.);
#3268=VECTOR('',#14400,1000.);
#3269=VECTOR('',#14403,1000.);
#3270=VECTOR('',#14406,1000.);
#3271=VECTOR('',#14411,1000.);
#3272=VECTOR('',#14412,1000.);
#3273=VECTOR('',#14417,1000.);
#3274=VECTOR('',#14422,1000.);
#3275=VECTOR('',#14423,1000.);
#3276=VECTOR('',#14424,1000.);
#3277=VECTOR('',#14427,1000.);
#3278=VECTOR('',#14428,1000.);
#3279=VECTOR('',#14429,1000.);
#3280=VECTOR('',#14430,1000.);
#3281=VECTOR('',#14435,1000.);
#3282=VECTOR('',#14440,1000.);
#3283=VECTOR('',#14471,1000.);
#3284=VECTOR('',#14472,1000.);
#3285=VECTOR('',#14473,1000.);
#3286=VECTOR('',#14474,1000.);
#3287=VECTOR('',#14475,1000.);
#3288=VECTOR('',#14480,1000.);
#3289=VECTOR('',#14481,1000.);
#3290=VECTOR('',#14482,1000.);
#3291=VECTOR('',#14483,1000.);
#3292=VECTOR('',#14486,1000.);
#3293=VECTOR('',#14499,1000.);
#3294=VECTOR('',#14500,1000.);
#3295=VECTOR('',#14503,10.);
#3296=VECTOR('',#14504,10.);
#3297=VECTOR('',#14511,1000.);
#3298=VECTOR('',#14512,1000.);
#3299=VECTOR('',#14513,1000.);
#3300=VECTOR('',#14514,1000.);
#3301=VECTOR('',#14515,1000.);
#3302=VECTOR('',#14524,1000.);
#3303=VECTOR('',#14525,1000.);
#3304=VECTOR('',#14526,1000.);
#3305=VECTOR('',#14527,1000.);
#3306=VECTOR('',#14528,1000.);
#3307=VECTOR('',#14545,1000.);
#3308=VECTOR('',#14550,1000.);
#3309=VECTOR('',#14551,1000.);
#3310=VECTOR('',#14552,10.);
#3311=VECTOR('',#14553,1000.);
#3312=VECTOR('',#14556,1000.);
#3313=VECTOR('',#14557,1000.);
#3314=VECTOR('',#14558,10.);
#3315=VECTOR('',#14559,1000.);
#3316=VECTOR('',#14562,1000.);
#3317=VECTOR('',#14569,1000.);
#3318=VECTOR('',#14572,1000.);
#3319=VECTOR('',#14577,1000.);
#3320=VECTOR('',#14578,1000.);
#3321=VECTOR('',#14581,1000.);
#3322=VECTOR('',#14584,1000.);
#3323=VECTOR('',#14589,1000.);
#3324=VECTOR('',#14594,1000.);
#3325=VECTOR('',#14599,1000.);
#3326=VECTOR('',#14600,1000.);
#3327=VECTOR('',#14601,1000.);
#3328=VECTOR('',#14604,1000.);
#3329=VECTOR('',#14605,1000.);
#3330=VECTOR('',#14606,1000.);
#3331=VECTOR('',#14607,1000.);
#3332=VECTOR('',#14610,1000.);
#3333=VECTOR('',#14611,1000.);
#3334=VECTOR('',#14618,1000.);
#3335=VECTOR('',#14623,1000.);
#3336=VECTOR('',#14624,1000.);
#3337=VECTOR('',#14653,1000.);
#3338=VECTOR('',#14654,1000.);
#3339=VECTOR('',#14655,1000.);
#3340=VECTOR('',#14658,1000.);
#3341=VECTOR('',#14661,1000.);
#3342=VECTOR('',#14662,1000.);
#3343=VECTOR('',#14663,1000.);
#3344=VECTOR('',#14666,1000.);
#3345=VECTOR('',#14679,1000.);
#3346=VECTOR('',#14682,1000.);
#3347=VECTOR('',#14685,1000.);
#3348=VECTOR('',#14688,1000.);
#3349=VECTOR('',#14693,1000.);
#3350=VECTOR('',#14696,1000.);
#3351=VECTOR('',#14699,1000.);
#3352=VECTOR('',#14700,1000.);
#3353=VECTOR('',#14723,1000.);
#3354=VECTOR('',#14724,1000.);
#3355=VECTOR('',#14725,10.);
#3356=VECTOR('',#14726,1000.);
#3357=VECTOR('',#14729,1000.);
#3358=VECTOR('',#14730,1000.);
#3359=VECTOR('',#14731,10.);
#3360=VECTOR('',#14732,1000.);
#3361=VECTOR('',#14741,1000.);
#3362=VECTOR('',#14744,1000.);
#3363=VECTOR('',#14749,1000.);
#3364=VECTOR('',#14752,1000.);
#3365=VECTOR('',#14755,1000.);
#3366=VECTOR('',#14760,1000.);
#3367=VECTOR('',#14761,1000.);
#3368=VECTOR('',#14766,1000.);
#3369=VECTOR('',#14771,1000.);
#3370=VECTOR('',#14772,1000.);
#3371=VECTOR('',#14773,1000.);
#3372=VECTOR('',#14776,1000.);
#3373=VECTOR('',#14777,1000.);
#3374=VECTOR('',#14778,1000.);
#3375=VECTOR('',#14779,1000.);
#3376=VECTOR('',#14786,1000.);
#3377=VECTOR('',#14793,1000.);
#3378=VECTOR('',#16204,1000.);
#3379=VECTOR('',#16205,1000.);
#3380=VECTOR('',#16208,1000.);
#3381=VECTOR('',#16209,1000.);
#3382=VECTOR('',#16212,1000.);
#3383=VECTOR('',#16213,1000.);
#3384=VECTOR('',#16214,1000.);
#3385=VECTOR('',#16215,1000.);
#3386=VECTOR('',#16226,1000.);
#3387=VECTOR('',#16227,1000.);
#3388=VECTOR('',#16232,1000.);
#3389=VECTOR('',#16233,1000.);
#3390=VECTOR('',#16236,1000.);
#3391=VECTOR('',#16237,1000.);
#3392=VECTOR('',#16240,1000.);
#3393=VECTOR('',#16243,1000.);
#3394=VECTOR('',#16246,1000.);
#3395=VECTOR('',#16249,1000.);
#3396=VECTOR('',#16256,1000.);
#3397=VECTOR('',#16259,1000.);
#3398=VECTOR('',#16262,1000.);
#3399=VECTOR('',#16265,1000.);
#3400=VECTOR('',#16268,1000.);
#3401=VECTOR('',#16271,1000.);
#3402=VECTOR('',#16282,21.875);
#3403=VECTOR('',#16299,21.875);
#3404=VECTOR('',#16312,1.875);
#3405=VECTOR('',#16325,20.);
#3406=VECTOR('',#16330,10.);
#3407=VECTOR('',#16341,10.);
#3408=VECTOR('',#16342,10.);
#3409=VECTOR('',#16343,10.);
#3410=VECTOR('',#16344,10.);
#3411=VECTOR('',#16345,10.);
#3412=VECTOR('',#16346,10.);
#3413=CIRCLE('',#11525,2.1875);
#3414=CIRCLE('',#11526,2.1875);
#3415=CIRCLE('',#11528,2.5625);
#3416=CIRCLE('',#11529,2.5625);
#3417=CIRCLE('',#11531,3.4375);
#3418=CIRCLE('',#11532,3.4375);
#3419=CIRCLE('',#11534,1.3125);
#3420=CIRCLE('',#11535,1.3125);
#3421=CIRCLE('',#11537,2.8125);
#3422=CIRCLE('',#11538,2.8125);
#3423=CIRCLE('',#11539,0.3125);
#3424=CIRCLE('',#11540,3.125);
#3425=CIRCLE('',#11542,3.125);
#3426=CIRCLE('',#11543,0.3125);
#3427=CIRCLE('',#11544,2.8125);
#3428=CIRCLE('',#11545,2.8125);
#3429=CIRCLE('',#11547,3.125);
#3430=CIRCLE('',#11548,0.3125);
#3431=CIRCLE('',#11549,2.8125);
#3432=CIRCLE('',#11551,3.125);
#3433=CIRCLE('',#11552,0.3125);
#3434=CIRCLE('',#11553,2.8125);
#3435=CIRCLE('',#11554,2.8125);
#3436=CIRCLE('',#11556,0.625000000000001);
#3437=CIRCLE('',#11557,0.3125);
#3438=CIRCLE('',#11558,0.937500000000001);
#3439=CIRCLE('',#11559,0.312499999999997);
#3440=CIRCLE('',#11561,4.375);
#3441=CIRCLE('',#11562,0.312500000000001);
#3442=CIRCLE('',#11563,4.6875);
#3443=CIRCLE('',#11564,0.312500000000001);
#3444=CIRCLE('',#11566,1.25);
#3445=CIRCLE('',#11567,0.312499999999997);
#3446=CIRCLE('',#11568,0.937500000000001);
#3447=CIRCLE('',#11569,0.3125);
#3448=CIRCLE('',#11571,4.375);
#3449=CIRCLE('',#11572,0.312499999999997);
#3450=CIRCLE('',#11573,4.0625);
#3451=CIRCLE('',#11574,0.312500000000001);
#3452=CIRCLE('',#11576,2.8125);
#3453=CIRCLE('',#11577,2.8125);
#3454=CIRCLE('',#11578,0.3125);
#3455=CIRCLE('',#11579,3.125);
#3456=CIRCLE('',#11581,3.125);
#3457=CIRCLE('',#11582,0.3125);
#3458=CIRCLE('',#11583,2.8125);
#3459=CIRCLE('',#11584,2.8125);
#3460=CIRCLE('',#11586,3.125);
#3461=CIRCLE('',#11587,0.3125);
#3462=CIRCLE('',#11588,2.8125);
#3463=CIRCLE('',#11589,2.8125);
#3464=CIRCLE('',#11591,3.125);
#3465=CIRCLE('',#11592,0.3125);
#3466=CIRCLE('',#11593,2.8125);
#3467=CIRCLE('',#11594,2.8125);
#3468=CIRCLE('',#11596,0.625000000000001);
#3469=CIRCLE('',#11597,0.312499999999997);
#3470=CIRCLE('',#11598,0.937500000000001);
#3471=CIRCLE('',#11599,0.3125);
#3472=CIRCLE('',#11601,4.375);
#3473=CIRCLE('',#11602,0.312500000000001);
#3474=CIRCLE('',#11603,4.6875);
#3475=CIRCLE('',#11604,0.312500000000001);
#3476=CIRCLE('',#11606,1.25);
#3477=CIRCLE('',#11607,0.3125);
#3478=CIRCLE('',#11608,0.937500000000001);
#3479=CIRCLE('',#11609,0.312499999999997);
#3480=CIRCLE('',#11611,4.375);
#3481=CIRCLE('',#11612,0.312500000000001);
#3482=CIRCLE('',#11613,4.0625);
#3483=CIRCLE('',#11614,0.312500000000001);
#3484=CIRCLE('',#11616,2.8125);
#3485=CIRCLE('',#11617,0.3125);
#3486=CIRCLE('',#11618,3.125);
#3487=CIRCLE('',#11620,3.125);
#3488=CIRCLE('',#11621,0.3125);
#3489=CIRCLE('',#11622,2.8125);
#3490=CIRCLE('',#11624,3.125);
#3491=CIRCLE('',#11625,0.3125);
#3492=CIRCLE('',#11626,2.8125);
#3493=CIRCLE('',#11627,2.8125);
#3494=CIRCLE('',#11629,3.125);
#3495=CIRCLE('',#11630,0.3125);
#3496=CIRCLE('',#11631,2.8125);
#3497=CIRCLE('',#11633,0.625000000000001);
#3498=CIRCLE('',#11634,0.312500000000001);
#3499=CIRCLE('',#11635,0.937500000000001);
#3500=CIRCLE('',#11636,0.3125);
#3501=CIRCLE('',#11638,1.25);
#3502=CIRCLE('',#11639,0.3125);
#3503=CIRCLE('',#11640,0.937500000000001);
#3504=CIRCLE('',#11641,0.312500000000001);
#3505=CIRCLE('',#11643,2.8125);
#3506=CIRCLE('',#11644,0.3125);
#3507=CIRCLE('',#11645,3.125);
#3508=CIRCLE('',#11646,2.8125);
#3509=CIRCLE('',#11648,3.125);
#3510=CIRCLE('',#11649,0.3125);
#3511=CIRCLE('',#11650,2.8125);
#3512=CIRCLE('',#11651,2.8125);
#3513=CIRCLE('',#11653,3.125);
#3514=CIRCLE('',#11654,0.3125);
#3515=CIRCLE('',#11655,2.8125);
#3516=CIRCLE('',#11656,2.8125);
#3517=CIRCLE('',#11658,3.125);
#3518=CIRCLE('',#11659,0.3125);
#3519=CIRCLE('',#11660,2.8125);
#3520=CIRCLE('',#11661,2.8125);
#3521=CIRCLE('',#11663,49.6875);
#3522=CIRCLE('',#11664,0.312499999999998);
#3523=CIRCLE('',#11665,49.7790291308792);
#3524=CIRCLE('',#11666,0.312500000000003);
#3525=CIRCLE('',#11668,49.7790291308792);
#3526=CIRCLE('',#11669,0.312499999999998);
#3527=CIRCLE('',#11670,49.6875);
#3528=CIRCLE('',#11671,0.312499999999998);
#3529=CIRCLE('',#11673,1.25);
#3530=CIRCLE('',#11674,0.312500000000001);
#3531=CIRCLE('',#11675,0.937500000000001);
#3532=CIRCLE('',#11676,0.312500000000001);
#3533=CIRCLE('',#11678,1.25);
#3534=CIRCLE('',#11679,0.312500000000001);
#3535=CIRCLE('',#11680,0.937500000000001);
#3536=CIRCLE('',#11681,0.312500000000001);
#3537=CIRCLE('',#11683,1.25);
#3538=CIRCLE('',#11684,0.312500000000001);
#3539=CIRCLE('',#11685,0.937500000000001);
#3540=CIRCLE('',#11686,0.312500000000001);
#3541=CIRCLE('',#11688,1.25);
#3542=CIRCLE('',#11689,0.312500000000001);
#3543=CIRCLE('',#11690,0.937500000000001);
#3544=CIRCLE('',#11691,0.312499999999996);
#3545=CIRCLE('',#11693,0.3125);
#3546=CIRCLE('',#11694,0.3125);
#3547=CIRCLE('',#11696,0.3125);
#3548=CIRCLE('',#11697,0.3125);
#3549=CIRCLE('',#11699,0.3125);
#3550=CIRCLE('',#11700,0.3125);
#3551=CIRCLE('',#11702,0.3125);
#3552=CIRCLE('',#11703,0.625000000000001);
#3553=CIRCLE('',#11704,0.3125);
#3554=CIRCLE('',#11706,0.3125);
#3555=CIRCLE('',#11707,0.3125);
#3556=CIRCLE('',#11709,0.3125);
#3557=CIRCLE('',#11710,0.3125);
#3558=CIRCLE('',#11712,0.3125);
#3559=CIRCLE('',#11713,0.3125);
#3560=CIRCLE('',#11715,0.3125);
#3561=CIRCLE('',#11716,0.3125);
#3562=CIRCLE('',#11718,0.3125);
#3563=CIRCLE('',#11719,0.312499999999999);
#3564=CIRCLE('',#11720,0.625000000000001);
#3565=CIRCLE('',#11721,0.312500000000001);
#3566=CIRCLE('',#11723,0.625000000000001);
#3567=CIRCLE('',#11724,0.3125);
#3568=CIRCLE('',#11725,0.937500000000001);
#3569=CIRCLE('',#11726,0.312500000000001);
#3570=CIRCLE('',#11728,1.25);
#3571=CIRCLE('',#11729,0.312500000000001);
#3572=CIRCLE('',#11730,0.937500000000001);
#3573=CIRCLE('',#11731,0.3125);
#3574=CIRCLE('',#11733,0.937500000000001);
#3575=CIRCLE('',#11734,0.937500000000001);
#3576=CIRCLE('',#11736,4.375);
#3577=CIRCLE('',#11737,4.375);
#3578=CIRCLE('',#11741,0.937500000000001);
#3579=CIRCLE('',#11743,0.937500000000001);
#3580=CIRCLE('',#11744,0.937500000000001);
#3581=CIRCLE('',#11746,4.375);
#3582=CIRCLE('',#11747,4.375);
#3583=CIRCLE('',#11751,54.4084708691208);
#3584=CIRCLE('',#11752,54.4084708691208);
#3585=CIRCLE('',#11754,0.937500000000001);
#3586=CIRCLE('',#11756,0.937500000000001);
#3587=CIRCLE('',#11757,0.937500000000001);
#3588=CIRCLE('',#11762,49.7790291308792);
#3589=CIRCLE('',#11763,54.4084708691208);
#3590=CIRCLE('',#11764,54.4084708691208);
#3591=CIRCLE('',#11766,0.937500000000001);
#3592=CIRCLE('',#11770,48.4374999999919);
#3593=CIRCLE('',#11771,48.4375);
#3594=CIRCLE('',#11772,48.4374999999962);
#3595=CIRCLE('',#11773,48.4374999999878);
#3596=CIRCLE('',#11774,48.4375);
#3597=CIRCLE('',#11775,48.4374999999957);
#3598=CIRCLE('',#11776,48.4375000000006);
#3599=CIRCLE('',#11777,48.4375);
#3600=CIRCLE('',#11778,48.4375);
#3601=CIRCLE('',#11779,48.4375);
#3602=CIRCLE('',#11780,48.4375);
#3603=CIRCLE('',#11781,48.4375);
#3604=CIRCLE('',#11782,48.4374999999921);
#3605=CIRCLE('',#11783,48.4375000000018);
#3606=CIRCLE('',#11784,48.4375);
#3607=CIRCLE('',#11785,48.4375);
#3608=CIRCLE('',#11786,48.4375);
#3609=CIRCLE('',#11787,48.4375);
#3610=CIRCLE('',#11788,48.4375);
#3611=CIRCLE('',#11789,48.4374999999846);
#3612=CIRCLE('',#11790,48.4375000000085);
#3613=CIRCLE('',#11791,48.4375);
#3614=CIRCLE('',#11792,48.4375);
#3615=CIRCLE('',#11793,48.4375);
#3616=CIRCLE('',#11794,48.4375);
#3617=CIRCLE('',#11795,48.4375);
#3618=CIRCLE('',#11796,48.4374999999955);
#3619=CIRCLE('',#11797,48.4374999999898);
#3620=CIRCLE('',#11798,48.4375);
#3621=CIRCLE('',#11799,48.4375);
#3622=CIRCLE('',#11800,48.4375);
#3623=CIRCLE('',#11801,48.4375);
#3624=CIRCLE('',#11802,48.4375);
#3625=CIRCLE('',#11803,48.4375000000021);
#3626=CIRCLE('',#11804,48.4375000000048);
#3627=CIRCLE('',#11805,48.4375);
#3628=CIRCLE('',#11806,48.4375000000005);
#3629=CIRCLE('',#11807,48.4374999999868);
#3630=CIRCLE('',#11808,48.4375);
#3631=CIRCLE('',#11809,48.4375000000012);
#3632=CIRCLE('',#11813,49.7790291308792);
#3633=CIRCLE('',#11814,54.4084708691208);
#3634=CIRCLE('',#11815,54.4084708691208);
#3635=CIRCLE('',#11817,0.937500000000001);
#3636=CIRCLE('',#11819,1.25);
#3637=CIRCLE('',#11820,1.25);
#3638=CIRCLE('',#11822,4.0625);
#3639=CIRCLE('',#11823,1.25);
#3640=CIRCLE('',#11824,1.25);
#3641=CIRCLE('',#11825,54.6875);
#3642=CIRCLE('',#11826,1.25);
#3643=CIRCLE('',#11827,5.3125);
#3644=CIRCLE('',#11828,5.3125);
#3645=CIRCLE('',#11829,5.3125);
#3646=CIRCLE('',#11830,5.3125);
#3647=CIRCLE('',#11831,54.6875);
#3648=CIRCLE('',#11832,1.25);
#3649=CIRCLE('',#11833,1.25);
#3650=CIRCLE('',#11834,4.0625);
#3651=CIRCLE('',#11835,1.25);
#3652=CIRCLE('',#11836,54.6875);
#3653=CIRCLE('',#11837,1.25);
#3654=CIRCLE('',#11838,1.25);
#3655=CIRCLE('',#11839,1.25);
#3656=CIRCLE('',#11840,54.6875);
#3657=CIRCLE('',#11841,1.25);
#3658=CIRCLE('',#11842,1.25);
#3659=CIRCLE('',#11843,1.25);
#3660=CIRCLE('',#11844,53.5669417382416);
#3661=CIRCLE('',#11845,53.5669417382416);
#3662=CIRCLE('',#11846,53.5669417382416);
#3663=CIRCLE('',#11847,53.5669417382416);
#3664=CIRCLE('',#11851,54.6294417382416);
#3665=CIRCLE('',#11852,1.25);
#3666=CIRCLE('',#11853,54.6294417382416);
#3667=CIRCLE('',#11854,5.3125);
#3668=CIRCLE('',#11856,5.3125);
#3669=CIRCLE('',#11857,50.8794417382416);
#3670=CIRCLE('',#11858,50.8794417382416);
#3671=CIRCLE('',#11861,0.3125);
#3672=CIRCLE('',#11862,0.3125);
#3673=CIRCLE('',#11864,0.3125);
#3674=CIRCLE('',#11865,0.3125);
#3675=CIRCLE('',#11867,0.3125);
#3676=CIRCLE('',#11868,0.3125);
#3677=CIRCLE('',#11870,0.3125);
#3678=CIRCLE('',#11871,0.3125);
#3679=CIRCLE('',#11873,0.3125);
#3680=CIRCLE('',#11875,0.3125);
#3681=CIRCLE('',#11878,0.312499999999999);
#3682=CIRCLE('',#11879,0.312499999999999);
#3683=CIRCLE('',#11881,0.312499999999999);
#3684=CIRCLE('',#11882,0.3125);
#3685=CIRCLE('',#11884,1.25);
#3686=CIRCLE('',#11885,20.);
#3687=CIRCLE('',#11899,55.7165291308792);
#3688=CIRCLE('',#11901,48.5290291308792);
#3689=CIRCLE('',#11902,57.0959708691208);
#3690=CIRCLE('',#11903,1927.031520572);
#3691=CIRCLE('',#11905,0.625000000000001);
#3692=CIRCLE('',#11906,21.5625);
#3693=CIRCLE('',#11907,48.125);
#3694=CIRCLE('',#11908,0.625000000000001);
#3695=CIRCLE('',#11909,21.5625);
#3696=CIRCLE('',#11910,48.125);
#3697=CIRCLE('',#11911,0.625000000000001);
#3698=CIRCLE('',#11912,21.5625);
#3699=CIRCLE('',#11913,48.125);
#3700=CIRCLE('',#11914,21.5625);
#3701=CIRCLE('',#11915,48.125);
#3702=CIRCLE('',#11916,20.);
#3703=CIRCLE('',#11917,1.25);
#3704=CIRCLE('',#11919,1924.96574975015);
#3705=CIRCLE('',#11921,890.503059959066);
#3706=CIRCLE('',#11923,48.5290291308792);
#3707=CIRCLE('',#11924,55.7165291308792);
#3708=CIRCLE('',#11925,893.129292938247);
#3709=CIRCLE('',#11926,57.0959708691208);
#3710=CIRCLE('',#11928,49.7790291308792);
#3711=CIRCLE('',#11929,54.4084708691208);
#3712=CIRCLE('',#11930,54.4084708691208);
#3713=CIRCLE('',#11932,49.6875);
#3714=CIRCLE('',#11933,49.6875);
#3715=CIRCLE('',#11935,49.6875);
#3716=CIRCLE('',#11936,49.6875);
#3717=CIRCLE('',#11938,49.7790291308792);
#3718=CIRCLE('',#11939,50.6584708691208);
#3719=CIRCLE('',#11940,50.6584708691208);
#3720=CIRCLE('',#11942,49.7790291308792);
#3721=CIRCLE('',#11943,50.6584708691208);
#3722=CIRCLE('',#11944,50.6584708691208);
#3723=CIRCLE('',#11946,5.3125);
#3724=CIRCLE('',#11947,54.6294417382416);
#3725=CIRCLE('',#11948,54.6294417382416);
#3726=CIRCLE('',#11950,5.3125);
#3727=CIRCLE('',#11951,50.8794417382416);
#3728=CIRCLE('',#11952,1.25);
#3729=CIRCLE('',#11953,50.8794417382416);
#3730=CIRCLE('',#11957,5.625);
#3731=CIRCLE('',#11958,5.625);
#3732=CIRCLE('',#11962,57.3169417382416);
#3733=CIRCLE('',#11963,57.3169417382416);
#3734=CIRCLE('',#11964,21.5625);
#3735=CIRCLE('',#11965,0.625000000000001);
#3736=CIRCLE('',#11966,5.3125);
#3737=CIRCLE('',#11967,5.3125);
#3738=CIRCLE('',#11968,5.3125);
#3739=CIRCLE('',#11969,5.3125);
#3740=CIRCLE('',#11970,57.3169417382416);
#3741=CIRCLE('',#11971,21.5625);
#3742=CIRCLE('',#11972,0.625000000000001);
#3743=CIRCLE('',#11973,57.3169417382416);
#3744=CIRCLE('',#11974,57.3169417382416);
#3745=CIRCLE('',#11975,21.5625);
#3746=CIRCLE('',#11976,57.3169417382416);
#3747=CIRCLE('',#11977,21.5625);
#3748=CIRCLE('',#11978,0.625000000000001);
#3749=CIRCLE('',#11979,57.3169417382416);
#3750=CIRCLE('',#11980,57.3169417382416);
#3751=CIRCLE('',#11982,5.625);
#3752=CIRCLE('',#11983,5.625);
#3753=CIRCLE('',#11985,48.5290291308792);
#3754=CIRCLE('',#11986,53.3459708691208);
#3755=CIRCLE('',#11996,21.875);
#3756=CIRCLE('',#11997,21.875);
#3757=CIRCLE('',#11999,55.4955582617584);
#3758=CIRCLE('',#12000,48.75);
#3759=CIRCLE('',#12003,55.4955582617584);
#3760=CIRCLE('',#12004,48.75);
#3761=CIRCLE('',#12007,55.);
#3762=CIRCLE('',#12008,55.);
#3763=CIRCLE('',#12012,0.625000000000001);
#3764=CIRCLE('',#12013,55.3125);
#3765=CIRCLE('',#12014,0.625000000000001);
#3766=CIRCLE('',#12015,0.625000000000001);
#3767=CIRCLE('',#12017,0.937500000000001);
#3768=CIRCLE('',#12018,0.937500000000001);
#3769=CIRCLE('',#12020,0.937500000000001);
#3770=CIRCLE('',#12021,0.937500000000001);
#3771=CIRCLE('',#12023,0.937500000000001);
#3772=CIRCLE('',#12024,0.937500000000001);
#3773=CIRCLE('',#12026,55.7165291308792);
#3774=CIRCLE('',#12028,48.5290291308792);
#3775=CIRCLE('',#12029,57.0959708691208);
#3776=CIRCLE('',#12030,1927.03152059917);
#3777=CIRCLE('',#12032,1924.96575403414);
#3778=CIRCLE('',#12034,890.503063305381);
#3779=CIRCLE('',#12036,48.5290291308792);
#3780=CIRCLE('',#12037,55.7165291308792);
#3781=CIRCLE('',#12038,893.129293181156);
#3782=CIRCLE('',#12039,57.0959708691208);
#3783=CIRCLE('',#12041,49.6875);
#3784=CIRCLE('',#12042,49.6875);
#3785=CIRCLE('',#12044,49.7790291308792);
#3786=CIRCLE('',#12045,50.6584708691208);
#3787=CIRCLE('',#12046,50.6584708691208);
#3788=CIRCLE('',#12048,5.3125);
#3789=CIRCLE('',#12049,54.6294417382416);
#3790=CIRCLE('',#12050,54.6294417382416);
#3791=CIRCLE('',#12052,5.3125);
#3792=CIRCLE('',#12053,50.8794417382416);
#3793=CIRCLE('',#12054,1.25);
#3794=CIRCLE('',#12055,50.8794417382416);
#3795=CIRCLE('',#12058,5.625);
#3796=CIRCLE('',#12059,5.625);
#3797=CIRCLE('',#12062,5.625);
#3798=CIRCLE('',#12063,5.625);
#3799=CIRCLE('',#12065,48.5290291308792);
#3800=CIRCLE('',#12066,53.3459708691208);
#3801=CIRCLE('',#12073,21.875);
#3802=CIRCLE('',#12074,21.875);
#3803=CIRCLE('',#12076,55.4955582617584);
#3804=CIRCLE('',#12077,48.75);
#3805=CIRCLE('',#12080,55.4955582617584);
#3806=CIRCLE('',#12081,48.75);
#3807=CIRCLE('',#12084,55.);
#3808=CIRCLE('',#12085,55.);
#3809=CIRCLE('',#12089,0.625000000000001);
#3810=CIRCLE('',#12090,0.625000000000001);
#3811=CIRCLE('',#12091,55.3125);
#3812=CIRCLE('',#12092,0.625000000000001);
#3813=CIRCLE('',#12095,0.937500000000001);
#3814=CIRCLE('',#12096,0.937500000000001);
#3815=CIRCLE('',#12098,0.937500000000001);
#3816=CIRCLE('',#12099,0.937500000000001);
#3817=CIRCLE('',#12101,55.7165291308792);
#3818=CIRCLE('',#12103,48.5290291308792);
#3819=CIRCLE('',#12104,57.0959708691208);
#3820=CIRCLE('',#12105,1927.031520572);
#3821=CIRCLE('',#12107,1924.96571317355);
#3822=CIRCLE('',#12109,890.503061246252);
#3823=CIRCLE('',#12111,48.5290291308792);
#3824=CIRCLE('',#12112,55.7165291308792);
#3825=CIRCLE('',#12113,893.129292782135);
#3826=CIRCLE('',#12114,57.0959708691208);
#3827=CIRCLE('',#12117,50.6584708691208);
#3828=CIRCLE('',#12118,50.6584708691208);
#3829=CIRCLE('',#12121,5.625);
#3830=CIRCLE('',#12122,5.625);
#3831=CIRCLE('',#12125,5.625);
#3832=CIRCLE('',#12126,5.625);
#3833=CIRCLE('',#12128,48.5290291308792);
#3834=CIRCLE('',#12129,53.3459708691208);
#3835=CIRCLE('',#12136,21.875);
#3836=CIRCLE('',#12137,21.875);
#3837=CIRCLE('',#12139,55.4955582617584);
#3838=CIRCLE('',#12140,48.75);
#3839=CIRCLE('',#12143,55.4955582617584);
#3840=CIRCLE('',#12144,48.75);
#3841=CIRCLE('',#12147,55.);
#3842=CIRCLE('',#12148,55.);
#3843=CIRCLE('',#12152,0.625000000000001);
#3844=CIRCLE('',#12153,55.3125);
#3845=CIRCLE('',#12154,0.625000000000001);
#3846=CIRCLE('',#12155,0.625000000000001);
#3847=CIRCLE('',#12156,4.6875);
#3848=CIRCLE('',#12158,0.937500000000001);
#3849=CIRCLE('',#12159,0.937500000000001);
#3850=CIRCLE('',#12162,0.937500000000001);
#3851=CIRCLE('',#12163,0.937500000000001);
#3852=CIRCLE('',#12165,55.7165291308792);
#3853=CIRCLE('',#12167,48.5290291308792);
#3854=CIRCLE('',#12168,57.0959708691208);
#3855=CIRCLE('',#12169,1927.03152058192);
#3856=CIRCLE('',#12171,1924.9657347274);
#3857=CIRCLE('',#12173,890.503062314187);
#3858=CIRCLE('',#12175,48.5290291308792);
#3859=CIRCLE('',#12176,55.7165291308792);
#3860=CIRCLE('',#12177,893.129296310679);
#3861=CIRCLE('',#12178,57.0959708691208);
#3862=CIRCLE('',#12180,5.3125);
#3863=CIRCLE('',#12181,54.6294417382416);
#3864=CIRCLE('',#12182,1.25);
#3865=CIRCLE('',#12183,54.6294417382416);
#3866=CIRCLE('',#12185,5.3125);
#3867=CIRCLE('',#12186,50.8794417382416);
#3868=CIRCLE('',#12187,50.8794417382416);
#3869=CIRCLE('',#12189,5.625);
#3870=CIRCLE('',#12190,5.625);
#3871=CIRCLE('',#12192,5.625);
#3872=CIRCLE('',#12193,5.625);
#3873=CIRCLE('',#12195,48.5290291308792);
#3874=CIRCLE('',#12196,53.3459708691208);
#3875=CIRCLE('',#12200,21.875);
#3876=CIRCLE('',#12201,21.875);
#3877=CIRCLE('',#12203,55.4955582617584);
#3878=CIRCLE('',#12204,48.75);
#3879=CIRCLE('',#12207,55.4955582617584);
#3880=CIRCLE('',#12208,48.75);
#3881=CIRCLE('',#12211,55.);
#3882=CIRCLE('',#12212,55.);
#3883=CIRCLE('',#12216,4.6875);
#3884=CIRCLE('',#12217,0.625000000000001);
#3885=CIRCLE('',#12218,0.625000000000001);
#3886=CIRCLE('',#12219,55.3125);
#3887=CIRCLE('',#12220,0.625000000000001);
#3888=CIRCLE('',#12222,0.937500000000001);
#3889=CIRCLE('',#12223,0.937500000000001);
#3890=CIRCLE('',#12225,0.937500000000001);
#3891=CIRCLE('',#12226,0.937500000000001);
#3892=CIRCLE('',#12229,0.3125);
#3893=CIRCLE('',#12231,0.3125);
#3894=CIRCLE('',#12233,0.3125);
#3895=CIRCLE('',#12235,0.3125);
#3896=CIRCLE('',#12237,0.312499999999999);
#3897=CIRCLE('',#12239,0.312499999999997);
#3898=CIRCLE('',#12242,0.3125);
#3899=CIRCLE('',#12244,0.3125);
#3900=CIRCLE('',#12246,0.3125);
#3901=CIRCLE('',#12248,0.3125);
#3902=CIRCLE('',#12250,0.312499999999999);
#3903=CIRCLE('',#12252,0.312499999999997);
#3904=CIRCLE('',#12254,0.313663740331856);
#3905=CIRCLE('',#12255,0.313663740332209);
#3906=CIRCLE('',#12256,0.3125);
#3907=CIRCLE('',#12257,0.312500000000002);
#3908=CIRCLE('',#12258,0.312500000000002);
#3909=CIRCLE('',#12259,0.3125);
#3910=CIRCLE('',#12261,0.312499999999997);
#3911=CIRCLE('',#12263,0.312499999999999);
#3912=CIRCLE('',#12265,0.3125);
#3913=CIRCLE('',#12268,0.3125);
#3914=CIRCLE('',#12269,0.3125);
#3915=CIRCLE('',#12270,0.312500000000003);
#3916=CIRCLE('',#12272,0.312500000000002);
#3917=CIRCLE('',#12273,0.312500000000001);
#3918=CIRCLE('',#12274,0.312499999999996);
#3919=CIRCLE('',#12275,0.312499999999999);
#3920=CIRCLE('',#12277,0.312500000000002);
#3921=CIRCLE('',#12278,0.312500000000003);
#3922=CIRCLE('',#12280,0.312499999999998);
#3923=CIRCLE('',#12282,0.312499999999999);
#3924=CIRCLE('',#12285,0.3125);
#3925=CIRCLE('',#12286,0.3125);
#3926=CIRCLE('',#12288,0.3125);
#3927=CIRCLE('',#12290,0.312499999999999);
#3928=CIRCLE('',#12291,0.312499999999999);
#3929=CIRCLE('',#12293,0.312499999999999);
#3930=CIRCLE('',#12294,0.312499999999999);
#3931=CIRCLE('',#12296,0.312500000000001);
#3932=CIRCLE('',#12298,0.312499999999998);
#3933=CIRCLE('',#12299,0.312500000000002);
#3934=CIRCLE('',#12300,0.312500000000002);
#3935=CIRCLE('',#12301,0.3125);
#3936=CIRCLE('',#12303,0.312499999999997);
#3937=CIRCLE('',#12305,0.312500000000002);
#3938=CIRCLE('',#12306,0.312500000000002);
#3939=CIRCLE('',#12307,0.3125);
#3940=CIRCLE('',#12308,0.3125);
#3941=CIRCLE('',#12310,0.3125);
#3942=CIRCLE('',#12312,0.3125);
#3943=CIRCLE('',#12313,0.312499999999996);
#3944=CIRCLE('',#12317,0.3125);
#3945=CIRCLE('',#12320,0.312500000000002);
#3946=CIRCLE('',#12322,0.3125);
#3947=CIRCLE('',#12323,0.312500000000003);
#3948=CIRCLE('',#12324,0.313663740332281);
#3949=CIRCLE('',#12326,0.3125);
#3950=CIRCLE('',#12328,0.312500000000002);
#3951=CIRCLE('',#12330,0.312499999999999);
#3952=CIRCLE('',#12331,0.312500000000002);
#3953=CIRCLE('',#12332,0.312500000000001);
#3954=CIRCLE('',#12333,0.312500000000002);
#3955=CIRCLE('',#12335,0.312499999999998);
#3956=CIRCLE('',#12336,0.3125);
#3957=CIRCLE('',#12337,0.3125);
#3958=CIRCLE('',#12339,0.312500000000002);
#3959=CIRCLE('',#12341,0.312499999999997);
#3960=CIRCLE('',#12343,0.312500000000002);
#3961=CIRCLE('',#12345,0.3125);
#3962=CIRCLE('',#12347,0.312499999999999);
#3963=CIRCLE('',#12349,0.312499999999997);
#3964=CIRCLE('',#12351,0.312499999999999);
#3965=CIRCLE('',#12352,0.312500000000002);
#3966=CIRCLE('',#12353,0.312500000000002);
#3967=CIRCLE('',#12354,0.312500000000002);
#3968=CIRCLE('',#12355,0.312500000000002);
#3969=CIRCLE('',#12356,0.3125);
#3970=CIRCLE('',#12358,0.312499999999999);
#3971=CIRCLE('',#12360,0.312499999999999);
#3972=CIRCLE('',#12362,0.3125);
#3973=CIRCLE('',#12365,0.312500000000002);
#3974=CIRCLE('',#12367,0.3125);
#3975=CIRCLE('',#12369,0.312500000000001);
#3976=CIRCLE('',#12371,0.312499999999999);
#3977=CIRCLE('',#12372,0.312500000000003);
#3978=CIRCLE('',#12374,0.312500000000001);
#3979=CIRCLE('',#12376,0.312499999999999);
#3980=CIRCLE('',#12379,0.3125);
#3981=CIRCLE('',#12380,0.3125);
#3982=CIRCLE('',#12381,0.312500000000003);
#3983=CIRCLE('',#12383,0.312500000000002);
#3984=CIRCLE('',#12384,0.312500000000001);
#3985=CIRCLE('',#12386,0.3125);
#3986=CIRCLE('',#12387,0.3125);
#3987=CIRCLE('',#12389,0.312499999999999);
#3988=CIRCLE('',#12391,0.312499999999999);
#3989=CIRCLE('',#12393,0.3125);
#3990=CIRCLE('',#12395,0.312500000000002);
#3991=CIRCLE('',#12397,0.3125);
#3992=CIRCLE('',#12398,0.312500000000003);
#3993=CIRCLE('',#12400,0.312499999999998);
#3994=CIRCLE('',#12402,0.312499999999999);
#3995=CIRCLE('',#12405,0.3125);
#3996=CIRCLE('',#12408,0.312500000000001);
#3997=CIRCLE('',#12410,0.3125);
#3998=CIRCLE('',#12412,0.312499999999999);
#3999=CIRCLE('',#12415,0.312499999999999);
#4000=CIRCLE('',#12416,0.312500000000002);
#4001=CIRCLE('',#12418,0.3125);
#4002=CIRCLE('',#12420,0.312499999999999);
#4003=CIRCLE('',#12421,0.312500000000002);
#4004=CIRCLE('',#12422,0.312500000000002);
#4005=CIRCLE('',#12423,0.312499999999997);
#4006=CIRCLE('',#12425,0.3125);
#4007=CIRCLE('',#12426,0.312500000000001);
#4008=CIRCLE('',#12428,0.312500000000001);
#4009=CIRCLE('',#12430,0.312499999999999);
#4010=CIRCLE('',#12432,0.312500000000002);
#4011=CIRCLE('',#12434,0.312499999999999);
#4012=CIRCLE('',#12436,0.3125);
#4013=CIRCLE('',#12438,0.312500000000002);
#4014=CIRCLE('',#12440,0.312499999999999);
#4015=CIRCLE('',#12441,0.312500000000002);
#4016=CIRCLE('',#12443,0.3125);
#4017=CIRCLE('',#12444,0.312500000000002);
#4018=CIRCLE('',#12446,0.312500000000002);
#4019=CIRCLE('',#12448,0.312500000000002);
#4020=CIRCLE('',#12450,0.3125);
#4021=CIRCLE('',#12452,0.3125);
#4022=CIRCLE('',#12454,0.312499999999997);
#4023=CIRCLE('',#12456,0.3125);
#4024=CIRCLE('',#12457,0.3125);
#4025=CIRCLE('',#12459,0.312500000000002);
#4026=CIRCLE('',#12460,0.312500000000002);
#4027=CIRCLE('',#12463,0.312499999999997);
#4028=CIRCLE('',#12465,0.312500000000001);
#4029=CIRCLE('',#12467,0.312499999999999);
#4030=CIRCLE('',#12468,0.312499999999999);
#4031=CIRCLE('',#12470,0.312499999999996);
#4032=CIRCLE('',#12472,0.312500000000002);
#4033=CIRCLE('',#12474,0.312499999999997);
#4034=CIRCLE('',#12475,0.3125);
#4035=CIRCLE('',#12477,0.3125);
#4036=CIRCLE('',#12479,0.312499999999999);
#4037=CIRCLE('',#12480,0.312499999999999);
#4038=CIRCLE('',#12482,0.3125);
#4039=CIRCLE('',#12484,0.3125);
#4040=CIRCLE('',#12487,0.312500000000002);
#4041=CIRCLE('',#12488,0.312500000000001);
#4042=CIRCLE('',#12490,0.312500000000003);
#4043=CIRCLE('',#12492,0.3125);
#4044=CIRCLE('',#12493,0.312499999999997);
#4045=CIRCLE('',#12495,0.312499999999999);
#4046=CIRCLE('',#12496,0.3125);
#4047=CIRCLE('',#12497,0.312499999999999);
#4048=CIRCLE('',#12499,0.312500000000001);
#4049=CIRCLE('',#12502,0.3125);
#4050=CIRCLE('',#12504,0.3125);
#4051=CIRCLE('',#12506,0.3125);
#4052=CIRCLE('',#12508,0.3125);
#4053=CIRCLE('',#12509,0.312500000000003);
#4054=CIRCLE('',#12510,0.313663740331845);
#4055=CIRCLE('',#12512,0.3125);
#4056=CIRCLE('',#12514,0.312500000000002);
#4057=CIRCLE('',#12516,0.312499999999998);
#4058=CIRCLE('',#12518,0.312499999999998);
#4059=CIRCLE('',#12520,0.3125);
#4060=CIRCLE('',#12521,0.3125);
#4061=CIRCLE('',#12523,0.312500000000002);
#4062=CIRCLE('',#12524,0.312500000000001);
#4063=CIRCLE('',#12526,0.312499999999999);
#4064=CIRCLE('',#12528,0.312500000000002);
#4065=CIRCLE('',#12529,0.312499999999999);
#4066=CIRCLE('',#12530,0.312500000000001);
#4067=CIRCLE('',#12533,0.312499999999997);
#4068=CIRCLE('',#12534,0.312500000000002);
#4069=CIRCLE('',#12537,0.312500000000003);
#4070=CIRCLE('',#12538,0.312499999999999);
#4071=CIRCLE('',#12540,0.312500000000003);
#4072=CIRCLE('',#12542,0.312499999999996);
#4073=CIRCLE('',#12543,0.312499999999999);
#4074=CIRCLE('',#12545,0.312499999999998);
#4075=CIRCLE('',#12548,0.312500000000001);
#4076=CIRCLE('',#12550,0.312500000000003);
#4077=CIRCLE('',#12551,0.3125);
#4078=CIRCLE('',#12553,0.312500000000003);
#4079=CIRCLE('',#12554,0.3125);
#4080=CIRCLE('',#12555,0.3125);
#4081=CIRCLE('',#12557,0.312500000000001);
#4082=CIRCLE('',#12558,0.312499999999999);
#4083=CIRCLE('',#12560,0.312500000000003);
#4084=CIRCLE('',#12562,0.312500000000002);
#4085=CIRCLE('',#12564,0.312500000000004);
#4086=CIRCLE('',#12565,0.3125);
#4087=CIRCLE('',#12567,0.3125);
#4088=CIRCLE('',#12569,0.312500000000001);
#4089=CIRCLE('',#12571,0.3125);
#4090=CIRCLE('',#12572,0.312500000000001);
#4091=CIRCLE('',#12574,0.312500000000003);
#4092=CIRCLE('',#12576,0.312500000000001);
#4093=CIRCLE('',#12577,0.3125);
#4094=CIRCLE('',#12579,0.3125);
#4095=CIRCLE('',#12581,0.312499999999997);
#4096=CIRCLE('',#12582,0.312499999999999);
#4097=CIRCLE('',#12585,0.312499999999998);
#4098=CIRCLE('',#12587,0.312500000000001);
#4099=CIRCLE('',#12589,0.3125);
#4100=CIRCLE('',#12591,0.3125);
#4101=CIRCLE('',#12594,0.312499999999998);
#4102=CIRCLE('',#12595,0.3125);
#4103=CIRCLE('',#12596,0.3125);
#4104=CIRCLE('',#12598,0.312500000000001);
#4105=CIRCLE('',#12599,0.3125);
#4106=CIRCLE('',#12601,0.312499999999996);
#4107=CIRCLE('',#12603,0.3125);
#4108=CIRCLE('',#12604,0.3125);
#4109=CIRCLE('',#12606,0.3125);
#4110=CIRCLE('',#12607,0.312500000000003);
#4111=CIRCLE('',#12609,0.312500000000001);
#4112=CIRCLE('',#12611,0.3125);
#4113=CIRCLE('',#12612,0.3125);
#4114=CIRCLE('',#12616,0.312500000000001);
#4115=CIRCLE('',#12618,0.312499999999999);
#4116=CIRCLE('',#12620,0.3125);
#4117=CIRCLE('',#12621,0.3125);
#4118=CIRCLE('',#12623,0.312500000000003);
#4119=CIRCLE('',#12625,0.3125);
#4120=CIRCLE('',#12626,0.312500000000002);
#4121=CIRCLE('',#12627,0.312500000000001);
#4122=CIRCLE('',#12629,0.3125);
#4123=CIRCLE('',#12631,0.3125);
#4124=CIRCLE('',#12632,0.3125);
#4125=CIRCLE('',#12634,0.312500000000002);
#4126=CIRCLE('',#12635,0.3125);
#4127=CIRCLE('',#12636,0.3125);
#4128=CIRCLE('',#12638,0.3125);
#4129=CIRCLE('',#12639,0.312500000000003);
#4130=CIRCLE('',#12641,0.312499999999998);
#4131=CIRCLE('',#12644,0.3125);
#4132=CIRCLE('',#12646,0.3125);
#4133=CIRCLE('',#12648,0.312500000000001);
#4134=CIRCLE('',#12650,0.312500000000003);
#4135=CIRCLE('',#12651,0.3125);
#4136=CIRCLE('',#12653,0.3125);
#4137=CIRCLE('',#12655,0.312499999999999);
#4138=CIRCLE('',#12657,0.312500000000002);
#4139=CIRCLE('',#12659,0.3125);
#4140=CIRCLE('',#12661,0.312499999999998);
#4141=CIRCLE('',#12662,0.3125);
#4142=CIRCLE('',#12664,0.3125);
#4143=CIRCLE('',#12666,0.312500000000001);
#4144=CIRCLE('',#12667,0.3125);
#4145=CIRCLE('',#12669,0.312500000000003);
#4146=CIRCLE('',#12670,0.3125);
#4147=CIRCLE('',#12671,0.3125);
#4148=CIRCLE('',#12673,0.3125);
#4149=CIRCLE('',#12675,0.312500000000001);
#4150=CIRCLE('',#12677,0.3125);
#4151=CIRCLE('',#12678,0.3125);
#4152=CIRCLE('',#12680,0.3125);
#4153=CIRCLE('',#12682,0.312499999999999);
#4154=CIRCLE('',#12684,0.3125);
#4155=CIRCLE('',#12686,0.312499999999998);
#4156=CIRCLE('',#12688,0.312499999999998);
#4157=CIRCLE('',#12689,0.312499999999999);
#4158=CIRCLE('',#12691,0.312499999999999);
#4159=CIRCLE('',#12693,0.3125);
#4160=CIRCLE('',#12695,0.3125);
#4161=CIRCLE('',#12697,0.312499999999998);
#4162=CIRCLE('',#12699,0.3125);
#4163=CIRCLE('',#12700,0.3125);
#4164=CIRCLE('',#12701,0.3125);
#4165=CIRCLE('',#12703,0.312499999999998);
#4166=CIRCLE('',#12705,0.3125);
#4167=CIRCLE('',#12707,0.312500000000001);
#4168=CIRCLE('',#12709,0.3125);
#4169=CIRCLE('',#12710,0.3125);
#4170=CIRCLE('',#12712,0.312500000000001);
#4171=CIRCLE('',#12714,0.3125);
#4172=CIRCLE('',#12715,0.3125);
#4173=CIRCLE('',#12717,0.312499999999998);
#4174=CIRCLE('',#12719,0.3125);
#4175=CIRCLE('',#12722,0.3125);
#4176=CIRCLE('',#12723,0.3125);
#4177=CIRCLE('',#12725,0.312500000000004);
#4178=CIRCLE('',#12727,0.312500000000001);
#4179=CIRCLE('',#12729,0.312500000000001);
#4180=CIRCLE('',#12731,0.3125);
#4181=CIRCLE('',#12732,0.3125);
#4182=CIRCLE('',#12734,0.312499999999997);
#4183=CIRCLE('',#12736,0.312500000000002);
#4184=CIRCLE('',#12738,0.312499999999997);
#4185=CIRCLE('',#12740,0.3125);
#4186=CIRCLE('',#12742,0.3125);
#4187=CIRCLE('',#12744,0.312500000000001);
#4188=CIRCLE('',#12745,0.312499999999999);
#4189=CIRCLE('',#12747,0.312500000000001);
#4190=CIRCLE('',#12749,0.312499999999999);
#4191=CIRCLE('',#12751,0.312499999999999);
#4192=CIRCLE('',#12753,0.312500000000001);
#4193=CIRCLE('',#12755,0.3125);
#4194=CIRCLE('',#12756,0.3125);
#4195=CIRCLE('',#12758,0.3125);
#4196=CIRCLE('',#12760,0.312500000000001);
#4197=CIRCLE('',#12762,0.312499999999999);
#4198=CIRCLE('',#12764,0.3125);
#4199=CIRCLE('',#12766,0.312499999999998);
#4200=CIRCLE('',#12767,0.3125);
#4201=CIRCLE('',#12769,0.3125);
#4202=CIRCLE('',#12771,0.312500000000001);
#4203=CIRCLE('',#12773,0.312499999999997);
#4204=CIRCLE('',#12775,0.3125);
#4205=CIRCLE('',#12776,0.312500000000003);
#4206=CIRCLE('',#12778,0.312500000000001);
#4207=CIRCLE('',#12780,0.3125);
#4208=CIRCLE('',#12783,0.3125);
#4209=CIRCLE('',#12785,0.312500000000001);
#4210=CIRCLE('',#12787,0.3125);
#4211=CIRCLE('',#12789,0.312499999999999);
#4212=CIRCLE('',#12791,0.312499999999997);
#4213=CIRCLE('',#12792,0.31366374033177);
#4214=CIRCLE('',#12793,0.313663740332204);
#4215=CIRCLE('',#12794,0.313663740331843);
#4216=CIRCLE('',#12796,0.3125);
#4217=CIRCLE('',#12797,0.3125);
#4218=CIRCLE('',#12798,0.312500000000001);
#4219=CIRCLE('',#12799,0.312500000000001);
#4220=CIRCLE('',#12801,0.312500000000001);
#4221=CIRCLE('',#12803,0.3125);
#4222=CIRCLE('',#12804,0.3125);
#4223=CIRCLE('',#12806,0.312500000000001);
#4224=CIRCLE('',#12807,0.312500000000001);
#4225=CIRCLE('',#12808,0.3125);
#4226=CIRCLE('',#12812,0.312500000000001);
#4227=CIRCLE('',#12814,0.3125);
#4228=CIRCLE('',#12815,0.313663740332451);
#4229=CIRCLE('',#12816,0.3125);
#4230=CIRCLE('',#12817,0.312500000000001);
#4231=CIRCLE('',#12821,0.3125);
#4232=CIRCLE('',#12823,0.312500000000001);
#4233=CIRCLE('',#12824,0.313672771251787);
#4234=CIRCLE('',#12826,0.3125);
#4235=CIRCLE('',#12827,0.3125);
#4236=CIRCLE('',#12829,0.3125);
#4237=CIRCLE('',#12831,0.3125);
#4238=CIRCLE('',#12833,0.3125);
#4239=CIRCLE('',#12835,0.3125);
#4240=CIRCLE('',#12837,0.3125);
#4241=CIRCLE('',#12839,0.3125);
#4242=CIRCLE('',#12842,0.3125);
#4243=CIRCLE('',#12843,0.3125);
#4244=CIRCLE('',#12845,0.3125);
#4245=CIRCLE('',#12847,0.3125);
#4246=CIRCLE('',#12849,0.3125);
#4247=CIRCLE('',#12851,0.3125);
#4248=CIRCLE('',#12853,0.3125);
#4249=CIRCLE('',#12855,0.3125);
#4250=CIRCLE('',#12858,0.312499999999997);
#4251=CIRCLE('',#12860,0.3125);
#4252=CIRCLE('',#12862,0.3125);
#4253=CIRCLE('',#12863,0.3125);
#4254=CIRCLE('',#12865,0.3125);
#4255=CIRCLE('',#12867,0.312499999999997);
#4256=CIRCLE('',#12869,0.312499999999997);
#4257=CIRCLE('',#12872,0.312500000000001);
#4258=CIRCLE('',#12874,0.3125);
#4259=CIRCLE('',#12876,0.3125);
#4260=CIRCLE('',#12877,0.3125);
#4261=CIRCLE('',#12879,0.3125);
#4262=CIRCLE('',#12881,0.312499999999997);
#4263=CIRCLE('',#12883,0.312499999999997);
#4264=CIRCLE('',#12886,0.3125);
#4265=CIRCLE('',#12888,0.3125);
#4266=CIRCLE('',#12890,0.3125);
#4267=CIRCLE('',#12893,0.312499999999997);
#4268=CIRCLE('',#12896,0.3125);
#4269=CIRCLE('',#12898,0.3125);
#4270=CIRCLE('',#12900,0.3125);
#4271=CIRCLE('',#12903,0.312499999999997);
#4272=CIRCLE('',#12906,0.3125);
#4273=CIRCLE('',#12908,0.3125);
#4274=CIRCLE('',#12911,0.3125);
#4275=CIRCLE('',#12913,0.312499999999997);
#4276=CIRCLE('',#12916,0.3125);
#4277=CIRCLE('',#12918,0.3125);
#4278=CIRCLE('',#12921,0.3125);
#4279=CIRCLE('',#12923,0.312499999999997);
#4280=CIRCLE('',#12952,21.875);
#4281=CIRCLE('',#12953,21.875);
#4282=CIRCLE('',#12954,21.875);
#4283=CIRCLE('',#12955,21.875);
#4284=CIRCLE('',#12956,21.875);
#4285=CIRCLE('',#12957,21.875);
#4286=CIRCLE('',#12958,21.875);
#4287=CIRCLE('',#12959,21.875);
#4288=CIRCLE('',#12960,21.875);
#4289=CIRCLE('',#12962,3.75);
#4290=CIRCLE('',#12963,2.5);
#4291=CIRCLE('',#12964,6.25);
#4292=CIRCLE('',#12966,1.875);
#4293=CIRCLE('',#12967,1.875);
#4294=CIRCLE('',#12969,18.75);
#4295=CIRCLE('',#12970,1.25);
#4296=CIRCLE('',#12971,20.);
#4297=CIRCLE('',#12973,20.);
#4298=CIRCLE('',#12976,19.375);
#4299=CIRCLE('',#12977,2.5);
#4300=CIRCLE('',#12978,21.875);
#4301=VERTEX_POINT('',#16376);
#4302=VERTEX_POINT('',#16378);
#4303=VERTEX_POINT('',#16382);
#4304=VERTEX_POINT('',#16384);
#4305=VERTEX_POINT('',#16388);
#4306=VERTEX_POINT('',#16390);
#4307=VERTEX_POINT('',#16394);
#4308=VERTEX_POINT('',#16396);
#4309=VERTEX_POINT('',#16400);
#4310=VERTEX_POINT('',#16401);
#4311=VERTEX_POINT('',#16404);
#4312=VERTEX_POINT('',#16408);
#4313=VERTEX_POINT('',#16410);
#4314=VERTEX_POINT('',#16412);
#4315=VERTEX_POINT('',#16416);
#4316=VERTEX_POINT('',#16418);
#4317=VERTEX_POINT('',#16422);
#4318=VERTEX_POINT('',#16424);
#4319=VERTEX_POINT('',#16426);
#4320=VERTEX_POINT('',#16430);
#4321=VERTEX_POINT('',#16431);
#4322=VERTEX_POINT('',#16433);
#4323=VERTEX_POINT('',#16435);
#4324=VERTEX_POINT('',#16439);
#4325=VERTEX_POINT('',#16440);
#4326=VERTEX_POINT('',#16442);
#4327=VERTEX_POINT('',#16444);
#4328=VERTEX_POINT('',#16448);
#4329=VERTEX_POINT('',#16449);
#4330=VERTEX_POINT('',#16451);
#4331=VERTEX_POINT('',#16453);
#4332=VERTEX_POINT('',#16457);
#4333=VERTEX_POINT('',#16458);
#4334=VERTEX_POINT('',#16460);
#4335=VERTEX_POINT('',#16462);
#4336=VERTEX_POINT('',#16466);
#4337=VERTEX_POINT('',#16467);
#4338=VERTEX_POINT('',#16470);
#4339=VERTEX_POINT('',#16474);
#4340=VERTEX_POINT('',#16476);
#4341=VERTEX_POINT('',#16478);
#4342=VERTEX_POINT('',#16482);
#4343=VERTEX_POINT('',#16484);
#4344=VERTEX_POINT('',#16486);
#4345=VERTEX_POINT('',#16490);
#4346=VERTEX_POINT('',#16492);
#4347=VERTEX_POINT('',#16494);
#4348=VERTEX_POINT('',#16498);
#4349=VERTEX_POINT('',#16499);
#4350=VERTEX_POINT('',#16501);
#4351=VERTEX_POINT('',#16503);
#4352=VERTEX_POINT('',#16507);
#4353=VERTEX_POINT('',#16508);
#4354=VERTEX_POINT('',#16510);
#4355=VERTEX_POINT('',#16512);
#4356=VERTEX_POINT('',#16516);
#4357=VERTEX_POINT('',#16517);
#4358=VERTEX_POINT('',#16519);
#4359=VERTEX_POINT('',#16521);
#4360=VERTEX_POINT('',#16525);
#4361=VERTEX_POINT('',#16526);
#4362=VERTEX_POINT('',#16528);
#4363=VERTEX_POINT('',#16530);
#4364=VERTEX_POINT('',#16534);
#4365=VERTEX_POINT('',#16536);
#4366=VERTEX_POINT('',#16540);
#4367=VERTEX_POINT('',#16542);
#4368=VERTEX_POINT('',#16546);
#4369=VERTEX_POINT('',#16548);
#4370=VERTEX_POINT('',#16550);
#4371=VERTEX_POINT('',#16554);
#4372=VERTEX_POINT('',#16556);
#4373=VERTEX_POINT('',#16560);
#4374=VERTEX_POINT('',#16561);
#4375=VERTEX_POINT('',#16563);
#4376=VERTEX_POINT('',#16565);
#4377=VERTEX_POINT('',#16569);
#4378=VERTEX_POINT('',#16570);
#4379=VERTEX_POINT('',#16572);
#4380=VERTEX_POINT('',#16574);
#4381=VERTEX_POINT('',#16578);
#4382=VERTEX_POINT('',#16579);
#4383=VERTEX_POINT('',#16581);
#4384=VERTEX_POINT('',#16586);
#4385=VERTEX_POINT('',#16588);
#4386=VERTEX_POINT('',#16590);
#4387=VERTEX_POINT('',#16594);
#4388=VERTEX_POINT('',#16596);
#4389=VERTEX_POINT('',#16598);
#4390=VERTEX_POINT('',#16602);
#4391=VERTEX_POINT('',#16604);
#4392=VERTEX_POINT('',#16606);
#4393=VERTEX_POINT('',#16610);
#4394=VERTEX_POINT('',#16611);
#4395=VERTEX_POINT('',#16613);
#4396=VERTEX_POINT('',#16615);
#4397=VERTEX_POINT('',#16619);
#4398=VERTEX_POINT('',#16620);
#4399=VERTEX_POINT('',#16622);
#4400=VERTEX_POINT('',#16624);
#4401=VERTEX_POINT('',#16628);
#4402=VERTEX_POINT('',#16629);
#4403=VERTEX_POINT('',#16631);
#4404=VERTEX_POINT('',#16633);
#4405=VERTEX_POINT('',#16637);
#4406=VERTEX_POINT('',#16638);
#4407=VERTEX_POINT('',#16640);
#4408=VERTEX_POINT('',#16642);
#4409=VERTEX_POINT('',#16646);
#4410=VERTEX_POINT('',#16647);
#4411=VERTEX_POINT('',#16649);
#4412=VERTEX_POINT('',#16651);
#4413=VERTEX_POINT('',#16655);
#4414=VERTEX_POINT('',#16656);
#4415=VERTEX_POINT('',#16658);
#4416=VERTEX_POINT('',#16660);
#4417=VERTEX_POINT('',#16664);
#4418=VERTEX_POINT('',#16665);
#4419=VERTEX_POINT('',#16667);
#4420=VERTEX_POINT('',#16669);
#4421=VERTEX_POINT('',#16673);
#4422=VERTEX_POINT('',#16674);
#4423=VERTEX_POINT('',#16676);
#4424=VERTEX_POINT('',#16678);
#4425=VERTEX_POINT('',#16682);
#4426=VERTEX_POINT('',#16683);
#4427=VERTEX_POINT('',#16685);
#4428=VERTEX_POINT('',#16687);
#4429=VERTEX_POINT('',#16691);
#4430=VERTEX_POINT('',#16693);
#4431=VERTEX_POINT('',#16697);
#4432=VERTEX_POINT('',#16698);
#4433=VERTEX_POINT('',#16700);
#4434=VERTEX_POINT('',#16702);
#4435=VERTEX_POINT('',#16706);
#4436=VERTEX_POINT('',#16707);
#4437=VERTEX_POINT('',#16709);
#4438=VERTEX_POINT('',#16711);
#4439=VERTEX_POINT('',#16715);
#4440=VERTEX_POINT('',#16716);
#4441=VERTEX_POINT('',#16718);
#4442=VERTEX_POINT('',#16720);
#4443=VERTEX_POINT('',#16724);
#4444=VERTEX_POINT('',#16725);
#4445=VERTEX_POINT('',#16727);
#4446=VERTEX_POINT('',#16729);
#4447=VERTEX_POINT('',#16733);
#4448=VERTEX_POINT('',#16734);
#4449=VERTEX_POINT('',#16736);
#4450=VERTEX_POINT('',#16738);
#4451=VERTEX_POINT('',#16742);
#4452=VERTEX_POINT('',#16743);
#4453=VERTEX_POINT('',#16745);
#4454=VERTEX_POINT('',#16747);
#4455=VERTEX_POINT('',#16751);
#4456=VERTEX_POINT('',#16752);
#4457=VERTEX_POINT('',#16754);
#4458=VERTEX_POINT('',#16756);
#4459=VERTEX_POINT('',#16760);
#4460=VERTEX_POINT('',#16761);
#4461=VERTEX_POINT('',#16763);
#4462=VERTEX_POINT('',#16765);
#4463=VERTEX_POINT('',#16769);
#4464=VERTEX_POINT('',#16772);
#4465=VERTEX_POINT('',#16780);
#4466=VERTEX_POINT('',#16782);
#4467=VERTEX_POINT('',#16786);
#4468=VERTEX_POINT('',#16787);
#4469=VERTEX_POINT('',#16789);
#4470=VERTEX_POINT('',#16791);
#4471=VERTEX_POINT('',#16795);
#4472=VERTEX_POINT('',#16797);
#4473=VERTEX_POINT('',#16806);
#4474=VERTEX_POINT('',#16815);
#4475=VERTEX_POINT('',#16817);
#4476=VERTEX_POINT('',#16828);
#4477=VERTEX_POINT('',#16839);
#4478=VERTEX_POINT('',#16850);
#4479=VERTEX_POINT('',#16852);
#4480=VERTEX_POINT('',#16856);
#4481=VERTEX_POINT('',#16857);
#4482=VERTEX_POINT('',#16859);
#4483=VERTEX_POINT('',#16861);
#4484=VERTEX_POINT('',#16872);
#4485=VERTEX_POINT('',#16873);
#4486=VERTEX_POINT('',#16875);
#4487=VERTEX_POINT('',#16884);
#4488=VERTEX_POINT('',#16886);
#4489=VERTEX_POINT('',#16897);
#4490=VERTEX_POINT('',#16908);
#4491=VERTEX_POINT('',#16919);
#4492=VERTEX_POINT('',#16920);
#4493=VERTEX_POINT('',#16931);
#4494=VERTEX_POINT('',#16932);
#4495=VERTEX_POINT('',#16934);
#4496=VERTEX_POINT('',#16936);
#4497=VERTEX_POINT('',#16938);
#4498=VERTEX_POINT('',#16940);
#4499=VERTEX_POINT('',#16942);
#4500=VERTEX_POINT('',#16944);
#4501=VERTEX_POINT('',#16946);
#4502=VERTEX_POINT('',#16948);
#4503=VERTEX_POINT('',#16950);
#4504=VERTEX_POINT('',#16997);
#4505=VERTEX_POINT('',#16999);
#4506=VERTEX_POINT('',#17001);
#4507=VERTEX_POINT('',#17003);
#4508=VERTEX_POINT('',#17035);
#4509=VERTEX_POINT('',#17037);
#4510=VERTEX_POINT('',#17072);
#4511=VERTEX_POINT('',#17075);
#4512=VERTEX_POINT('',#17119);
#4513=VERTEX_POINT('',#17121);
#4514=VERTEX_POINT('',#17123);
#4515=VERTEX_POINT('',#17125);
#4516=VERTEX_POINT('',#17127);
#4517=VERTEX_POINT('',#17174);
#4518=VERTEX_POINT('',#17177);
#4519=VERTEX_POINT('',#17209);
#4520=VERTEX_POINT('',#17211);
#4521=VERTEX_POINT('',#17246);
#4522=VERTEX_POINT('',#17248);
#4523=VERTEX_POINT('',#17250);
#4524=VERTEX_POINT('',#17252);
#4525=VERTEX_POINT('',#17296);
#4526=VERTEX_POINT('',#17298);
#4527=VERTEX_POINT('',#17300);
#4528=VERTEX_POINT('',#17302);
#4529=VERTEX_POINT('',#17304);
#4530=VERTEX_POINT('',#17351);
#4531=VERTEX_POINT('',#17353);
#4532=VERTEX_POINT('',#17355);
#4533=VERTEX_POINT('',#17357);
#4534=VERTEX_POINT('',#17389);
#4535=VERTEX_POINT('',#17425);
#4536=VERTEX_POINT('',#17427);
#4537=VERTEX_POINT('',#17429);
#4538=VERTEX_POINT('',#17473);
#4539=VERTEX_POINT('',#17475);
#4540=VERTEX_POINT('',#17477);
#4541=VERTEX_POINT('',#17479);
#4542=VERTEX_POINT('',#17527);
#4543=VERTEX_POINT('',#17529);
#4544=VERTEX_POINT('',#17531);
#4545=VERTEX_POINT('',#17563);
#4546=VERTEX_POINT('',#17565);
#4547=VERTEX_POINT('',#17600);
#4548=VERTEX_POINT('',#17602);
#4549=VERTEX_POINT('',#17604);
#4550=VERTEX_POINT('',#17606);
#4551=VERTEX_POINT('',#17650);
#4552=VERTEX_POINT('',#17653);
#4553=VERTEX_POINT('',#17655);
#4554=VERTEX_POINT('',#17657);
#4555=VERTEX_POINT('',#17659);
#4556=VERTEX_POINT('',#17661);
#4557=VERTEX_POINT('',#17669);
#4558=VERTEX_POINT('',#17670);
#4559=VERTEX_POINT('',#17672);
#4560=VERTEX_POINT('',#17681);
#4561=VERTEX_POINT('',#17683);
#4562=VERTEX_POINT('',#17694);
#4563=VERTEX_POINT('',#17705);
#4564=VERTEX_POINT('',#17716);
#4565=VERTEX_POINT('',#17717);
#4566=VERTEX_POINT('',#17722);
#4567=VERTEX_POINT('',#17723);
#4568=VERTEX_POINT('',#17725);
#4569=VERTEX_POINT('',#17727);
#4570=VERTEX_POINT('',#17731);
#4571=VERTEX_POINT('',#17732);
#4572=VERTEX_POINT('',#17734);
#4573=VERTEX_POINT('',#17736);
#4574=VERTEX_POINT('',#17739);
#4575=VERTEX_POINT('',#17741);
#4576=VERTEX_POINT('',#17743);
#4577=VERTEX_POINT('',#17745);
#4578=VERTEX_POINT('',#17747);
#4579=VERTEX_POINT('',#17749);
#4580=VERTEX_POINT('',#17751);
#4581=VERTEX_POINT('',#17753);
#4582=VERTEX_POINT('',#17755);
#4583=VERTEX_POINT('',#17757);
#4584=VERTEX_POINT('',#17759);
#4585=VERTEX_POINT('',#17761);
#4586=VERTEX_POINT('',#17763);
#4587=VERTEX_POINT('',#17765);
#4588=VERTEX_POINT('',#17767);
#4589=VERTEX_POINT('',#17769);
#4590=VERTEX_POINT('',#17772);
#4591=VERTEX_POINT('',#17773);
#4592=VERTEX_POINT('',#17775);
#4593=VERTEX_POINT('',#17777);
#4594=VERTEX_POINT('',#17779);
#4595=VERTEX_POINT('',#17782);
#4596=VERTEX_POINT('',#17785);
#4597=VERTEX_POINT('',#17787);
#4598=VERTEX_POINT('',#17789);
#4599=VERTEX_POINT('',#17792);
#4600=VERTEX_POINT('',#17795);
#4601=VERTEX_POINT('',#17797);
#4602=VERTEX_POINT('',#17800);
#4603=VERTEX_POINT('',#17802);
#4604=VERTEX_POINT('',#17805);
#4605=VERTEX_POINT('',#17806);
#4606=VERTEX_POINT('',#17815);
#4607=VERTEX_POINT('',#17817);
#4608=VERTEX_POINT('',#17826);
#4609=VERTEX_POINT('',#17828);
#4610=VERTEX_POINT('',#17848);
#4611=VERTEX_POINT('',#17850);
#4612=VERTEX_POINT('',#17870);
#4613=VERTEX_POINT('',#17872);
#4614=VERTEX_POINT('',#17892);
#4615=VERTEX_POINT('',#17894);
#4616=VERTEX_POINT('',#17903);
#4617=VERTEX_POINT('',#17905);
#4618=VERTEX_POINT('',#17925);
#4619=VERTEX_POINT('',#17927);
#4620=VERTEX_POINT('',#17949);
#4621=VERTEX_POINT('',#17950);
#4622=VERTEX_POINT('',#17952);
#4623=VERTEX_POINT('',#17954);
#4624=VERTEX_POINT('',#17958);
#4625=VERTEX_POINT('',#17959);
#4626=VERTEX_POINT('',#17961);
#4627=VERTEX_POINT('',#17963);
#4628=VERTEX_POINT('',#17967);
#4629=VERTEX_POINT('',#17968);
#4630=VERTEX_POINT('',#17970);
#4631=VERTEX_POINT('',#17972);
#4632=VERTEX_POINT('',#17974);
#4633=VERTEX_POINT('',#17976);
#4634=VERTEX_POINT('',#17978);
#4635=VERTEX_POINT('',#17980);
#4636=VERTEX_POINT('',#17982);
#4637=VERTEX_POINT('',#17984);
#4638=VERTEX_POINT('',#17986);
#4639=VERTEX_POINT('',#17988);
#4640=VERTEX_POINT('',#17990);
#4641=VERTEX_POINT('',#17992);
#4642=VERTEX_POINT('',#17994);
#4643=VERTEX_POINT('',#17996);
#4644=VERTEX_POINT('',#17998);
#4645=VERTEX_POINT('',#18000);
#4646=VERTEX_POINT('',#18004);
#4647=VERTEX_POINT('',#18005);
#4648=VERTEX_POINT('',#18007);
#4649=VERTEX_POINT('',#18009);
#4650=VERTEX_POINT('',#18011);
#4651=VERTEX_POINT('',#18013);
#4652=VERTEX_POINT('',#18016);
#4653=VERTEX_POINT('',#18018);
#4654=VERTEX_POINT('',#18020);
#4655=VERTEX_POINT('',#18022);
#4656=VERTEX_POINT('',#18024);
#4657=VERTEX_POINT('',#18026);
#4658=VERTEX_POINT('',#18028);
#4659=VERTEX_POINT('',#18030);
#4660=VERTEX_POINT('',#18034);
#4661=VERTEX_POINT('',#18035);
#4662=VERTEX_POINT('',#18047);
#4663=VERTEX_POINT('',#18048);
#4664=VERTEX_POINT('',#18058);
#4665=VERTEX_POINT('',#18062);
#4666=VERTEX_POINT('',#18063);
#4667=VERTEX_POINT('',#18065);
#4668=VERTEX_POINT('',#18067);
#4669=VERTEX_POINT('',#18071);
#4670=VERTEX_POINT('',#18073);
#4671=VERTEX_POINT('',#18077);
#4672=VERTEX_POINT('',#18079);
#4673=VERTEX_POINT('',#18083);
#4674=VERTEX_POINT('',#18084);
#4675=VERTEX_POINT('',#18086);
#4676=VERTEX_POINT('',#18088);
#4677=VERTEX_POINT('',#18090);
#4678=VERTEX_POINT('',#18094);
#4679=VERTEX_POINT('',#18095);
#4680=VERTEX_POINT('',#18097);
#4681=VERTEX_POINT('',#18099);
#4682=VERTEX_POINT('',#18131);
#4683=VERTEX_POINT('',#18171);
#4684=VERTEX_POINT('',#18172);
#4685=VERTEX_POINT('',#18174);
#4686=VERTEX_POINT('',#18176);
#4687=VERTEX_POINT('',#18208);
#4688=VERTEX_POINT('',#18248);
#4689=VERTEX_POINT('',#18249);
#4690=VERTEX_POINT('',#18251);
#4691=VERTEX_POINT('',#18253);
#4692=VERTEX_POINT('',#18288);
#4693=VERTEX_POINT('',#18325);
#4694=VERTEX_POINT('',#18326);
#4695=VERTEX_POINT('',#18328);
#4696=VERTEX_POINT('',#18330);
#4697=VERTEX_POINT('',#18362);
#4698=VERTEX_POINT('',#18402);
#4699=VERTEX_POINT('',#18403);
#4700=VERTEX_POINT('',#18405);
#4701=VERTEX_POINT('',#18455);
#4702=VERTEX_POINT('',#18457);
#4703=VERTEX_POINT('',#18459);
#4704=VERTEX_POINT('',#18468);
#4705=VERTEX_POINT('',#18472);
#4706=VERTEX_POINT('',#18473);
#4707=VERTEX_POINT('',#18476);
#4708=VERTEX_POINT('',#18478);
#4709=VERTEX_POINT('',#18480);
#4710=VERTEX_POINT('',#18482);
#4711=VERTEX_POINT('',#18484);
#4712=VERTEX_POINT('',#18486);
#4713=VERTEX_POINT('',#18488);
#4714=VERTEX_POINT('',#18490);
#4715=VERTEX_POINT('',#18492);
#4716=VERTEX_POINT('',#18494);
#4717=VERTEX_POINT('',#18496);
#4718=VERTEX_POINT('',#18498);
#4719=VERTEX_POINT('',#18500);
#4720=VERTEX_POINT('',#18502);
#4721=VERTEX_POINT('',#18505);
#4722=VERTEX_POINT('',#18507);
#4723=VERTEX_POINT('',#18509);
#4724=VERTEX_POINT('',#18511);
#4725=VERTEX_POINT('',#18514);
#4726=VERTEX_POINT('',#18516);
#4727=VERTEX_POINT('',#18520);
#4728=VERTEX_POINT('',#18521);
#4729=VERTEX_POINT('',#18524);
#4730=VERTEX_POINT('',#18559);
#4731=VERTEX_POINT('',#18561);
#4732=VERTEX_POINT('',#18565);
#4733=VERTEX_POINT('',#18566);
#4734=VERTEX_POINT('',#18568);
#4735=VERTEX_POINT('',#18570);
#4736=VERTEX_POINT('',#18572);
#4737=VERTEX_POINT('',#18574);
#4738=VERTEX_POINT('',#18576);
#4739=VERTEX_POINT('',#18607);
#4740=VERTEX_POINT('',#18608);
#4741=VERTEX_POINT('',#18610);
#4742=VERTEX_POINT('',#18627);
#4743=VERTEX_POINT('',#18671);
#4744=VERTEX_POINT('',#18673);
#4745=VERTEX_POINT('',#18675);
#4746=VERTEX_POINT('',#18733);
#4747=VERTEX_POINT('',#18734);
#4748=VERTEX_POINT('',#18743);
#4749=VERTEX_POINT('',#18745);
#4750=VERTEX_POINT('',#18754);
#4751=VERTEX_POINT('',#18756);
#4752=VERTEX_POINT('',#18779);
#4753=VERTEX_POINT('',#18780);
#4754=VERTEX_POINT('',#18782);
#4755=VERTEX_POINT('',#18784);
#4756=VERTEX_POINT('',#18791);
#4757=VERTEX_POINT('',#18792);
#4758=VERTEX_POINT('',#18794);
#4759=VERTEX_POINT('',#18796);
#4760=VERTEX_POINT('',#18798);
#4761=VERTEX_POINT('',#18800);
#4762=VERTEX_POINT('',#18831);
#4763=VERTEX_POINT('',#18832);
#4764=VERTEX_POINT('',#18834);
#4765=VERTEX_POINT('',#18836);
#4766=VERTEX_POINT('',#18838);
#4767=VERTEX_POINT('',#18840);
#4768=VERTEX_POINT('',#18883);
#4769=VERTEX_POINT('',#18884);
#4770=VERTEX_POINT('',#18886);
#4771=VERTEX_POINT('',#18888);
#4772=VERTEX_POINT('',#18890);
#4773=VERTEX_POINT('',#18893);
#4774=VERTEX_POINT('',#18897);
#4775=VERTEX_POINT('',#18898);
#4776=VERTEX_POINT('',#18900);
#4777=VERTEX_POINT('',#18902);
#4778=VERTEX_POINT('',#18904);
#4779=VERTEX_POINT('',#18906);
#4780=VERTEX_POINT('',#18908);
#4781=VERTEX_POINT('',#18910);
#4782=VERTEX_POINT('',#18914);
#4783=VERTEX_POINT('',#18915);
#4784=VERTEX_POINT('',#18935);
#4785=VERTEX_POINT('',#18937);
#4786=VERTEX_POINT('',#18939);
#4787=VERTEX_POINT('',#18941);
#4788=VERTEX_POINT('',#18943);
#4789=VERTEX_POINT('',#18945);
#4790=VERTEX_POINT('',#19027);
#4791=VERTEX_POINT('',#19028);
#4792=VERTEX_POINT('',#19030);
#4793=VERTEX_POINT('',#19032);
#4794=VERTEX_POINT('',#19046);
#4795=VERTEX_POINT('',#19129);
#4796=VERTEX_POINT('',#19149);
#4797=VERTEX_POINT('',#19151);
#4798=VERTEX_POINT('',#19158);
#4799=VERTEX_POINT('',#19159);
#4800=VERTEX_POINT('',#19161);
#4801=VERTEX_POINT('',#19163);
#4802=VERTEX_POINT('',#19177);
#4803=VERTEX_POINT('',#19212);
#4804=VERTEX_POINT('',#19226);
#4805=VERTEX_POINT('',#19228);
#4806=VERTEX_POINT('',#19232);
#4807=VERTEX_POINT('',#19233);
#4808=VERTEX_POINT('',#19247);
#4809=VERTEX_POINT('',#19249);
#4810=VERTEX_POINT('',#19251);
#4811=VERTEX_POINT('',#19253);
#4812=VERTEX_POINT('',#19255);
#4813=VERTEX_POINT('',#19257);
#4814=VERTEX_POINT('',#19291);
#4815=VERTEX_POINT('',#19292);
#4816=VERTEX_POINT('',#19294);
#4817=VERTEX_POINT('',#19296);
#4818=VERTEX_POINT('',#19298);
#4819=VERTEX_POINT('',#19300);
#4820=VERTEX_POINT('',#19302);
#4821=VERTEX_POINT('',#19304);
#4822=VERTEX_POINT('',#19360);
#4823=VERTEX_POINT('',#19362);
#4824=VERTEX_POINT('',#19382);
#4825=VERTEX_POINT('',#19384);
#4826=VERTEX_POINT('',#19393);
#4827=VERTEX_POINT('',#19395);
#4828=VERTEX_POINT('',#19451);
#4829=VERTEX_POINT('',#19453);
#4830=VERTEX_POINT('',#19456);
#4831=VERTEX_POINT('',#19458);
#4832=VERTEX_POINT('',#19460);
#4833=VERTEX_POINT('',#19462);
#4834=VERTEX_POINT('',#19464);
#4835=VERTEX_POINT('',#19467);
#4836=VERTEX_POINT('',#19469);
#4837=VERTEX_POINT('',#19471);
#4838=VERTEX_POINT('',#19473);
#4839=VERTEX_POINT('',#19475);
#4840=VERTEX_POINT('',#19477);
#4841=VERTEX_POINT('',#19480);
#4842=VERTEX_POINT('',#19481);
#4843=VERTEX_POINT('',#19483);
#4844=VERTEX_POINT('',#19539);
#4845=VERTEX_POINT('',#19541);
#4846=VERTEX_POINT('',#19543);
#4847=VERTEX_POINT('',#19545);
#4848=VERTEX_POINT('',#19547);
#4849=VERTEX_POINT('',#19603);
#4850=VERTEX_POINT('',#19605);
#4851=VERTEX_POINT('',#19628);
#4852=VERTEX_POINT('',#19638);
#4853=VERTEX_POINT('',#19639);
#4854=VERTEX_POINT('',#19641);
#4855=VERTEX_POINT('',#19697);
#4856=VERTEX_POINT('',#19700);
#4857=VERTEX_POINT('',#19702);
#4858=VERTEX_POINT('',#19758);
#4859=VERTEX_POINT('',#19760);
#4860=VERTEX_POINT('',#19783);
#4861=VERTEX_POINT('',#19793);
#4862=VERTEX_POINT('',#19794);
#4863=VERTEX_POINT('',#19796);
#4864=VERTEX_POINT('',#19798);
#4865=VERTEX_POINT('',#19800);
#4866=VERTEX_POINT('',#19856);
#4867=VERTEX_POINT('',#19858);
#4868=VERTEX_POINT('',#19881);
#4869=VERTEX_POINT('',#19883);
#4870=VERTEX_POINT('',#19892);
#4871=VERTEX_POINT('',#19894);
#4872=VERTEX_POINT('',#19955);
#4873=VERTEX_POINT('',#19956);
#4874=VERTEX_POINT('',#19965);
#4875=VERTEX_POINT('',#19967);
#4876=VERTEX_POINT('',#19978);
#4877=VERTEX_POINT('',#19979);
#4878=VERTEX_POINT('',#19981);
#4879=VERTEX_POINT('',#20016);
#4880=VERTEX_POINT('',#20018);
#4881=VERTEX_POINT('',#20055);
#4882=VERTEX_POINT('',#20056);
#4883=VERTEX_POINT('',#20058);
#4884=VERTEX_POINT('',#20090);
#4885=VERTEX_POINT('',#20092);
#4886=VERTEX_POINT('',#20132);
#4887=VERTEX_POINT('',#20140);
#4888=VERTEX_POINT('',#20144);
#4889=VERTEX_POINT('',#20146);
#4890=VERTEX_POINT('',#20153);
#4891=VERTEX_POINT('',#20155);
#4892=VERTEX_POINT('',#20159);
#4893=VERTEX_POINT('',#20160);
#4894=VERTEX_POINT('',#20162);
#4895=VERTEX_POINT('',#20164);
#4896=VERTEX_POINT('',#20168);
#4897=VERTEX_POINT('',#20169);
#4898=VERTEX_POINT('',#20171);
#4899=VERTEX_POINT('',#20173);
#4900=VERTEX_POINT('',#20177);
#4901=VERTEX_POINT('',#20178);
#4902=VERTEX_POINT('',#20180);
#4903=VERTEX_POINT('',#20190);
#4904=VERTEX_POINT('',#20191);
#4905=VERTEX_POINT('',#20193);
#4906=VERTEX_POINT('',#20195);
#4907=VERTEX_POINT('',#20199);
#4908=VERTEX_POINT('',#20200);
#4909=VERTEX_POINT('',#20202);
#4910=VERTEX_POINT('',#20209);
#4911=VERTEX_POINT('',#20211);
#4912=VERTEX_POINT('',#20215);
#4913=VERTEX_POINT('',#20216);
#4914=VERTEX_POINT('',#20221);
#4915=VERTEX_POINT('',#20222);
#4916=VERTEX_POINT('',#20224);
#4917=VERTEX_POINT('',#20226);
#4918=VERTEX_POINT('',#20230);
#4919=VERTEX_POINT('',#20233);
#4920=VERTEX_POINT('',#20235);
#4921=VERTEX_POINT('',#20237);
#4922=VERTEX_POINT('',#20250);
#4923=VERTEX_POINT('',#20251);
#4924=VERTEX_POINT('',#20253);
#4925=VERTEX_POINT('',#20303);
#4926=VERTEX_POINT('',#20305);
#4927=VERTEX_POINT('',#20307);
#4928=VERTEX_POINT('',#20316);
#4929=VERTEX_POINT('',#20320);
#4930=VERTEX_POINT('',#20322);
#4931=VERTEX_POINT('',#20324);
#4932=VERTEX_POINT('',#20326);
#4933=VERTEX_POINT('',#20361);
#4934=VERTEX_POINT('',#20363);
#4935=VERTEX_POINT('',#20367);
#4936=VERTEX_POINT('',#20369);
#4937=VERTEX_POINT('',#20371);
#4938=VERTEX_POINT('',#20373);
#4939=VERTEX_POINT('',#20375);
#4940=VERTEX_POINT('',#20406);
#4941=VERTEX_POINT('',#20407);
#4942=VERTEX_POINT('',#20409);
#4943=VERTEX_POINT('',#20426);
#4944=VERTEX_POINT('',#20470);
#4945=VERTEX_POINT('',#20472);
#4946=VERTEX_POINT('',#20474);
#4947=VERTEX_POINT('',#20532);
#4948=VERTEX_POINT('',#20533);
#4949=VERTEX_POINT('',#20535);
#4950=VERTEX_POINT('',#20537);
#4951=VERTEX_POINT('',#20541);
#4952=VERTEX_POINT('',#20542);
#4953=VERTEX_POINT('',#20544);
#4954=VERTEX_POINT('',#20546);
#4955=VERTEX_POINT('',#20548);
#4956=VERTEX_POINT('',#20550);
#4957=VERTEX_POINT('',#20593);
#4958=VERTEX_POINT('',#20594);
#4959=VERTEX_POINT('',#20596);
#4960=VERTEX_POINT('',#20598);
#4961=VERTEX_POINT('',#20600);
#4962=VERTEX_POINT('',#20603);
#4963=VERTEX_POINT('',#20607);
#4964=VERTEX_POINT('',#20608);
#4965=VERTEX_POINT('',#20610);
#4966=VERTEX_POINT('',#20612);
#4967=VERTEX_POINT('',#20614);
#4968=VERTEX_POINT('',#20616);
#4969=VERTEX_POINT('',#20618);
#4970=VERTEX_POINT('',#20620);
#4971=VERTEX_POINT('',#20624);
#4972=VERTEX_POINT('',#20625);
#4973=VERTEX_POINT('',#20627);
#4974=VERTEX_POINT('',#20629);
#4975=VERTEX_POINT('',#20631);
#4976=VERTEX_POINT('',#20633);
#4977=VERTEX_POINT('',#20635);
#4978=VERTEX_POINT('',#20649);
#4979=VERTEX_POINT('',#20740);
#4980=VERTEX_POINT('',#20741);
#4981=VERTEX_POINT('',#20743);
#4982=VERTEX_POINT('',#20745);
#4983=VERTEX_POINT('',#20747);
#4984=VERTEX_POINT('',#20761);
#4985=VERTEX_POINT('',#20796);
#4986=VERTEX_POINT('',#20810);
#4987=VERTEX_POINT('',#20817);
#4988=VERTEX_POINT('',#20818);
#4989=VERTEX_POINT('',#20827);
#4990=VERTEX_POINT('',#20829);
#4991=VERTEX_POINT('',#20840);
#4992=VERTEX_POINT('',#20841);
#4993=VERTEX_POINT('',#20843);
#4994=VERTEX_POINT('',#20878);
#4995=VERTEX_POINT('',#20880);
#4996=VERTEX_POINT('',#20917);
#4997=VERTEX_POINT('',#20918);
#4998=VERTEX_POINT('',#20926);
#4999=VERTEX_POINT('',#20928);
#5000=VERTEX_POINT('',#20932);
#5001=VERTEX_POINT('',#20940);
#5002=VERTEX_POINT('',#20944);
#5003=VERTEX_POINT('',#20949);
#5004=VERTEX_POINT('',#20950);
#5005=VERTEX_POINT('',#20952);
#5006=VERTEX_POINT('',#20954);
#5007=VERTEX_POINT('',#20958);
#5008=VERTEX_POINT('',#20959);
#5009=VERTEX_POINT('',#20961);
#5010=VERTEX_POINT('',#20971);
#5011=VERTEX_POINT('',#20972);
#5012=VERTEX_POINT('',#20974);
#5013=VERTEX_POINT('',#20976);
#5014=VERTEX_POINT('',#20980);
#5015=VERTEX_POINT('',#20981);
#5016=VERTEX_POINT('',#20983);
#5017=VERTEX_POINT('',#20994);
#5018=VERTEX_POINT('',#20995);
#5019=VERTEX_POINT('',#21001);
#5020=VERTEX_POINT('',#21003);
#5021=VERTEX_POINT('',#21007);
#5022=VERTEX_POINT('',#21009);
#5023=VERTEX_POINT('',#21011);
#5024=VERTEX_POINT('',#21014);
#5025=VERTEX_POINT('',#21025);
#5026=VERTEX_POINT('',#21026);
#5027=VERTEX_POINT('',#21028);
#5028=VERTEX_POINT('',#21078);
#5029=VERTEX_POINT('',#21080);
#5030=VERTEX_POINT('',#21082);
#5031=VERTEX_POINT('',#21091);
#5032=VERTEX_POINT('',#21095);
#5033=VERTEX_POINT('',#21096);
#5034=VERTEX_POINT('',#21098);
#5035=VERTEX_POINT('',#21100);
#5036=VERTEX_POINT('',#21102);
#5037=VERTEX_POINT('',#21104);
#5038=VERTEX_POINT('',#21139);
#5039=VERTEX_POINT('',#21143);
#5040=VERTEX_POINT('',#21144);
#5041=VERTEX_POINT('',#21146);
#5042=VERTEX_POINT('',#21148);
#5043=VERTEX_POINT('',#21150);
#5044=VERTEX_POINT('',#21152);
#5045=VERTEX_POINT('',#21154);
#5046=VERTEX_POINT('',#21185);
#5047=VERTEX_POINT('',#21186);
#5048=VERTEX_POINT('',#21188);
#5049=VERTEX_POINT('',#21205);
#5050=VERTEX_POINT('',#21249);
#5051=VERTEX_POINT('',#21251);
#5052=VERTEX_POINT('',#21253);
#5053=VERTEX_POINT('',#21314);
#5054=VERTEX_POINT('',#21316);
#5055=VERTEX_POINT('',#21318);
#5056=VERTEX_POINT('',#21320);
#5057=VERTEX_POINT('',#21363);
#5058=VERTEX_POINT('',#21364);
#5059=VERTEX_POINT('',#21384);
#5060=VERTEX_POINT('',#21386);
#5061=VERTEX_POINT('',#21388);
#5062=VERTEX_POINT('',#21390);
#5063=VERTEX_POINT('',#21392);
#5064=VERTEX_POINT('',#21394);
#5065=VERTEX_POINT('',#21479);
#5066=VERTEX_POINT('',#21480);
#5067=VERTEX_POINT('',#21482);
#5068=VERTEX_POINT('',#21484);
#5069=VERTEX_POINT('',#21498);
#5070=VERTEX_POINT('',#21533);
#5071=VERTEX_POINT('',#21547);
#5072=VERTEX_POINT('',#21549);
#5073=VERTEX_POINT('',#21556);
#5074=VERTEX_POINT('',#21557);
#5075=VERTEX_POINT('',#21566);
#5076=VERTEX_POINT('',#21568);
#5077=VERTEX_POINT('',#21579);
#5078=VERTEX_POINT('',#21580);
#5079=VERTEX_POINT('',#21582);
#5080=VERTEX_POINT('',#21617);
#5081=VERTEX_POINT('',#21619);
#5082=VERTEX_POINT('',#21656);
#5083=VERTEX_POINT('',#21657);
#5084=VERTEX_POINT('',#21665);
#5085=VERTEX_POINT('',#21667);
#5086=VERTEX_POINT('',#21671);
#5087=VERTEX_POINT('',#21673);
#5088=VERTEX_POINT('',#21680);
#5089=VERTEX_POINT('',#21682);
#5090=VERTEX_POINT('',#21686);
#5091=VERTEX_POINT('',#21687);
#5092=VERTEX_POINT('',#21692);
#5093=VERTEX_POINT('',#21693);
#5094=VERTEX_POINT('',#21695);
#5095=VERTEX_POINT('',#21697);
#5096=VERTEX_POINT('',#21701);
#5097=VERTEX_POINT('',#21702);
#5098=VERTEX_POINT('',#21704);
#5099=VERTEX_POINT('',#21714);
#5100=VERTEX_POINT('',#21715);
#5101=VERTEX_POINT('',#21717);
#5102=VERTEX_POINT('',#21719);
#5103=VERTEX_POINT('',#21723);
#5104=VERTEX_POINT('',#21730);
#5105=VERTEX_POINT('',#21732);
#5106=VERTEX_POINT('',#21736);
#5107=VERTEX_POINT('',#21738);
#5108=VERTEX_POINT('',#21742);
#5109=VERTEX_POINT('',#21743);
#5110=VERTEX_POINT('',#21745);
#5111=VERTEX_POINT('',#21747);
#5112=VERTEX_POINT('',#21751);
#5113=VERTEX_POINT('',#21752);
#5114=VERTEX_POINT('',#21754);
#5115=VERTEX_POINT('',#21756);
#5116=VERTEX_POINT('',#21758);
#5117=VERTEX_POINT('',#21760);
#5118=VERTEX_POINT('',#21762);
#5119=VERTEX_POINT('',#21764);
#5120=VERTEX_POINT('',#21767);
#5121=VERTEX_POINT('',#21778);
#5122=VERTEX_POINT('',#21779);
#5123=VERTEX_POINT('',#21781);
#5124=VERTEX_POINT('',#21831);
#5125=VERTEX_POINT('',#21833);
#5126=VERTEX_POINT('',#21835);
#5127=VERTEX_POINT('',#21844);
#5128=VERTEX_POINT('',#21848);
#5129=VERTEX_POINT('',#21850);
#5130=VERTEX_POINT('',#21852);
#5131=VERTEX_POINT('',#21887);
#5132=VERTEX_POINT('',#21889);
#5133=VERTEX_POINT('',#21893);
#5134=VERTEX_POINT('',#21894);
#5135=VERTEX_POINT('',#21897);
#5136=VERTEX_POINT('',#21899);
#5137=VERTEX_POINT('',#21901);
#5138=VERTEX_POINT('',#21932);
#5139=VERTEX_POINT('',#21933);
#5140=VERTEX_POINT('',#21935);
#5141=VERTEX_POINT('',#21952);
#5142=VERTEX_POINT('',#21996);
#5143=VERTEX_POINT('',#21998);
#5144=VERTEX_POINT('',#22000);
#5145=VERTEX_POINT('',#22058);
#5146=VERTEX_POINT('',#22059);
#5147=VERTEX_POINT('',#22061);
#5148=VERTEX_POINT('',#22063);
#5149=VERTEX_POINT('',#22065);
#5150=VERTEX_POINT('',#22067);
#5151=VERTEX_POINT('',#22069);
#5152=VERTEX_POINT('',#22071);
#5153=VERTEX_POINT('',#22075);
#5154=VERTEX_POINT('',#22076);
#5155=VERTEX_POINT('',#22078);
#5156=VERTEX_POINT('',#22080);
#5157=VERTEX_POINT('',#22082);
#5158=VERTEX_POINT('',#22085);
#5159=VERTEX_POINT('',#22095);
#5160=VERTEX_POINT('',#22096);
#5161=VERTEX_POINT('',#22105);
#5162=VERTEX_POINT('',#22107);
#5163=VERTEX_POINT('',#22118);
#5164=VERTEX_POINT('',#22119);
#5165=VERTEX_POINT('',#22127);
#5166=VERTEX_POINT('',#22129);
#5167=VERTEX_POINT('',#22133);
#5168=VERTEX_POINT('',#22135);
#5169=VERTEX_POINT('',#22142);
#5170=VERTEX_POINT('',#22144);
#5171=VERTEX_POINT('',#22151);
#5172=VERTEX_POINT('',#22152);
#5173=VERTEX_POINT('',#22154);
#5174=VERTEX_POINT('',#22156);
#5175=VERTEX_POINT('',#22160);
#5176=VERTEX_POINT('',#22170);
#5177=VERTEX_POINT('',#22171);
#5178=VERTEX_POINT('',#22173);
#5179=VERTEX_POINT('',#22175);
#5180=VERTEX_POINT('',#22179);
#5181=VERTEX_POINT('',#22180);
#5182=VERTEX_POINT('',#22182);
#5183=VERTEX_POINT('',#22189);
#5184=VERTEX_POINT('',#22191);
#5185=VERTEX_POINT('',#22195);
#5186=VERTEX_POINT('',#22196);
#5187=VERTEX_POINT('',#22201);
#5188=VERTEX_POINT('',#22202);
#5189=VERTEX_POINT('',#22208);
#5190=VERTEX_POINT('',#22210);
#5191=VERTEX_POINT('',#22212);
#5192=VERTEX_POINT('',#22214);
#5193=VERTEX_POINT('',#22216);
#5194=VERTEX_POINT('',#22218);
#5195=VERTEX_POINT('',#22314);
#5196=VERTEX_POINT('',#22321);
#5197=VERTEX_POINT('',#22412);
#5198=VERTEX_POINT('',#22543);
#5199=VERTEX_POINT('',#22636);
#5200=VERTEX_POINT('',#22746);
#5201=VERTEX_POINT('',#22747);
#5202=VERTEX_POINT('',#22824);
#5203=VERTEX_POINT('',#22917);
#5204=VERTEX_POINT('',#23067);
#5205=VERTEX_POINT('',#23135);
#5206=VERTEX_POINT('',#23142);
#5207=VERTEX_POINT('',#23233);
#5208=VERTEX_POINT('',#23364);
#5209=VERTEX_POINT('',#23457);
#5210=VERTEX_POINT('',#23567);
#5211=VERTEX_POINT('',#23568);
#5212=VERTEX_POINT('',#23645);
#5213=VERTEX_POINT('',#23738);
#5214=VERTEX_POINT('',#23888);
#5215=VERTEX_POINT('',#29491);
#5216=VERTEX_POINT('',#29498);
#5217=VERTEX_POINT('',#29591);
#5218=VERTEX_POINT('',#29741);
#5219=VERTEX_POINT('',#29832);
#5220=VERTEX_POINT('',#29951);
#5221=VERTEX_POINT('',#29952);
#5222=VERTEX_POINT('',#30029);
#5223=VERTEX_POINT('',#30122);
#5224=VERTEX_POINT('',#30272);
#5225=VERTEX_POINT('',#30340);
#5226=VERTEX_POINT('',#30347);
#5227=VERTEX_POINT('',#30438);
#5228=VERTEX_POINT('',#30569);
#5229=VERTEX_POINT('',#30662);
#5230=VERTEX_POINT('',#30772);
#5231=VERTEX_POINT('',#30773);
#5232=VERTEX_POINT('',#30850);
#5233=VERTEX_POINT('',#30943);
#5234=VERTEX_POINT('',#31132);
#5235=VERTEX_POINT('',#32152);
#5236=VERTEX_POINT('',#32160);
#5237=VERTEX_POINT('',#32168);
#5238=VERTEX_POINT('',#32197);
#5239=VERTEX_POINT('',#32199);
#5240=VERTEX_POINT('',#32201);
#5241=VERTEX_POINT('',#32212);
#5242=VERTEX_POINT('',#32214);
#5243=VERTEX_POINT('',#32225);
#5244=VERTEX_POINT('',#32236);
#5245=VERTEX_POINT('',#32238);
#5246=VERTEX_POINT('',#32249);
#5247=VERTEX_POINT('',#32260);
#5248=VERTEX_POINT('',#32262);
#5249=VERTEX_POINT('',#32264);
#5250=VERTEX_POINT('',#32275);
#5251=VERTEX_POINT('',#32286);
#5252=VERTEX_POINT('',#32288);
#5253=VERTEX_POINT('',#32299);
#5254=VERTEX_POINT('',#32310);
#5255=VERTEX_POINT('',#32312);
#5256=VERTEX_POINT('',#32323);
#5257=VERTEX_POINT('',#32334);
#5258=VERTEX_POINT('',#32336);
#5259=VERTEX_POINT('',#32347);
#5260=VERTEX_POINT('',#32358);
#5261=VERTEX_POINT('',#32360);
#5262=VERTEX_POINT('',#32362);
#5263=VERTEX_POINT('',#32372);
#5264=VERTEX_POINT('',#32374);
#5265=VERTEX_POINT('',#32378);
#5266=VERTEX_POINT('',#32380);
#5267=VERTEX_POINT('',#32384);
#5268=VERTEX_POINT('',#32386);
#5269=VERTEX_POINT('',#32390);
#5270=VERTEX_POINT('',#32394);
#5271=VERTEX_POINT('',#32395);
#5272=VERTEX_POINT('',#32406);
#5273=VERTEX_POINT('',#32417);
#5274=VERTEX_POINT('',#32420);
#5275=VERTEX_POINT('',#32431);
#5276=VERTEX_POINT('',#32451);
#5277=VERTEX_POINT('',#32462);
#5278=VERTEX_POINT('',#32482);
#5279=VERTEX_POINT('',#32493);
#5280=VERTEX_POINT('',#32501);
#5281=VERTEX_POINT('',#32515);
#5282=VERTEX_POINT('',#32526);
#5283=VERTEX_POINT('',#32546);
#5284=VERTEX_POINT('',#32557);
#5285=VERTEX_POINT('',#32577);
#5286=VERTEX_POINT('',#32588);
#5287=VERTEX_POINT('',#32608);
#5288=VERTEX_POINT('',#32619);
#5289=VERTEX_POINT('',#32741);
#5290=VERTEX_POINT('',#32748);
#5291=VERTEX_POINT('',#33028);
#5292=VERTEX_POINT('',#33650);
#5293=VERTEX_POINT('',#33657);
#5294=VERTEX_POINT('',#33965);
#5295=VERTEX_POINT('',#34361);
#5296=VERTEX_POINT('',#34368);
#5297=VERTEX_POINT('',#34676);
#5298=VERTEX_POINT('',#35072);
#5299=VERTEX_POINT('',#35079);
#5300=VERTEX_POINT('',#35387);
#5301=VERTEX_POINT('',#36472);
#5302=VERTEX_POINT('',#36479);
#5303=VERTEX_POINT('',#36787);
#5304=VERTEX_POINT('',#37183);
#5305=VERTEX_POINT('',#37190);
#5306=VERTEX_POINT('',#37498);
#5307=EDGE_CURVE('',#4301,#4301,#3413,.T.);
#5308=EDGE_CURVE('',#4301,#4302,#2537,.T.);
#5309=EDGE_CURVE('',#4302,#4302,#3414,.T.);
#5310=EDGE_CURVE('',#4303,#4303,#3415,.T.);
#5311=EDGE_CURVE('',#4303,#4304,#2538,.T.);
#5312=EDGE_CURVE('',#4304,#4304,#3416,.T.);
#5313=EDGE_CURVE('',#4305,#4305,#3417,.T.);
#5314=EDGE_CURVE('',#4305,#4306,#2539,.T.);
#5315=EDGE_CURVE('',#4306,#4306,#3418,.T.);
#5316=EDGE_CURVE('',#4307,#4307,#3419,.T.);
#5317=EDGE_CURVE('',#4307,#4308,#2540,.T.);
#5318=EDGE_CURVE('',#4308,#4308,#3420,.T.);
#5319=EDGE_CURVE('',#4309,#4310,#3421,.T.);
#5320=EDGE_CURVE('',#4310,#4309,#3422,.T.);
#5321=EDGE_CURVE('',#4310,#4311,#3423,.T.);
#5322=EDGE_CURVE('',#4311,#4311,#3424,.T.);
#5323=EDGE_CURVE('',#4312,#4312,#3425,.T.);
#5324=EDGE_CURVE('',#4312,#4313,#3426,.T.);
#5325=EDGE_CURVE('',#4314,#4313,#3427,.T.);
#5326=EDGE_CURVE('',#4313,#4314,#3428,.T.);
#5327=EDGE_CURVE('',#4315,#4315,#3429,.T.);
#5328=EDGE_CURVE('',#4315,#4316,#3430,.T.);
#5329=EDGE_CURVE('',#4316,#4316,#3431,.T.);
#5330=EDGE_CURVE('',#4317,#4317,#3432,.T.);
#5331=EDGE_CURVE('',#4317,#4318,#3433,.T.);
#5332=EDGE_CURVE('',#4319,#4318,#3434,.T.);
#5333=EDGE_CURVE('',#4318,#4319,#3435,.T.);
#5334=EDGE_CURVE('',#4320,#4321,#3436,.T.);
#5335=EDGE_CURVE('',#4320,#4322,#3437,.T.);
#5336=EDGE_CURVE('',#4323,#4322,#3438,.T.);
#5337=EDGE_CURVE('',#4321,#4323,#3439,.T.);
#5338=EDGE_CURVE('',#4324,#4325,#3440,.T.);
#5339=EDGE_CURVE('',#4326,#4324,#3441,.T.);
#5340=EDGE_CURVE('',#4327,#4326,#3442,.T.);
#5341=EDGE_CURVE('',#4325,#4327,#3443,.T.);
#5342=EDGE_CURVE('',#4328,#4329,#3444,.T.);
#5343=EDGE_CURVE('',#4330,#4328,#3445,.T.);
#5344=EDGE_CURVE('',#4331,#4330,#3446,.T.);
#5345=EDGE_CURVE('',#4331,#4329,#3447,.T.);
#5346=EDGE_CURVE('',#4332,#4333,#3448,.T.);
#5347=EDGE_CURVE('',#4334,#4332,#3449,.T.);
#5348=EDGE_CURVE('',#4335,#4334,#3450,.T.);
#5349=EDGE_CURVE('',#4333,#4335,#3451,.T.);
#5350=EDGE_CURVE('',#4336,#4337,#3452,.T.);
#5351=EDGE_CURVE('',#4337,#4336,#3453,.T.);
#5352=EDGE_CURVE('',#4337,#4338,#3454,.T.);
#5353=EDGE_CURVE('',#4338,#4338,#3455,.T.);
#5354=EDGE_CURVE('',#4339,#4339,#3456,.T.);
#5355=EDGE_CURVE('',#4339,#4340,#3457,.T.);
#5356=EDGE_CURVE('',#4341,#4340,#3458,.T.);
#5357=EDGE_CURVE('',#4340,#4341,#3459,.T.);
#5358=EDGE_CURVE('',#4342,#4342,#3460,.T.);
#5359=EDGE_CURVE('',#4342,#4343,#3461,.T.);
#5360=EDGE_CURVE('',#4344,#4343,#3462,.T.);
#5361=EDGE_CURVE('',#4343,#4344,#3463,.T.);
#5362=EDGE_CURVE('',#4345,#4345,#3464,.T.);
#5363=EDGE_CURVE('',#4345,#4346,#3465,.T.);
#5364=EDGE_CURVE('',#4347,#4346,#3466,.T.);
#5365=EDGE_CURVE('',#4346,#4347,#3467,.T.);
#5366=EDGE_CURVE('',#4348,#4349,#3468,.T.);
#5367=EDGE_CURVE('',#4350,#4348,#3469,.T.);
#5368=EDGE_CURVE('',#4351,#4350,#3470,.T.);
#5369=EDGE_CURVE('',#4351,#4349,#3471,.T.);
#5370=EDGE_CURVE('',#4352,#4353,#3472,.T.);
#5371=EDGE_CURVE('',#4354,#4352,#3473,.T.);
#5372=EDGE_CURVE('',#4355,#4354,#3474,.T.);
#5373=EDGE_CURVE('',#4353,#4355,#3475,.T.);
#5374=EDGE_CURVE('',#4356,#4357,#3476,.T.);
#5375=EDGE_CURVE('',#4356,#4358,#3477,.T.);
#5376=EDGE_CURVE('',#4359,#4358,#3478,.T.);
#5377=EDGE_CURVE('',#4357,#4359,#3479,.T.);
#5378=EDGE_CURVE('',#4360,#4361,#3480,.T.);
#5379=EDGE_CURVE('',#4362,#4360,#3481,.T.);
#5380=EDGE_CURVE('',#4363,#4362,#3482,.T.);
#5381=EDGE_CURVE('',#4361,#4363,#3483,.T.);
#5382=EDGE_CURVE('',#4364,#4364,#3484,.T.);
#5383=EDGE_CURVE('',#4364,#4365,#3485,.T.);
#5384=EDGE_CURVE('',#4365,#4365,#3486,.T.);
#5385=EDGE_CURVE('',#4366,#4366,#3487,.T.);
#5386=EDGE_CURVE('',#4366,#4367,#3488,.T.);
#5387=EDGE_CURVE('',#4367,#4367,#3489,.T.);
#5388=EDGE_CURVE('',#4368,#4368,#3490,.T.);
#5389=EDGE_CURVE('',#4368,#4369,#3491,.T.);
#5390=EDGE_CURVE('',#4370,#4369,#3492,.T.);
#5391=EDGE_CURVE('',#4369,#4370,#3493,.T.);
#5392=EDGE_CURVE('',#4371,#4371,#3494,.T.);
#5393=EDGE_CURVE('',#4371,#4372,#3495,.T.);
#5394=EDGE_CURVE('',#4372,#4372,#3496,.T.);
#5395=EDGE_CURVE('',#4373,#4374,#3497,.T.);
#5396=EDGE_CURVE('',#4373,#4375,#3498,.T.);
#5397=EDGE_CURVE('',#4376,#4375,#3499,.T.);
#5398=EDGE_CURVE('',#4374,#4376,#3500,.T.);
#5399=EDGE_CURVE('',#4377,#4378,#3501,.T.);
#5400=EDGE_CURVE('',#4379,#4377,#3502,.T.);
#5401=EDGE_CURVE('',#4380,#4379,#3503,.T.);
#5402=EDGE_CURVE('',#4380,#4378,#3504,.T.);
#5403=EDGE_CURVE('',#4381,#4382,#3505,.T.);
#5404=EDGE_CURVE('',#4381,#4383,#3506,.T.);
#5405=EDGE_CURVE('',#4383,#4383,#3507,.T.);
#5406=EDGE_CURVE('',#4382,#4381,#3508,.T.);
#5407=EDGE_CURVE('',#4384,#4384,#3509,.T.);
#5408=EDGE_CURVE('',#4384,#4385,#3510,.T.);
#5409=EDGE_CURVE('',#4386,#4385,#3511,.T.);
#5410=EDGE_CURVE('',#4385,#4386,#3512,.T.);
#5411=EDGE_CURVE('',#4387,#4387,#3513,.T.);
#5412=EDGE_CURVE('',#4387,#4388,#3514,.T.);
#5413=EDGE_CURVE('',#4389,#4388,#3515,.T.);
#5414=EDGE_CURVE('',#4388,#4389,#3516,.T.);
#5415=EDGE_CURVE('',#4390,#4390,#3517,.T.);
#5416=EDGE_CURVE('',#4390,#4391,#3518,.T.);
#5417=EDGE_CURVE('',#4392,#4391,#3519,.T.);
#5418=EDGE_CURVE('',#4391,#4392,#3520,.T.);
#5419=EDGE_CURVE('',#4393,#4394,#3521,.T.);
#5420=EDGE_CURVE('',#4395,#4393,#3522,.T.);
#5421=EDGE_CURVE('',#4396,#4395,#3523,.T.);
#5422=EDGE_CURVE('',#4396,#4394,#3524,.T.);
#5423=EDGE_CURVE('',#4397,#4398,#3525,.T.);
#5424=EDGE_CURVE('',#4399,#4397,#3526,.T.);
#5425=EDGE_CURVE('',#4400,#4399,#3527,.T.);
#5426=EDGE_CURVE('',#4400,#4398,#3528,.T.);
#5427=EDGE_CURVE('',#4401,#4402,#3529,.T.);
#5428=EDGE_CURVE('',#4401,#4403,#3530,.T.);
#5429=EDGE_CURVE('',#4404,#4403,#3531,.T.);
#5430=EDGE_CURVE('',#4402,#4404,#3532,.T.);
#5431=EDGE_CURVE('',#4405,#4406,#3533,.T.);
#5432=EDGE_CURVE('',#4407,#4405,#3534,.T.);
#5433=EDGE_CURVE('',#4408,#4407,#3535,.T.);
#5434=EDGE_CURVE('',#4408,#4406,#3536,.T.);
#5435=EDGE_CURVE('',#4409,#4410,#3537,.T.);
#5436=EDGE_CURVE('',#4411,#4409,#3538,.T.);
#5437=EDGE_CURVE('',#4412,#4411,#3539,.T.);
#5438=EDGE_CURVE('',#4412,#4410,#3540,.T.);
#5439=EDGE_CURVE('',#4413,#4414,#3541,.T.);
#5440=EDGE_CURVE('',#4413,#4415,#3542,.T.);
#5441=EDGE_CURVE('',#4416,#4415,#3543,.T.);
#5442=EDGE_CURVE('',#4414,#4416,#3544,.T.);
#5443=EDGE_CURVE('',#4417,#4418,#3545,.T.);
#5444=EDGE_CURVE('',#4419,#4417,#2541,.T.);
#5445=EDGE_CURVE('',#4419,#4420,#3546,.T.);
#5446=EDGE_CURVE('',#4418,#4420,#2542,.T.);
#5447=EDGE_CURVE('',#4421,#4422,#3547,.T.);
#5448=EDGE_CURVE('',#4423,#4421,#2543,.T.);
#5449=EDGE_CURVE('',#4423,#4424,#3548,.T.);
#5450=EDGE_CURVE('',#4422,#4424,#2544,.T.);
#5451=EDGE_CURVE('',#4425,#4426,#3549,.T.);
#5452=EDGE_CURVE('',#4427,#4426,#2545,.T.);
#5453=EDGE_CURVE('',#4428,#4427,#3550,.T.);
#5454=EDGE_CURVE('',#4425,#4428,#2546,.T.);
#5455=EDGE_CURVE('',#4425,#4429,#3551,.T.);
#5456=EDGE_CURVE('',#4430,#4429,#3552,.T.);
#5457=EDGE_CURVE('',#4426,#4430,#3553,.T.);
#5458=EDGE_CURVE('',#4431,#4432,#3554,.T.);
#5459=EDGE_CURVE('',#4433,#4432,#2547,.T.);
#5460=EDGE_CURVE('',#4434,#4433,#3555,.T.);
#5461=EDGE_CURVE('',#4431,#4434,#2548,.T.);
#5462=EDGE_CURVE('',#4435,#4436,#3556,.T.);
#5463=EDGE_CURVE('',#4437,#4435,#2549,.T.);
#5464=EDGE_CURVE('',#4437,#4438,#3557,.T.);
#5465=EDGE_CURVE('',#4436,#4438,#2550,.T.);
#5466=EDGE_CURVE('',#4439,#4440,#3558,.T.);
#5467=EDGE_CURVE('',#4441,#4440,#2551,.T.);
#5468=EDGE_CURVE('',#4442,#4441,#3559,.T.);
#5469=EDGE_CURVE('',#4439,#4442,#2552,.T.);
#5470=EDGE_CURVE('',#4443,#4444,#3560,.T.);
#5471=EDGE_CURVE('',#4445,#4443,#2553,.T.);
#5472=EDGE_CURVE('',#4445,#4446,#3561,.T.);
#5473=EDGE_CURVE('',#4444,#4446,#2554,.T.);
#5474=EDGE_CURVE('',#4447,#4448,#3562,.T.);
#5475=EDGE_CURVE('',#4447,#4449,#3563,.T.);
#5476=EDGE_CURVE('',#4450,#4449,#3564,.T.);
#5477=EDGE_CURVE('',#4450,#4448,#3565,.T.);
#5478=EDGE_CURVE('',#4451,#4452,#3566,.T.);
#5479=EDGE_CURVE('',#4453,#4451,#3567,.T.);
#5480=EDGE_CURVE('',#4454,#4453,#3568,.T.);
#5481=EDGE_CURVE('',#4454,#4452,#3569,.T.);
#5482=EDGE_CURVE('',#4455,#4456,#3570,.T.);
#5483=EDGE_CURVE('',#4455,#4457,#3571,.T.);
#5484=EDGE_CURVE('',#4458,#4457,#3572,.T.);
#5485=EDGE_CURVE('',#4456,#4458,#3573,.T.);
#5486=EDGE_CURVE('',#4459,#4460,#3574,.T.);
#5487=EDGE_CURVE('',#4461,#4460,#2555,.T.);
#5488=EDGE_CURVE('',#4461,#4462,#3575,.T.);
#5489=EDGE_CURVE('',#4459,#4462,#2556,.T.);
#5490=EDGE_CURVE('',#4463,#4454,#3576,.T.);
#5491=EDGE_CURVE('',#4454,#4457,#2557,.T.);
#5492=EDGE_CURVE('',#4457,#4464,#3577,.T.);
#5493=EDGE_CURVE('',#4464,#4463,#2558,.T.);
#5494=EDGE_CURVE('',#4382,#4392,#2559,.T.);
#5495=EDGE_CURVE('',#4389,#4386,#2560,.T.);
#5496=EDGE_CURVE('',#4465,#4403,#2561,.T.);
#5497=EDGE_CURVE('',#4465,#4466,#3578,.T.);
#5498=EDGE_CURVE('',#4404,#4466,#2562,.T.);
#5499=EDGE_CURVE('',#4467,#4468,#3579,.T.);
#5500=EDGE_CURVE('',#4469,#4468,#2563,.T.);
#5501=EDGE_CURVE('',#4469,#4470,#3580,.T.);
#5502=EDGE_CURVE('',#4467,#4470,#2564,.T.);
#5503=EDGE_CURVE('',#4375,#4471,#3581,.T.);
#5504=EDGE_CURVE('',#4471,#4472,#2565,.T.);
#5505=EDGE_CURVE('',#4472,#4380,#3582,.T.);
#5506=EDGE_CURVE('',#4380,#4375,#2566,.T.);
#5507=EDGE_CURVE('',#4364,#4372,#2567,.T.);
#5508=EDGE_CURVE('',#4370,#4367,#2568,.T.);
#5509=EDGE_CURVE('',#4395,#4473,#419,.T.);
#5510=EDGE_CURVE('',#4473,#4474,#3583,.T.);
#5511=EDGE_CURVE('',#4474,#4475,#420,.T.);
#5512=EDGE_CURVE('',#4475,#4476,#421,.T.);
#5513=EDGE_CURVE('',#4476,#4477,#3584,.T.);
#5514=EDGE_CURVE('',#4477,#4396,#422,.T.);
#5515=EDGE_CURVE('',#4478,#4407,#2569,.T.);
#5516=EDGE_CURVE('',#4478,#4479,#3585,.T.);
#5517=EDGE_CURVE('',#4408,#4479,#2570,.T.);
#5518=EDGE_CURVE('',#4480,#4481,#3586,.T.);
#5519=EDGE_CURVE('',#4482,#4481,#2571,.T.);
#5520=EDGE_CURVE('',#4482,#4483,#3587,.T.);
#5521=EDGE_CURVE('',#4480,#4483,#2572,.T.);
#5522=EDGE_CURVE('',#4353,#4360,#2573,.T.);
#5523=EDGE_CURVE('',#4361,#4352,#2574,.T.);
#5524=EDGE_CURVE('',#4336,#4347,#2575,.T.);
#5525=EDGE_CURVE('',#4344,#4341,#2576,.T.);
#5526=EDGE_CURVE('',#4484,#4485,#3588,.T.);
#5527=EDGE_CURVE('',#4485,#4486,#423,.T.);
#5528=EDGE_CURVE('',#4486,#4487,#3589,.T.);
#5529=EDGE_CURVE('',#4487,#4488,#424,.T.);
#5530=EDGE_CURVE('',#4488,#4489,#425,.T.);
#5531=EDGE_CURVE('',#4489,#4490,#3590,.T.);
#5532=EDGE_CURVE('',#4490,#4484,#426,.T.);
#5533=EDGE_CURVE('',#4491,#4492,#3591,.T.);
#5534=EDGE_CURVE('',#4416,#4492,#2577,.T.);
#5535=EDGE_CURVE('',#4491,#4415,#2578,.T.);
#5536=EDGE_CURVE('',#4331,#4322,#2579,.T.);
#5537=EDGE_CURVE('',#4323,#4330,#2580,.T.);
#5538=EDGE_CURVE('',#4325,#4332,#2581,.T.);
#5539=EDGE_CURVE('',#4333,#4324,#2582,.T.);
#5540=EDGE_CURVE('',#4493,#4494,#3592,.T.);
#5541=EDGE_CURVE('',#4493,#4495,#3593,.T.);
#5542=EDGE_CURVE('',#4496,#4495,#3594,.T.);
#5543=EDGE_CURVE('',#4497,#4496,#3595,.T.);
#5544=EDGE_CURVE('',#4497,#4498,#3596,.T.);
#5545=EDGE_CURVE('',#4499,#4498,#3597,.T.);
#5546=EDGE_CURVE('',#4499,#4500,#2583,.T.);
#5547=EDGE_CURVE('',#4501,#4500,#3598,.T.);
#5548=EDGE_CURVE('',#4501,#4502,#3599,.T.);
#5549=EDGE_CURVE('',#4503,#4502,#427,.T.);
#5550=EDGE_CURVE('',#4503,#4504,#2584,.T.);
#5551=EDGE_CURVE('',#4504,#4505,#3600,.T.);
#5552=EDGE_CURVE('',#4505,#4506,#2585,.T.);
#5553=EDGE_CURVE('',#4507,#4506,#428,.T.);
#5554=EDGE_CURVE('',#4507,#4508,#3601,.T.);
#5555=EDGE_CURVE('',#4509,#4508,#429,.T.);
#5556=EDGE_CURVE('',#4509,#4510,#2586,.T.);
#5557=EDGE_CURVE('',#4510,#4433,#3602,.T.);
#5558=EDGE_CURVE('',#4432,#4511,#430,.T.);
#5559=EDGE_CURVE('',#4511,#4512,#3603,.T.);
#5560=EDGE_CURVE('',#4513,#4512,#3604,.T.);
#5561=EDGE_CURVE('',#4514,#4513,#3605,.T.);
#5562=EDGE_CURVE('',#4514,#4515,#3606,.T.);
#5563=EDGE_CURVE('',#4516,#4515,#431,.T.);
#5564=EDGE_CURVE('',#4516,#4517,#2587,.T.);
#5565=EDGE_CURVE('',#4517,#4437,#3607,.T.);
#5566=EDGE_CURVE('',#4518,#4435,#432,.T.);
#5567=EDGE_CURVE('',#4518,#4519,#3608,.T.);
#5568=EDGE_CURVE('',#4520,#4519,#433,.T.);
#5569=EDGE_CURVE('',#4520,#4521,#2588,.T.);
#5570=EDGE_CURVE('',#4521,#4522,#3609,.T.);
#5571=EDGE_CURVE('',#4522,#4523,#2589,.T.);
#5572=EDGE_CURVE('',#4523,#4524,#434,.T.);
#5573=EDGE_CURVE('',#4524,#4525,#3610,.T.);
#5574=EDGE_CURVE('',#4526,#4525,#3611,.T.);
#5575=EDGE_CURVE('',#4527,#4526,#3612,.T.);
#5576=EDGE_CURVE('',#4527,#4528,#3613,.T.);
#5577=EDGE_CURVE('',#4529,#4528,#435,.T.);
#5578=EDGE_CURVE('',#4529,#4530,#2590,.T.);
#5579=EDGE_CURVE('',#4530,#4531,#3614,.T.);
#5580=EDGE_CURVE('',#4531,#4532,#2591,.T.);
#5581=EDGE_CURVE('',#4533,#4532,#436,.T.);
#5582=EDGE_CURVE('',#4533,#4534,#3615,.T.);
#5583=EDGE_CURVE('',#4444,#4534,#437,.T.);
#5584=EDGE_CURVE('',#4446,#4535,#3616,.T.);
#5585=EDGE_CURVE('',#4535,#4536,#2592,.T.);
#5586=EDGE_CURVE('',#4536,#4537,#438,.T.);
#5587=EDGE_CURVE('',#4537,#4538,#3617,.T.);
#5588=EDGE_CURVE('',#4539,#4538,#3618,.T.);
#5589=EDGE_CURVE('',#4540,#4539,#3619,.T.);
#5590=EDGE_CURVE('',#4540,#4541,#3620,.T.);
#5591=EDGE_CURVE('',#4439,#4541,#439,.T.);
#5592=EDGE_CURVE('',#4442,#4542,#3621,.T.);
#5593=EDGE_CURVE('',#4542,#4543,#2593,.T.);
#5594=EDGE_CURVE('',#4544,#4543,#440,.T.);
#5595=EDGE_CURVE('',#4544,#4545,#3622,.T.);
#5596=EDGE_CURVE('',#4546,#4545,#441,.T.);
#5597=EDGE_CURVE('',#4546,#4547,#2594,.T.);
#5598=EDGE_CURVE('',#4547,#4548,#3623,.T.);
#5599=EDGE_CURVE('',#4548,#4549,#2595,.T.);
#5600=EDGE_CURVE('',#4549,#4550,#442,.T.);
#5601=EDGE_CURVE('',#4550,#4551,#3624,.T.);
#5602=EDGE_CURVE('',#4500,#4551,#3625,.T.);
#5603=EDGE_CURVE('',#4552,#4499,#3626,.T.);
#5604=EDGE_CURVE('',#4552,#4553,#3627,.T.);
#5605=EDGE_CURVE('',#4554,#4553,#3628,.T.);
#5606=EDGE_CURVE('',#4555,#4554,#3629,.T.);
#5607=EDGE_CURVE('',#4555,#4556,#3630,.T.);
#5608=EDGE_CURVE('',#4494,#4556,#3631,.T.);
#5609=EDGE_CURVE('',#4309,#4319,#2596,.T.);
#5610=EDGE_CURVE('',#4316,#4314,#2597,.T.);
#5611=EDGE_CURVE('',#4557,#4558,#3632,.T.);
#5612=EDGE_CURVE('',#4558,#4559,#443,.T.);
#5613=EDGE_CURVE('',#4559,#4560,#3633,.T.);
#5614=EDGE_CURVE('',#4560,#4561,#444,.T.);
#5615=EDGE_CURVE('',#4561,#4562,#445,.T.);
#5616=EDGE_CURVE('',#4562,#4563,#3634,.T.);
#5617=EDGE_CURVE('',#4563,#4557,#446,.T.);
#5618=EDGE_CURVE('',#4564,#4565,#3635,.T.);
#5619=EDGE_CURVE('',#4412,#4565,#2598,.T.);
#5620=EDGE_CURVE('',#4564,#4411,#2599,.T.);
#5621=EDGE_CURVE('',#4566,#4567,#3636,.T.);
#5622=EDGE_CURVE('',#4566,#4568,#2600,.T.);
#5623=EDGE_CURVE('',#4568,#4569,#3637,.T.);
#5624=EDGE_CURVE('',#4567,#4569,#2601,.T.);
#5625=EDGE_CURVE('',#4570,#4571,#2602,.T.);
#5626=EDGE_CURVE('',#4572,#4571,#2603,.T.);
#5627=EDGE_CURVE('',#4573,#4572,#2604,.T.);
#5628=EDGE_CURVE('',#4573,#4377,#2605,.T.);
#5629=EDGE_CURVE('',#4378,#4574,#3638,.T.);
#5630=EDGE_CURVE('',#4574,#4575,#3639,.T.);
#5631=EDGE_CURVE('',#4575,#4576,#2606,.T.);
#5632=EDGE_CURVE('',#4576,#4577,#3640,.T.);
#5633=EDGE_CURVE('',#4577,#4578,#3641,.T.);
#5634=EDGE_CURVE('',#4578,#4579,#3642,.T.);
#5635=EDGE_CURVE('',#4579,#4580,#2607,.T.);
#5636=EDGE_CURVE('',#4581,#4580,#2608,.T.);
#5637=EDGE_CURVE('',#4581,#4582,#2609,.T.);
#5638=EDGE_CURVE('',#4582,#4583,#2610,.T.);
#5639=EDGE_CURVE('',#4583,#4584,#3643,.T.);
#5640=EDGE_CURVE('',#4584,#4585,#2611,.T.);
#5641=EDGE_CURVE('',#4585,#4586,#3644,.T.);
#5642=EDGE_CURVE('',#4586,#4587,#2612,.T.);
#5643=EDGE_CURVE('',#4587,#4588,#3645,.T.);
#5644=EDGE_CURVE('',#4588,#4589,#2613,.T.);
#5645=EDGE_CURVE('',#4589,#4570,#3646,.T.);
#5646=EDGE_CURVE('',#4590,#4591,#3647,.T.);
#5647=EDGE_CURVE('',#4591,#4592,#3648,.T.);
#5648=EDGE_CURVE('',#4592,#4593,#2614,.T.);
#5649=EDGE_CURVE('',#4593,#4594,#3649,.T.);
#5650=EDGE_CURVE('',#4594,#4455,#3650,.T.);
#5651=EDGE_CURVE('',#4456,#4595,#2615,.T.);
#5652=EDGE_CURVE('',#4595,#4590,#3651,.T.);
#5653=EDGE_CURVE('',#4357,#4596,#3652,.T.);
#5654=EDGE_CURVE('',#4596,#4597,#3653,.T.);
#5655=EDGE_CURVE('',#4597,#4598,#2616,.T.);
#5656=EDGE_CURVE('',#4598,#4363,#3654,.T.);
#5657=EDGE_CURVE('',#4362,#4599,#3655,.T.);
#5658=EDGE_CURVE('',#4599,#4356,#2617,.T.);
#5659=EDGE_CURVE('',#4600,#4328,#3656,.T.);
#5660=EDGE_CURVE('',#4329,#4601,#2618,.T.);
#5661=EDGE_CURVE('',#4601,#4335,#3657,.T.);
#5662=EDGE_CURVE('',#4334,#4602,#3658,.T.);
#5663=EDGE_CURVE('',#4602,#4603,#2619,.T.);
#5664=EDGE_CURVE('',#4603,#4600,#3659,.T.);
#5665=EDGE_CURVE('',#4604,#4605,#447,.T.);
#5666=EDGE_CURVE('',#4604,#4606,#3660,.T.);
#5667=EDGE_CURVE('',#4607,#4606,#448,.T.);
#5668=EDGE_CURVE('',#4607,#4608,#2620,.T.);
#5669=EDGE_CURVE('',#4609,#4608,#449,.T.);
#5670=EDGE_CURVE('',#4609,#4610,#3661,.T.);
#5671=EDGE_CURVE('',#4611,#4610,#450,.T.);
#5672=EDGE_CURVE('',#4611,#4612,#2621,.T.);
#5673=EDGE_CURVE('',#4613,#4612,#451,.T.);
#5674=EDGE_CURVE('',#4613,#4614,#3662,.T.);
#5675=EDGE_CURVE('',#4615,#4614,#452,.T.);
#5676=EDGE_CURVE('',#4615,#4616,#2622,.T.);
#5677=EDGE_CURVE('',#4617,#4616,#453,.T.);
#5678=EDGE_CURVE('',#4617,#4618,#3663,.T.);
#5679=EDGE_CURVE('',#4619,#4618,#454,.T.);
#5680=EDGE_CURVE('',#4619,#4605,#2623,.T.);
#5681=EDGE_CURVE('',#4620,#4621,#2624,.T.);
#5682=EDGE_CURVE('',#4620,#4622,#2625,.T.);
#5683=EDGE_CURVE('',#4622,#4623,#2626,.T.);
#5684=EDGE_CURVE('',#4623,#4621,#2627,.T.);
#5685=EDGE_CURVE('',#4624,#4625,#2628,.T.);
#5686=EDGE_CURVE('',#4624,#4626,#2629,.T.);
#5687=EDGE_CURVE('',#4626,#4627,#2630,.T.);
#5688=EDGE_CURVE('',#4627,#4625,#2631,.T.);
#5689=EDGE_CURVE('',#4628,#4629,#2632,.T.);
#5690=EDGE_CURVE('',#4630,#4629,#2633,.T.);
#5691=EDGE_CURVE('',#4631,#4630,#2634,.T.);
#5692=EDGE_CURVE('',#4632,#4631,#2635,.T.);
#5693=EDGE_CURVE('',#4633,#4632,#2636,.T.);
#5694=EDGE_CURVE('',#4633,#4634,#2637,.T.);
#5695=EDGE_CURVE('',#4634,#4635,#2638,.T.);
#5696=EDGE_CURVE('',#4635,#4636,#3664,.T.);
#5697=EDGE_CURVE('',#4636,#4637,#2639,.T.);
#5698=EDGE_CURVE('',#4637,#4638,#3665,.T.);
#5699=EDGE_CURVE('',#4638,#4639,#2640,.T.);
#5700=EDGE_CURVE('',#4639,#4640,#3666,.T.);
#5701=EDGE_CURVE('',#4640,#4641,#2641,.T.);
#5702=EDGE_CURVE('',#4641,#4642,#3667,.T.);
#5703=EDGE_CURVE('',#4642,#4643,#2642,.T.);
#5704=EDGE_CURVE('',#4644,#4643,#2643,.T.);
#5705=EDGE_CURVE('',#4645,#4644,#2644,.T.);
#5706=EDGE_CURVE('',#4628,#4645,#2645,.T.);
#5707=EDGE_CURVE('',#4646,#4647,#2646,.T.);
#5708=EDGE_CURVE('',#4646,#4648,#2647,.T.);
#5709=EDGE_CURVE('',#4648,#4649,#3668,.T.);
#5710=EDGE_CURVE('',#4649,#4650,#2648,.T.);
#5711=EDGE_CURVE('',#4650,#4651,#3669,.T.);
#5712=EDGE_CURVE('',#4651,#4405,#2649,.T.);
#5713=EDGE_CURVE('',#4406,#4652,#2650,.T.);
#5714=EDGE_CURVE('',#4652,#4653,#3670,.T.);
#5715=EDGE_CURVE('',#4653,#4654,#2651,.T.);
#5716=EDGE_CURVE('',#4654,#4655,#2652,.T.);
#5717=EDGE_CURVE('',#4656,#4655,#2653,.T.);
#5718=EDGE_CURVE('',#4656,#4657,#2654,.T.);
#5719=EDGE_CURVE('',#4657,#4658,#2655,.T.);
#5720=EDGE_CURVE('',#4659,#4658,#2656,.T.);
#5721=EDGE_CURVE('',#4647,#4659,#2657,.T.);
#5722=EDGE_CURVE('',#4660,#4661,#2658,.T.);
#5723=EDGE_CURVE('',#4660,#4376,#2659,.T.);
#5724=EDGE_CURVE('',#4376,#4379,#2660,.T.);
#5725=EDGE_CURVE('',#4379,#4661,#2661,.T.);
#5726=EDGE_CURVE('',#4646,#4625,#3671,.T.);
#5727=EDGE_CURVE('',#4648,#4627,#3672,.T.);
#5728=EDGE_CURVE('',#4620,#4643,#3673,.T.);
#5729=EDGE_CURVE('',#4622,#4642,#3674,.T.);
#5730=EDGE_CURVE('',#4662,#4663,#2662,.T.);
#5731=EDGE_CURVE('',#4662,#4621,#3675,.T.);
#5732=EDGE_CURVE('',#4663,#4623,#3676,.T.);
#5733=EDGE_CURVE('',#4624,#4571,#3677,.T.);
#5734=EDGE_CURVE('',#4626,#4570,#3678,.T.);
#5735=EDGE_CURVE('',#4573,#4661,#3679,.T.);
#5736=EDGE_CURVE('',#4664,#4660,#3680,.T.);
#5737=EDGE_CURVE('',#4374,#4664,#2663,.T.);
#5738=EDGE_CURVE('',#4665,#4666,#2664,.T.);
#5739=EDGE_CURVE('',#4666,#4667,#2665,.T.);
#5740=EDGE_CURVE('',#4667,#4668,#2666,.T.);
#5741=EDGE_CURVE('',#4668,#4665,#2667,.T.);
#5742=EDGE_CURVE('',#4669,#4667,#3681,.T.);
#5743=EDGE_CURVE('',#4670,#4669,#2668,.T.);
#5744=EDGE_CURVE('',#4668,#4670,#3682,.T.);
#5745=EDGE_CURVE('',#4666,#4671,#3683,.T.);
#5746=EDGE_CURVE('',#4665,#4672,#3684,.T.);
#5747=EDGE_CURVE('',#4671,#4672,#2669,.T.);
#5748=EDGE_CURVE('',#4673,#4674,#2670,.T.);
#5749=EDGE_CURVE('',#4674,#4675,#3685,.T.);
#5750=EDGE_CURVE('',#4675,#4676,#3686,.T.);
#5751=EDGE_CURVE('',#4677,#4676,#2671,.T.);
#5752=EDGE_CURVE('',#4673,#4677,#2672,.T.);
#5753=EDGE_CURVE('',#4678,#4679,#264,.T.);
#5754=EDGE_CURVE('',#4680,#4678,#265,.T.);
#5755=EDGE_CURVE('',#4680,#4681,#455,.T.);
#5756=EDGE_CURVE('',#4681,#4682,#2673,.T.);
#5757=EDGE_CURVE('',#4682,#4679,#456,.T.);
#5758=EDGE_CURVE('',#4683,#4684,#266,.T.);
#5759=EDGE_CURVE('',#4685,#4683,#267,.T.);
#5760=EDGE_CURVE('',#4685,#4686,#457,.T.);
#5761=EDGE_CURVE('',#4686,#4687,#2674,.T.);
#5762=EDGE_CURVE('',#4687,#4684,#458,.T.);
#5763=EDGE_CURVE('',#4688,#4689,#268,.T.);
#5764=EDGE_CURVE('',#4690,#4688,#269,.T.);
#5765=EDGE_CURVE('',#4690,#4691,#459,.T.);
#5766=EDGE_CURVE('',#4691,#4692,#2675,.T.);
#5767=EDGE_CURVE('',#4692,#4689,#460,.T.);
#5768=EDGE_CURVE('',#4693,#4694,#270,.T.);
#5769=EDGE_CURVE('',#4695,#4693,#271,.T.);
#5770=EDGE_CURVE('',#4695,#4696,#461,.T.);
#5771=EDGE_CURVE('',#4696,#4697,#2676,.T.);
#5772=EDGE_CURVE('',#4697,#4694,#462,.T.);
#5773=EDGE_CURVE('',#4698,#4699,#3687,.T.);
#5774=EDGE_CURVE('',#4699,#4700,#463,.T.);
#5775=EDGE_CURVE('',#4700,#4701,#272,.T.);
#5776=EDGE_CURVE('',#4701,#4702,#3688,.T.);
#5777=EDGE_CURVE('',#4702,#4703,#464,.T.);
#5778=EDGE_CURVE('',#4703,#4704,#3689,.T.);
#5779=EDGE_CURVE('',#4704,#4698,#3690,.T.);
#5780=EDGE_CURVE('',#4705,#4706,#2677,.T.);
#5781=EDGE_CURVE('',#4671,#4705,#2678,.T.);
#5782=EDGE_CURVE('',#4672,#4707,#3691,.T.);
#5783=EDGE_CURVE('',#4707,#4708,#3692,.T.);
#5784=EDGE_CURVE('',#4708,#4709,#2679,.T.);
#5785=EDGE_CURVE('',#4709,#4710,#3693,.T.);
#5786=EDGE_CURVE('',#4710,#4711,#2680,.T.);
#5787=EDGE_CURVE('',#4711,#4712,#3694,.T.);
#5788=EDGE_CURVE('',#4712,#4713,#3695,.T.);
#5789=EDGE_CURVE('',#4713,#4714,#2681,.T.);
#5790=EDGE_CURVE('',#4714,#4715,#3696,.T.);
#5791=EDGE_CURVE('',#4715,#4716,#2682,.T.);
#5792=EDGE_CURVE('',#4716,#4717,#3697,.T.);
#5793=EDGE_CURVE('',#4717,#4718,#3698,.T.);
#5794=EDGE_CURVE('',#4718,#4719,#2683,.T.);
#5795=EDGE_CURVE('',#4719,#4720,#3699,.T.);
#5796=EDGE_CURVE('',#4720,#4430,#2684,.T.);
#5797=EDGE_CURVE('',#4429,#4721,#3700,.T.);
#5798=EDGE_CURVE('',#4721,#4722,#2685,.T.);
#5799=EDGE_CURVE('',#4722,#4723,#3701,.T.);
#5800=EDGE_CURVE('',#4723,#4724,#2686,.T.);
#5801=EDGE_CURVE('',#4569,#4724,#2687,.T.);
#5802=EDGE_CURVE('',#4568,#4725,#2688,.T.);
#5803=EDGE_CURVE('',#4726,#4725,#3702,.T.);
#5804=EDGE_CURVE('',#4726,#4706,#3703,.T.);
#5805=EDGE_CURVE('',#4727,#4728,#2689,.T.);
#5806=EDGE_CURVE('',#4728,#4436,#2690,.T.);
#5807=EDGE_CURVE('',#4729,#4438,#465,.T.);
#5808=EDGE_CURVE('',#4729,#4730,#2691,.T.);
#5809=EDGE_CURVE('',#4730,#4731,#3704,.T.);
#5810=EDGE_CURVE('',#4731,#4727,#2692,.T.);
#5811=EDGE_CURVE('',#4732,#4733,#2693,.T.);
#5812=EDGE_CURVE('',#4733,#4734,#2694,.T.);
#5813=EDGE_CURVE('',#4734,#4735,#2695,.T.);
#5814=EDGE_CURVE('',#4735,#4736,#2696,.T.);
#5815=EDGE_CURVE('',#4736,#4737,#3705,.T.);
#5816=EDGE_CURVE('',#4737,#4738,#2697,.T.);
#5817=EDGE_CURVE('',#4732,#4738,#466,.T.);
#5818=EDGE_CURVE('',#4739,#4740,#3706,.T.);
#5819=EDGE_CURVE('',#4740,#4741,#467,.T.);
#5820=EDGE_CURVE('',#4742,#4741,#468,.T.);
#5821=EDGE_CURVE('',#4742,#4743,#3707,.T.);
#5822=EDGE_CURVE('',#4743,#4744,#3708,.T.);
#5823=EDGE_CURVE('',#4744,#4745,#3709,.T.);
#5824=EDGE_CURVE('',#4745,#4739,#469,.T.);
#5825=EDGE_CURVE('',#4746,#4747,#470,.T.);
#5826=EDGE_CURVE('',#4747,#4748,#3710,.T.);
#5827=EDGE_CURVE('',#4748,#4749,#471,.T.);
#5828=EDGE_CURVE('',#4749,#4750,#3711,.T.);
#5829=EDGE_CURVE('',#4750,#4751,#472,.T.);
#5830=EDGE_CURVE('',#4751,#4746,#3712,.T.);
#5831=EDGE_CURVE('',#4752,#4753,#2698,.T.);
#5832=EDGE_CURVE('',#4753,#4754,#3713,.T.);
#5833=EDGE_CURVE('',#4754,#4755,#2699,.T.);
#5834=EDGE_CURVE('',#4755,#4752,#3714,.T.);
#5835=EDGE_CURVE('',#4420,#4423,#3715,.T.);
#5836=EDGE_CURVE('',#4421,#4418,#3716,.T.);
#5837=EDGE_CURVE('',#4756,#4757,#2700,.T.);
#5838=EDGE_CURVE('',#4757,#4758,#3717,.T.);
#5839=EDGE_CURVE('',#4758,#4759,#2701,.T.);
#5840=EDGE_CURVE('',#4759,#4760,#3718,.T.);
#5841=EDGE_CURVE('',#4760,#4761,#473,.T.);
#5842=EDGE_CURVE('',#4761,#4756,#3719,.T.);
#5843=EDGE_CURVE('',#4762,#4763,#2702,.T.);
#5844=EDGE_CURVE('',#4763,#4764,#3720,.T.);
#5845=EDGE_CURVE('',#4764,#4765,#2703,.T.);
#5846=EDGE_CURVE('',#4765,#4766,#3721,.T.);
#5847=EDGE_CURVE('',#4766,#4767,#474,.T.);
#5848=EDGE_CURVE('',#4767,#4762,#3722,.T.);
#5849=EDGE_CURVE('',#4768,#4769,#2704,.T.);
#5850=EDGE_CURVE('',#4769,#4770,#3723,.T.);
#5851=EDGE_CURVE('',#4770,#4771,#2705,.T.);
#5852=EDGE_CURVE('',#4771,#4772,#3724,.T.);
#5853=EDGE_CURVE('',#4772,#4409,#2706,.T.);
#5854=EDGE_CURVE('',#4410,#4773,#2707,.T.);
#5855=EDGE_CURVE('',#4773,#4768,#3725,.T.);
#5856=EDGE_CURVE('',#4774,#4775,#2708,.T.);
#5857=EDGE_CURVE('',#4775,#4776,#3726,.T.);
#5858=EDGE_CURVE('',#4776,#4777,#2709,.T.);
#5859=EDGE_CURVE('',#4777,#4778,#3727,.T.);
#5860=EDGE_CURVE('',#4778,#4779,#2710,.T.);
#5861=EDGE_CURVE('',#4779,#4780,#3728,.T.);
#5862=EDGE_CURVE('',#4780,#4781,#2711,.T.);
#5863=EDGE_CURVE('',#4781,#4774,#3729,.T.);
#5864=EDGE_CURVE('',#4782,#4783,#475,.T.);
#5865=EDGE_CURVE('',#4782,#4784,#2712,.T.);
#5866=EDGE_CURVE('',#4784,#4785,#2713,.T.);
#5867=EDGE_CURVE('',#4785,#4786,#2714,.T.);
#5868=EDGE_CURVE('',#4787,#4786,#2715,.T.);
#5869=EDGE_CURVE('',#4787,#4788,#2716,.T.);
#5870=EDGE_CURVE('',#4789,#4788,#476,.T.);
#5871=EDGE_CURVE('',#4789,#4783,#477,.T.);
#5872=EDGE_CURVE('',#4790,#4791,#2717,.T.);
#5873=EDGE_CURVE('',#4790,#4792,#2718,.T.);
#5874=EDGE_CURVE('',#4793,#4792,#478,.T.);
#5875=EDGE_CURVE('',#4793,#4794,#479,.T.);
#5876=EDGE_CURVE('',#4795,#4794,#480,.T.);
#5877=EDGE_CURVE('',#4795,#4796,#2719,.T.);
#5878=EDGE_CURVE('',#4796,#4797,#2720,.T.);
#5879=EDGE_CURVE('',#4797,#4791,#2721,.T.);
#5880=EDGE_CURVE('',#4796,#4787,#3730,.T.);
#5881=EDGE_CURVE('',#4786,#4797,#3731,.T.);
#5882=EDGE_CURVE('',#4798,#4799,#2722,.T.);
#5883=EDGE_CURVE('',#4799,#4800,#2723,.T.);
#5884=EDGE_CURVE('',#4801,#4800,#481,.T.);
#5885=EDGE_CURVE('',#4801,#4802,#482,.T.);
#5886=EDGE_CURVE('',#4803,#4802,#483,.T.);
#5887=EDGE_CURVE('',#4803,#4804,#2724,.T.);
#5888=EDGE_CURVE('',#4805,#4804,#2725,.T.);
#5889=EDGE_CURVE('',#4805,#4798,#2726,.T.);
#5890=EDGE_CURVE('',#4806,#4807,#484,.T.);
#5891=EDGE_CURVE('',#4806,#4808,#2727,.T.);
#5892=EDGE_CURVE('',#4809,#4808,#2728,.T.);
#5893=EDGE_CURVE('',#4809,#4810,#2729,.T.);
#5894=EDGE_CURVE('',#4810,#4811,#2730,.T.);
#5895=EDGE_CURVE('',#4811,#4812,#2731,.T.);
#5896=EDGE_CURVE('',#4813,#4812,#485,.T.);
#5897=EDGE_CURVE('',#4813,#4807,#486,.T.);
#5898=EDGE_CURVE('',#4814,#4815,#2732,.T.);
#5899=EDGE_CURVE('',#4816,#4815,#2733,.T.);
#5900=EDGE_CURVE('',#4817,#4816,#2734,.T.);
#5901=EDGE_CURVE('',#4818,#4817,#2735,.T.);
#5902=EDGE_CURVE('',#4818,#4819,#2736,.T.);
#5903=EDGE_CURVE('',#4819,#4820,#2737,.T.);
#5904=EDGE_CURVE('',#4821,#4820,#487,.T.);
#5905=EDGE_CURVE('',#4821,#4822,#3732,.T.);
#5906=EDGE_CURVE('',#4823,#4822,#488,.T.);
#5907=EDGE_CURVE('',#4823,#4824,#2738,.T.);
#5908=EDGE_CURVE('',#4825,#4824,#489,.T.);
#5909=EDGE_CURVE('',#4825,#4826,#3733,.T.);
#5910=EDGE_CURVE('',#4826,#4827,#490,.T.);
#5911=EDGE_CURVE('',#4827,#4828,#2739,.T.);
#5912=EDGE_CURVE('',#4828,#4829,#3734,.T.);
#5913=EDGE_CURVE('',#4829,#4670,#3735,.T.);
#5914=EDGE_CURVE('',#4669,#4830,#2740,.T.);
#5915=EDGE_CURVE('',#4830,#4831,#2741,.T.);
#5916=EDGE_CURVE('',#4832,#4831,#2742,.T.);
#5917=EDGE_CURVE('',#4832,#4833,#2743,.T.);
#5918=EDGE_CURVE('',#4833,#4834,#2744,.T.);
#5919=EDGE_CURVE('',#4834,#4662,#2745,.T.);
#5920=EDGE_CURVE('',#4663,#4835,#3736,.T.);
#5921=EDGE_CURVE('',#4835,#4836,#2746,.T.);
#5922=EDGE_CURVE('',#4836,#4837,#3737,.T.);
#5923=EDGE_CURVE('',#4837,#4838,#2747,.T.);
#5924=EDGE_CURVE('',#4838,#4839,#3738,.T.);
#5925=EDGE_CURVE('',#4839,#4840,#2748,.T.);
#5926=EDGE_CURVE('',#4840,#4814,#3739,.T.);
#5927=EDGE_CURVE('',#4841,#4842,#3740,.T.);
#5928=EDGE_CURVE('',#4842,#4843,#491,.T.);
#5929=EDGE_CURVE('',#4843,#4844,#2749,.T.);
#5930=EDGE_CURVE('',#4844,#4845,#3741,.T.);
#5931=EDGE_CURVE('',#4845,#4846,#3742,.T.);
#5932=EDGE_CURVE('',#4846,#4847,#2750,.T.);
#5933=EDGE_CURVE('',#4848,#4847,#492,.T.);
#5934=EDGE_CURVE('',#4848,#4849,#3743,.T.);
#5935=EDGE_CURVE('',#4850,#4849,#493,.T.);
#5936=EDGE_CURVE('',#4850,#4851,#2751,.T.);
#5937=EDGE_CURVE('',#4841,#4851,#494,.T.);
#5938=EDGE_CURVE('',#4852,#4853,#3744,.T.);
#5939=EDGE_CURVE('',#4853,#4854,#495,.T.);
#5940=EDGE_CURVE('',#4854,#4855,#2752,.T.);
#5941=EDGE_CURVE('',#4855,#4450,#3745,.T.);
#5942=EDGE_CURVE('',#4449,#4856,#2753,.T.);
#5943=EDGE_CURVE('',#4857,#4856,#496,.T.);
#5944=EDGE_CURVE('',#4857,#4858,#3746,.T.);
#5945=EDGE_CURVE('',#4859,#4858,#497,.T.);
#5946=EDGE_CURVE('',#4859,#4860,#2754,.T.);
#5947=EDGE_CURVE('',#4852,#4860,#498,.T.);
#5948=EDGE_CURVE('',#4861,#4862,#3747,.T.);
#5949=EDGE_CURVE('',#4862,#4863,#3748,.T.);
#5950=EDGE_CURVE('',#4863,#4864,#2755,.T.);
#5951=EDGE_CURVE('',#4865,#4864,#499,.T.);
#5952=EDGE_CURVE('',#4865,#4866,#3749,.T.);
#5953=EDGE_CURVE('',#4867,#4866,#500,.T.);
#5954=EDGE_CURVE('',#4867,#4868,#2756,.T.);
#5955=EDGE_CURVE('',#4869,#4868,#501,.T.);
#5956=EDGE_CURVE('',#4869,#4870,#3750,.T.);
#5957=EDGE_CURVE('',#4870,#4871,#502,.T.);
#5958=EDGE_CURVE('',#4871,#4861,#2757,.T.);
#5959=EDGE_CURVE('',#4804,#4811,#3751,.T.);
#5960=EDGE_CURVE('',#4810,#4805,#3752,.T.);
#5961=EDGE_CURVE('',#4872,#4873,#503,.T.);
#5962=EDGE_CURVE('',#4873,#4874,#3753,.T.);
#5963=EDGE_CURVE('',#4874,#4875,#504,.T.);
#5964=EDGE_CURVE('',#4875,#4872,#3754,.T.);
#5965=EDGE_CURVE('',#4876,#4877,#273,.T.);
#5966=EDGE_CURVE('',#4876,#4878,#505,.T.);
#5967=EDGE_CURVE('',#4878,#4879,#2758,.T.);
#5968=EDGE_CURVE('',#4879,#4880,#506,.T.);
#5969=EDGE_CURVE('',#4877,#4880,#274,.T.);
#5970=EDGE_CURVE('',#4881,#4882,#275,.T.);
#5971=EDGE_CURVE('',#4881,#4883,#507,.T.);
#5972=EDGE_CURVE('',#4883,#4884,#2759,.T.);
#5973=EDGE_CURVE('',#4884,#4885,#508,.T.);
#5974=EDGE_CURVE('',#4882,#4885,#276,.T.);
#5975=EDGE_CURVE('',#4417,#4886,#509,.T.);
#5976=EDGE_CURVE('',#4886,#4412,#2760,.T.);
#5977=EDGE_CURVE('',#4565,#4887,#2761,.T.);
#5978=EDGE_CURVE('',#4887,#4419,#2762,.T.);
#5979=EDGE_CURVE('',#4411,#4888,#2763,.T.);
#5980=EDGE_CURVE('',#4888,#4889,#510,.T.);
#5981=EDGE_CURVE('',#4889,#4890,#2764,.T.);
#5982=EDGE_CURVE('',#4890,#4891,#2765,.T.);
#5983=EDGE_CURVE('',#4891,#4564,#2766,.T.);
#5984=EDGE_CURVE('',#4892,#4893,#2767,.T.);
#5985=EDGE_CURVE('',#4893,#4894,#3755,.T.);
#5986=EDGE_CURVE('',#4895,#4894,#2768,.T.);
#5987=EDGE_CURVE('',#4895,#4892,#3756,.T.);
#5988=EDGE_CURVE('',#4896,#4897,#2769,.T.);
#5989=EDGE_CURVE('',#4897,#4898,#3757,.T.);
#5990=EDGE_CURVE('',#4898,#4899,#2770,.T.);
#5991=EDGE_CURVE('',#4899,#4896,#3758,.T.);
#5992=EDGE_CURVE('',#4900,#4901,#2771,.T.);
#5993=EDGE_CURVE('',#4901,#4902,#511,.T.);
#5994=EDGE_CURVE('',#4902,#4900,#2772,.T.);
#5995=EDGE_CURVE('',#4903,#4904,#2773,.T.);
#5996=EDGE_CURVE('',#4904,#4905,#3759,.T.);
#5997=EDGE_CURVE('',#4905,#4906,#2774,.T.);
#5998=EDGE_CURVE('',#4906,#4903,#3760,.T.);
#5999=EDGE_CURVE('',#4907,#4908,#2775,.T.);
#6000=EDGE_CURVE('',#4908,#4909,#512,.T.);
#6001=EDGE_CURVE('',#4909,#4907,#2776,.T.);
#6002=EDGE_CURVE('',#4330,#4910,#3761,.T.);
#6003=EDGE_CURVE('',#4910,#4911,#2777,.T.);
#6004=EDGE_CURVE('',#4911,#4323,#3762,.T.);
#6005=EDGE_CURVE('',#4912,#4913,#2778,.T.);
#6006=EDGE_CURVE('',#4913,#4331,#2779,.T.);
#6007=EDGE_CURVE('',#4322,#4912,#2780,.T.);
#6008=EDGE_CURVE('',#4914,#4915,#2781,.T.);
#6009=EDGE_CURVE('',#4915,#4916,#2782,.T.);
#6010=EDGE_CURVE('',#4916,#4917,#2783,.T.);
#6011=EDGE_CURVE('',#4917,#4914,#2784,.T.);
#6012=EDGE_CURVE('',#4326,#4918,#3763,.T.);
#6013=EDGE_CURVE('',#4918,#4320,#2785,.T.);
#6014=EDGE_CURVE('',#4321,#4919,#3764,.T.);
#6015=EDGE_CURVE('',#4919,#4920,#3765,.T.);
#6016=EDGE_CURVE('',#4920,#4921,#2786,.T.);
#6017=EDGE_CURVE('',#4921,#4327,#3766,.T.);
#6018=EDGE_CURVE('',#4914,#4911,#3767,.T.);
#6019=EDGE_CURVE('',#4910,#4915,#3768,.T.);
#6020=EDGE_CURVE('',#4912,#4324,#3769,.T.);
#6021=EDGE_CURVE('',#4333,#4913,#3770,.T.);
#6022=EDGE_CURVE('',#4325,#4917,#3771,.T.);
#6023=EDGE_CURVE('',#4916,#4332,#3772,.T.);
#6024=EDGE_CURVE('',#4922,#4923,#3773,.T.);
#6025=EDGE_CURVE('',#4923,#4924,#513,.T.);
#6026=EDGE_CURVE('',#4924,#4925,#277,.T.);
#6027=EDGE_CURVE('',#4925,#4926,#3774,.T.);
#6028=EDGE_CURVE('',#4926,#4927,#514,.T.);
#6029=EDGE_CURVE('',#4927,#4928,#3775,.T.);
#6030=EDGE_CURVE('',#4928,#4922,#3776,.T.);
#6031=EDGE_CURVE('',#4447,#4929,#2787,.T.);
#6032=EDGE_CURVE('',#4929,#4930,#2788,.T.);
#6033=EDGE_CURVE('',#4930,#4931,#2789,.T.);
#6034=EDGE_CURVE('',#4932,#4931,#515,.T.);
#6035=EDGE_CURVE('',#4932,#4933,#2790,.T.);
#6036=EDGE_CURVE('',#4933,#4934,#3777,.T.);
#6037=EDGE_CURVE('',#4934,#4447,#2791,.T.);
#6038=EDGE_CURVE('',#4443,#4935,#2792,.T.);
#6039=EDGE_CURVE('',#4935,#4936,#2793,.T.);
#6040=EDGE_CURVE('',#4936,#4937,#2794,.T.);
#6041=EDGE_CURVE('',#4937,#4938,#3778,.T.);
#6042=EDGE_CURVE('',#4938,#4939,#2795,.T.);
#6043=EDGE_CURVE('',#4445,#4939,#516,.T.);
#6044=EDGE_CURVE('',#4940,#4941,#3779,.T.);
#6045=EDGE_CURVE('',#4941,#4942,#517,.T.);
#6046=EDGE_CURVE('',#4943,#4942,#518,.T.);
#6047=EDGE_CURVE('',#4943,#4944,#3780,.T.);
#6048=EDGE_CURVE('',#4944,#4945,#3781,.T.);
#6049=EDGE_CURVE('',#4945,#4946,#3782,.T.);
#6050=EDGE_CURVE('',#4946,#4940,#519,.T.);
#6051=EDGE_CURVE('',#4947,#4948,#2796,.T.);
#6052=EDGE_CURVE('',#4948,#4949,#3783,.T.);
#6053=EDGE_CURVE('',#4949,#4950,#2797,.T.);
#6054=EDGE_CURVE('',#4950,#4947,#3784,.T.);
#6055=EDGE_CURVE('',#4951,#4952,#2798,.T.);
#6056=EDGE_CURVE('',#4952,#4953,#3785,.T.);
#6057=EDGE_CURVE('',#4953,#4954,#2799,.T.);
#6058=EDGE_CURVE('',#4954,#4955,#3786,.T.);
#6059=EDGE_CURVE('',#4955,#4956,#520,.T.);
#6060=EDGE_CURVE('',#4956,#4951,#3787,.T.);
#6061=EDGE_CURVE('',#4957,#4958,#2800,.T.);
#6062=EDGE_CURVE('',#4958,#4959,#3788,.T.);
#6063=EDGE_CURVE('',#4959,#4960,#2801,.T.);
#6064=EDGE_CURVE('',#4960,#4961,#3789,.T.);
#6065=EDGE_CURVE('',#4961,#4413,#2802,.T.);
#6066=EDGE_CURVE('',#4414,#4962,#2803,.T.);
#6067=EDGE_CURVE('',#4962,#4957,#3790,.T.);
#6068=EDGE_CURVE('',#4963,#4964,#2804,.T.);
#6069=EDGE_CURVE('',#4964,#4965,#3791,.T.);
#6070=EDGE_CURVE('',#4965,#4966,#2805,.T.);
#6071=EDGE_CURVE('',#4966,#4967,#3792,.T.);
#6072=EDGE_CURVE('',#4967,#4968,#2806,.T.);
#6073=EDGE_CURVE('',#4968,#4969,#3793,.T.);
#6074=EDGE_CURVE('',#4969,#4970,#2807,.T.);
#6075=EDGE_CURVE('',#4970,#4963,#3794,.T.);
#6076=EDGE_CURVE('',#4971,#4972,#2808,.T.);
#6077=EDGE_CURVE('',#4972,#4973,#2809,.T.);
#6078=EDGE_CURVE('',#4973,#4974,#2810,.T.);
#6079=EDGE_CURVE('',#4975,#4974,#2811,.T.);
#6080=EDGE_CURVE('',#4975,#4976,#2812,.T.);
#6081=EDGE_CURVE('',#4977,#4976,#521,.T.);
#6082=EDGE_CURVE('',#4977,#4978,#522,.T.);
#6083=EDGE_CURVE('',#4971,#4978,#523,.T.);
#6084=EDGE_CURVE('',#4784,#4975,#3795,.T.);
#6085=EDGE_CURVE('',#4974,#4785,#3796,.T.);
#6086=EDGE_CURVE('',#4979,#4980,#2813,.T.);
#6087=EDGE_CURVE('',#4980,#4981,#2814,.T.);
#6088=EDGE_CURVE('',#4981,#4982,#2815,.T.);
#6089=EDGE_CURVE('',#4983,#4982,#524,.T.);
#6090=EDGE_CURVE('',#4983,#4984,#525,.T.);
#6091=EDGE_CURVE('',#4985,#4984,#526,.T.);
#6092=EDGE_CURVE('',#4985,#4986,#2816,.T.);
#6093=EDGE_CURVE('',#4979,#4986,#2817,.T.);
#6094=EDGE_CURVE('',#4986,#4799,#3797,.T.);
#6095=EDGE_CURVE('',#4798,#4979,#3798,.T.);
#6096=EDGE_CURVE('',#4987,#4988,#527,.T.);
#6097=EDGE_CURVE('',#4988,#4989,#3799,.T.);
#6098=EDGE_CURVE('',#4989,#4990,#528,.T.);
#6099=EDGE_CURVE('',#4990,#4987,#3800,.T.);
#6100=EDGE_CURVE('',#4991,#4992,#278,.T.);
#6101=EDGE_CURVE('',#4991,#4993,#529,.T.);
#6102=EDGE_CURVE('',#4993,#4994,#2818,.T.);
#6103=EDGE_CURVE('',#4994,#4995,#530,.T.);
#6104=EDGE_CURVE('',#4992,#4995,#279,.T.);
#6105=EDGE_CURVE('',#4996,#4997,#531,.T.);
#6106=EDGE_CURVE('',#4997,#4416,#2819,.T.);
#6107=EDGE_CURVE('',#4492,#4998,#2820,.T.);
#6108=EDGE_CURVE('',#4998,#4999,#2821,.T.);
#6109=EDGE_CURVE('',#4999,#4996,#2822,.T.);
#6110=EDGE_CURVE('',#4415,#5000,#2823,.T.);
#6111=EDGE_CURVE('',#5000,#4422,#532,.T.);
#6112=EDGE_CURVE('',#4424,#5001,#2824,.T.);
#6113=EDGE_CURVE('',#5001,#4491,#2825,.T.);
#6114=EDGE_CURVE('',#5002,#4448,#2826,.T.);
#6115=EDGE_CURVE('',#4448,#4735,#3801,.T.);
#6116=EDGE_CURVE('',#4734,#5002,#3802,.T.);
#6117=EDGE_CURVE('',#5003,#5004,#2827,.T.);
#6118=EDGE_CURVE('',#5004,#5005,#3803,.T.);
#6119=EDGE_CURVE('',#5005,#5006,#2828,.T.);
#6120=EDGE_CURVE('',#5006,#5003,#3804,.T.);
#6121=EDGE_CURVE('',#5007,#5008,#2829,.T.);
#6122=EDGE_CURVE('',#5008,#5009,#533,.T.);
#6123=EDGE_CURVE('',#5009,#5007,#2830,.T.);
#6124=EDGE_CURVE('',#5010,#5011,#2831,.T.);
#6125=EDGE_CURVE('',#5011,#5012,#3805,.T.);
#6126=EDGE_CURVE('',#5012,#5013,#2832,.T.);
#6127=EDGE_CURVE('',#5013,#5010,#3806,.T.);
#6128=EDGE_CURVE('',#5014,#5015,#2833,.T.);
#6129=EDGE_CURVE('',#5015,#5016,#534,.T.);
#6130=EDGE_CURVE('',#5016,#5014,#2834,.T.);
#6131=EDGE_CURVE('',#4483,#4359,#3807,.T.);
#6132=EDGE_CURVE('',#4359,#4350,#2835,.T.);
#6133=EDGE_CURVE('',#4350,#4480,#3808,.T.);
#6134=EDGE_CURVE('',#5017,#5018,#2836,.T.);
#6135=EDGE_CURVE('',#5018,#4482,#2837,.T.);
#6136=EDGE_CURVE('',#4481,#5017,#2838,.T.);
#6137=EDGE_CURVE('',#4351,#4358,#2839,.T.);
#6138=EDGE_CURVE('',#4358,#5019,#2840,.T.);
#6139=EDGE_CURVE('',#5019,#5020,#2841,.T.);
#6140=EDGE_CURVE('',#5020,#4351,#2842,.T.);
#6141=EDGE_CURVE('',#4354,#5021,#3809,.T.);
#6142=EDGE_CURVE('',#5021,#5022,#2843,.T.);
#6143=EDGE_CURVE('',#5022,#5023,#3810,.T.);
#6144=EDGE_CURVE('',#5023,#4348,#3811,.T.);
#6145=EDGE_CURVE('',#4349,#5024,#2844,.T.);
#6146=EDGE_CURVE('',#5024,#4355,#3812,.T.);
#6147=EDGE_CURVE('',#5017,#4352,#3813,.T.);
#6148=EDGE_CURVE('',#4361,#5018,#3814,.T.);
#6149=EDGE_CURVE('',#4353,#5020,#3815,.T.);
#6150=EDGE_CURVE('',#5019,#4360,#3816,.T.);
#6151=EDGE_CURVE('',#5025,#5026,#3817,.T.);
#6152=EDGE_CURVE('',#5026,#5027,#535,.T.);
#6153=EDGE_CURVE('',#5027,#5028,#280,.T.);
#6154=EDGE_CURVE('',#5028,#5029,#3818,.T.);
#6155=EDGE_CURVE('',#5029,#5030,#536,.T.);
#6156=EDGE_CURVE('',#5030,#5031,#3819,.T.);
#6157=EDGE_CURVE('',#5031,#5025,#3820,.T.);
#6158=EDGE_CURVE('',#5032,#5033,#2845,.T.);
#6159=EDGE_CURVE('',#5033,#5034,#2846,.T.);
#6160=EDGE_CURVE('',#5034,#5035,#2847,.T.);
#6161=EDGE_CURVE('',#5035,#5036,#2848,.T.);
#6162=EDGE_CURVE('',#5037,#5036,#537,.T.);
#6163=EDGE_CURVE('',#5037,#5038,#2849,.T.);
#6164=EDGE_CURVE('',#5038,#5032,#3821,.T.);
#6165=EDGE_CURVE('',#5039,#5040,#2850,.T.);
#6166=EDGE_CURVE('',#5040,#5041,#2851,.T.);
#6167=EDGE_CURVE('',#5041,#5042,#2852,.T.);
#6168=EDGE_CURVE('',#5042,#5043,#2853,.T.);
#6169=EDGE_CURVE('',#5043,#5044,#3822,.T.);
#6170=EDGE_CURVE('',#5044,#5045,#2854,.T.);
#6171=EDGE_CURVE('',#5039,#5045,#538,.T.);
#6172=EDGE_CURVE('',#5046,#5047,#3823,.T.);
#6173=EDGE_CURVE('',#5047,#5048,#539,.T.);
#6174=EDGE_CURVE('',#5049,#5048,#540,.T.);
#6175=EDGE_CURVE('',#5049,#5050,#3824,.T.);
#6176=EDGE_CURVE('',#5050,#5051,#3825,.T.);
#6177=EDGE_CURVE('',#5051,#5052,#3826,.T.);
#6178=EDGE_CURVE('',#5052,#5046,#541,.T.);
#6179=EDGE_CURVE('',#4394,#4400,#2855,.T.);
#6180=EDGE_CURVE('',#4399,#4393,#2856,.T.);
#6181=EDGE_CURVE('',#5053,#4397,#2857,.T.);
#6182=EDGE_CURVE('',#4398,#5054,#2858,.T.);
#6183=EDGE_CURVE('',#5054,#5055,#3827,.T.);
#6184=EDGE_CURVE('',#5055,#5056,#542,.T.);
#6185=EDGE_CURVE('',#5056,#5053,#3828,.T.);
#6186=EDGE_CURVE('',#5057,#5058,#543,.T.);
#6187=EDGE_CURVE('',#5057,#5059,#2859,.T.);
#6188=EDGE_CURVE('',#5059,#5060,#2860,.T.);
#6189=EDGE_CURVE('',#5060,#5061,#2861,.T.);
#6190=EDGE_CURVE('',#5062,#5061,#2862,.T.);
#6191=EDGE_CURVE('',#5062,#5063,#2863,.T.);
#6192=EDGE_CURVE('',#5064,#5063,#544,.T.);
#6193=EDGE_CURVE('',#5064,#5058,#545,.T.);
#6194=EDGE_CURVE('',#4622,#5062,#3829,.T.);
#6195=EDGE_CURVE('',#5061,#4623,#3830,.T.);
#6196=EDGE_CURVE('',#5065,#5066,#2864,.T.);
#6197=EDGE_CURVE('',#5066,#5067,#2865,.T.);
#6198=EDGE_CURVE('',#5068,#5067,#546,.T.);
#6199=EDGE_CURVE('',#5068,#5069,#547,.T.);
#6200=EDGE_CURVE('',#5070,#5069,#548,.T.);
#6201=EDGE_CURVE('',#5070,#5071,#2866,.T.);
#6202=EDGE_CURVE('',#5072,#5071,#2867,.T.);
#6203=EDGE_CURVE('',#5072,#5065,#2868,.T.);
#6204=EDGE_CURVE('',#5071,#4627,#3831,.T.);
#6205=EDGE_CURVE('',#4626,#5072,#3832,.T.);
#6206=EDGE_CURVE('',#5073,#5074,#549,.T.);
#6207=EDGE_CURVE('',#5074,#5075,#3833,.T.);
#6208=EDGE_CURVE('',#5075,#5076,#550,.T.);
#6209=EDGE_CURVE('',#5076,#5073,#3834,.T.);
#6210=EDGE_CURVE('',#5077,#5078,#281,.T.);
#6211=EDGE_CURVE('',#5077,#5079,#551,.T.);
#6212=EDGE_CURVE('',#5079,#5080,#2869,.T.);
#6213=EDGE_CURVE('',#5080,#5081,#552,.T.);
#6214=EDGE_CURVE('',#5078,#5081,#282,.T.);
#6215=EDGE_CURVE('',#5082,#5083,#553,.T.);
#6216=EDGE_CURVE('',#5083,#4478,#2870,.T.);
#6217=EDGE_CURVE('',#4407,#5084,#2871,.T.);
#6218=EDGE_CURVE('',#5084,#5085,#2872,.T.);
#6219=EDGE_CURVE('',#5085,#5082,#2873,.T.);
#6220=EDGE_CURVE('',#4479,#5086,#2874,.T.);
#6221=EDGE_CURVE('',#5086,#5087,#554,.T.);
#6222=EDGE_CURVE('',#5087,#5088,#2875,.T.);
#6223=EDGE_CURVE('',#5088,#5089,#2876,.T.);
#6224=EDGE_CURVE('',#5089,#4408,#2877,.T.);
#6225=EDGE_CURVE('',#5090,#5091,#2878,.T.);
#6226=EDGE_CURVE('',#5091,#4936,#3835,.T.);
#6227=EDGE_CURVE('',#4935,#5090,#3836,.T.);
#6228=EDGE_CURVE('',#5092,#5093,#2879,.T.);
#6229=EDGE_CURVE('',#5093,#5094,#3837,.T.);
#6230=EDGE_CURVE('',#5094,#5095,#2880,.T.);
#6231=EDGE_CURVE('',#5095,#5092,#3838,.T.);
#6232=EDGE_CURVE('',#5096,#5097,#2881,.T.);
#6233=EDGE_CURVE('',#5097,#5098,#555,.T.);
#6234=EDGE_CURVE('',#5098,#5096,#2882,.T.);
#6235=EDGE_CURVE('',#5099,#5100,#2883,.T.);
#6236=EDGE_CURVE('',#5100,#5101,#3839,.T.);
#6237=EDGE_CURVE('',#5101,#5102,#2884,.T.);
#6238=EDGE_CURVE('',#5102,#5099,#3840,.T.);
#6239=EDGE_CURVE('',#4440,#5103,#556,.T.);
#6240=EDGE_CURVE('',#5103,#4441,#2885,.T.);
#6241=EDGE_CURVE('',#4470,#5104,#3841,.T.);
#6242=EDGE_CURVE('',#5104,#5105,#2886,.T.);
#6243=EDGE_CURVE('',#5105,#4467,#3842,.T.);
#6244=EDGE_CURVE('',#4468,#5106,#2887,.T.);
#6245=EDGE_CURVE('',#5106,#5107,#2888,.T.);
#6246=EDGE_CURVE('',#5107,#4469,#2889,.T.);
#6247=EDGE_CURVE('',#5108,#5109,#2890,.T.);
#6248=EDGE_CURVE('',#5109,#5110,#2891,.T.);
#6249=EDGE_CURVE('',#5110,#5111,#2892,.T.);
#6250=EDGE_CURVE('',#5111,#5108,#2893,.T.);
#6251=EDGE_CURVE('',#5112,#5113,#2894,.T.);
#6252=EDGE_CURVE('',#5112,#5114,#2895,.T.);
#6253=EDGE_CURVE('',#5114,#5115,#3843,.T.);
#6254=EDGE_CURVE('',#5115,#5116,#3844,.T.);
#6255=EDGE_CURVE('',#5116,#5117,#3845,.T.);
#6256=EDGE_CURVE('',#5117,#5118,#2896,.T.);
#6257=EDGE_CURVE('',#5118,#5119,#3846,.T.);
#6258=EDGE_CURVE('',#5119,#4373,#3847,.T.);
#6259=EDGE_CURVE('',#4664,#5120,#2897,.T.);
#6260=EDGE_CURVE('',#5113,#5120,#2898,.T.);
#6261=EDGE_CURVE('',#5108,#5105,#3848,.T.);
#6262=EDGE_CURVE('',#5104,#5109,#3849,.T.);
#6263=EDGE_CURVE('',#4471,#5111,#3850,.T.);
#6264=EDGE_CURVE('',#5110,#4472,#3851,.T.);
#6265=EDGE_CURVE('',#5121,#5122,#3852,.T.);
#6266=EDGE_CURVE('',#5122,#5123,#557,.T.);
#6267=EDGE_CURVE('',#5123,#5124,#283,.T.);
#6268=EDGE_CURVE('',#5124,#5125,#3853,.T.);
#6269=EDGE_CURVE('',#5125,#5126,#558,.T.);
#6270=EDGE_CURVE('',#5126,#5127,#3854,.T.);
#6271=EDGE_CURVE('',#5127,#5121,#3855,.T.);
#6272=EDGE_CURVE('',#4426,#5128,#2899,.T.);
#6273=EDGE_CURVE('',#5128,#5129,#2900,.T.);
#6274=EDGE_CURVE('',#5130,#5129,#559,.T.);
#6275=EDGE_CURVE('',#5130,#5131,#2901,.T.);
#6276=EDGE_CURVE('',#5131,#5132,#3856,.T.);
#6277=EDGE_CURVE('',#5132,#4427,#2902,.T.);
#6278=EDGE_CURVE('',#5133,#5134,#2903,.T.);
#6279=EDGE_CURVE('',#5134,#4895,#2904,.T.);
#6280=EDGE_CURVE('',#4894,#5135,#2905,.T.);
#6281=EDGE_CURVE('',#5135,#5136,#3857,.T.);
#6282=EDGE_CURVE('',#5136,#5137,#2906,.T.);
#6283=EDGE_CURVE('',#5133,#5137,#560,.T.);
#6284=EDGE_CURVE('',#5138,#5139,#3858,.T.);
#6285=EDGE_CURVE('',#5139,#5140,#561,.T.);
#6286=EDGE_CURVE('',#5141,#5140,#562,.T.);
#6287=EDGE_CURVE('',#5141,#5142,#3859,.T.);
#6288=EDGE_CURVE('',#5142,#5143,#3860,.T.);
#6289=EDGE_CURVE('',#5143,#5144,#3861,.T.);
#6290=EDGE_CURVE('',#5144,#5138,#563,.T.);
#6291=EDGE_CURVE('',#5145,#5146,#2907,.T.);
#6292=EDGE_CURVE('',#5146,#5147,#3862,.T.);
#6293=EDGE_CURVE('',#5147,#5148,#2908,.T.);
#6294=EDGE_CURVE('',#5148,#5149,#3863,.T.);
#6295=EDGE_CURVE('',#5149,#5150,#2909,.T.);
#6296=EDGE_CURVE('',#5150,#5151,#3864,.T.);
#6297=EDGE_CURVE('',#5151,#5152,#2910,.T.);
#6298=EDGE_CURVE('',#5152,#5145,#3865,.T.);
#6299=EDGE_CURVE('',#5153,#5154,#2911,.T.);
#6300=EDGE_CURVE('',#5154,#5155,#3866,.T.);
#6301=EDGE_CURVE('',#5155,#5156,#2912,.T.);
#6302=EDGE_CURVE('',#5156,#5157,#3867,.T.);
#6303=EDGE_CURVE('',#5157,#4401,#2913,.T.);
#6304=EDGE_CURVE('',#4402,#5158,#2914,.T.);
#6305=EDGE_CURVE('',#5158,#5153,#3868,.T.);
#6306=EDGE_CURVE('',#5059,#4790,#3869,.T.);
#6307=EDGE_CURVE('',#4791,#5060,#3870,.T.);
#6308=EDGE_CURVE('',#4808,#5066,#3871,.T.);
#6309=EDGE_CURVE('',#5065,#4809,#3872,.T.);
#6310=EDGE_CURVE('',#5159,#5160,#564,.T.);
#6311=EDGE_CURVE('',#5160,#5161,#3873,.T.);
#6312=EDGE_CURVE('',#5161,#5162,#565,.T.);
#6313=EDGE_CURVE('',#5162,#5159,#3874,.T.);
#6314=EDGE_CURVE('',#5163,#5164,#566,.T.);
#6315=EDGE_CURVE('',#5164,#4465,#2915,.T.);
#6316=EDGE_CURVE('',#4403,#5165,#2916,.T.);
#6317=EDGE_CURVE('',#5165,#5166,#2917,.T.);
#6318=EDGE_CURVE('',#5166,#5163,#2918,.T.);
#6319=EDGE_CURVE('',#4466,#5167,#2919,.T.);
#6320=EDGE_CURVE('',#5167,#5168,#567,.T.);
#6321=EDGE_CURVE('',#5168,#5169,#2920,.T.);
#6322=EDGE_CURVE('',#5169,#5170,#2921,.T.);
#6323=EDGE_CURVE('',#5170,#4404,#2922,.T.);
#6324=EDGE_CURVE('',#4428,#5042,#3875,.T.);
#6325=EDGE_CURVE('',#5041,#4425,#3876,.T.);
#6326=EDGE_CURVE('',#5171,#5172,#2923,.T.);
#6327=EDGE_CURVE('',#5172,#5173,#3877,.T.);
#6328=EDGE_CURVE('',#5173,#5174,#2924,.T.);
#6329=EDGE_CURVE('',#5174,#5171,#3878,.T.);
#6330=EDGE_CURVE('',#4434,#5175,#2925,.T.);
#6331=EDGE_CURVE('',#5175,#4431,#568,.T.);
#6332=EDGE_CURVE('',#5176,#5177,#2926,.T.);
#6333=EDGE_CURVE('',#5177,#5178,#3879,.T.);
#6334=EDGE_CURVE('',#5178,#5179,#2927,.T.);
#6335=EDGE_CURVE('',#5179,#5176,#3880,.T.);
#6336=EDGE_CURVE('',#5180,#5181,#2928,.T.);
#6337=EDGE_CURVE('',#5181,#5182,#569,.T.);
#6338=EDGE_CURVE('',#5182,#5180,#2929,.T.);
#6339=EDGE_CURVE('',#4462,#5183,#3881,.T.);
#6340=EDGE_CURVE('',#5183,#5184,#2930,.T.);
#6341=EDGE_CURVE('',#5184,#4459,#3882,.T.);
#6342=EDGE_CURVE('',#5185,#5186,#2931,.T.);
#6343=EDGE_CURVE('',#5186,#4461,#2932,.T.);
#6344=EDGE_CURVE('',#4460,#5185,#2933,.T.);
#6345=EDGE_CURVE('',#5187,#5188,#2934,.T.);
#6346=EDGE_CURVE('',#5188,#4458,#2935,.T.);
#6347=EDGE_CURVE('',#4458,#4453,#2936,.T.);
#6348=EDGE_CURVE('',#4453,#5187,#2937,.T.);
#6349=EDGE_CURVE('',#4452,#5189,#3883,.T.);
#6350=EDGE_CURVE('',#5189,#5190,#3884,.T.);
#6351=EDGE_CURVE('',#5190,#5191,#2938,.T.);
#6352=EDGE_CURVE('',#5191,#5192,#3885,.T.);
#6353=EDGE_CURVE('',#5192,#5193,#3886,.T.);
#6354=EDGE_CURVE('',#5193,#5194,#3887,.T.);
#6355=EDGE_CURVE('',#5194,#4451,#2939,.T.);
#6356=EDGE_CURVE('',#5187,#5184,#3888,.T.);
#6357=EDGE_CURVE('',#5183,#5188,#3889,.T.);
#6358=EDGE_CURVE('',#5185,#4463,#3890,.T.);
#6359=EDGE_CURVE('',#4464,#5186,#3891,.T.);
#6360=EDGE_CURVE('',#4464,#4594,#3892,.T.);
#6361=EDGE_CURVE('',#5186,#4593,#3893,.T.);
#6362=EDGE_CURVE('',#4461,#4592,#3894,.T.);
#6363=EDGE_CURVE('',#4595,#5188,#3895,.T.);
#6364=EDGE_CURVE('',#4462,#4591,#3896,.T.);
#6365=EDGE_CURVE('',#4590,#5183,#3897,.T.);
#6366=EDGE_CURVE('',#5189,#4463,#3898,.T.);
#6367=EDGE_CURVE('',#5190,#5185,#3899,.T.);
#6368=EDGE_CURVE('',#5191,#4460,#3900,.T.);
#6369=EDGE_CURVE('',#5187,#5194,#3901,.T.);
#6370=EDGE_CURVE('',#5192,#4459,#3902,.T.);
#6371=EDGE_CURVE('',#5184,#5193,#3903,.T.);
#6372=EDGE_CURVE('',#4500,#5195,#570,.T.);
#6373=EDGE_CURVE('',#4551,#5196,#571,.T.);
#6374=EDGE_CURVE('',#5196,#5195,#572,.T.);
#6375=EDGE_CURVE('',#5196,#5046,#573,.T.);
#6376=EDGE_CURVE('',#5046,#5197,#574,.T.);
#6377=EDGE_CURVE('',#5197,#5195,#575,.T.);
#6378=EDGE_CURVE('',#5197,#4695,#576,.T.);
#6379=EDGE_CURVE('',#4693,#5195,#577,.T.);
#6380=EDGE_CURVE('',#4694,#5198,#578,.T.);
#6381=EDGE_CURVE('',#5198,#5195,#579,.T.);
#6382=EDGE_CURVE('',#5198,#5125,#580,.T.);
#6383=EDGE_CURVE('',#5199,#5125,#581,.T.);
#6384=EDGE_CURVE('',#5199,#5195,#582,.T.);
#6385=EDGE_CURVE('',#5200,#5201,#583,.T.);
#6386=EDGE_CURVE('',#5200,#4881,#584,.T.);
#6387=EDGE_CURVE('',#4882,#5201,#585,.T.);
#6388=EDGE_CURVE('',#4885,#5202,#586,.T.);
#6389=EDGE_CURVE('',#5202,#5201,#587,.T.);
#6390=EDGE_CURVE('',#5202,#4702,#588,.T.);
#6391=EDGE_CURVE('',#4702,#5203,#589,.T.);
#6392=EDGE_CURVE('',#5203,#5201,#590,.T.);
#6393=EDGE_CURVE('',#5203,#4514,#591,.T.);
#6394=EDGE_CURVE('',#4513,#5201,#592,.T.);
#6395=EDGE_CURVE('',#5204,#4512,#3904,.T.);
#6396=EDGE_CURVE('',#5204,#5201,#593,.T.);
#6397=EDGE_CURVE('',#4539,#5205,#594,.T.);
#6398=EDGE_CURVE('',#4538,#5206,#595,.T.);
#6399=EDGE_CURVE('',#5206,#5205,#596,.T.);
#6400=EDGE_CURVE('',#5206,#4940,#597,.T.);
#6401=EDGE_CURVE('',#4940,#5207,#598,.T.);
#6402=EDGE_CURVE('',#5207,#5205,#599,.T.);
#6403=EDGE_CURVE('',#5207,#4685,#600,.T.);
#6404=EDGE_CURVE('',#4683,#5205,#601,.T.);
#6405=EDGE_CURVE('',#4684,#5208,#602,.T.);
#6406=EDGE_CURVE('',#5208,#5205,#603,.T.);
#6407=EDGE_CURVE('',#5208,#5029,#604,.T.);
#6408=EDGE_CURVE('',#5209,#5029,#605,.T.);
#6409=EDGE_CURVE('',#5209,#5205,#606,.T.);
#6410=EDGE_CURVE('',#5210,#5211,#607,.T.);
#6411=EDGE_CURVE('',#5210,#4680,#608,.T.);
#6412=EDGE_CURVE('',#4678,#5211,#609,.T.);
#6413=EDGE_CURVE('',#4679,#5212,#610,.T.);
#6414=EDGE_CURVE('',#5212,#5211,#611,.T.);
#6415=EDGE_CURVE('',#5212,#4926,#612,.T.);
#6416=EDGE_CURVE('',#4926,#5213,#613,.T.);
#6417=EDGE_CURVE('',#5213,#5211,#614,.T.);
#6418=EDGE_CURVE('',#5213,#4527,#615,.T.);
#6419=EDGE_CURVE('',#4526,#5211,#616,.T.);
#6420=EDGE_CURVE('',#5214,#4525,#3905,.T.);
#6421=EDGE_CURVE('',#5214,#5211,#617,.T.);
#6422=EDGE_CURVE('',#4925,#5015,#618,.T.);
#6423=EDGE_CURVE('',#5016,#4924,#3906,.T.);
#6424=EDGE_CURVE('',#5011,#4923,#3907,.T.);
#6425=EDGE_CURVE('',#5016,#5011,#619,.T.);
#6426=EDGE_CURVE('',#4925,#4528,#3908,.T.);
#6427=EDGE_CURVE('',#4529,#5015,#3909,.T.);
#6428=EDGE_CURVE('',#5012,#4922,#3910,.T.);
#6429=EDGE_CURVE('',#5014,#5010,#3911,.T.);
#6430=EDGE_CURVE('',#4530,#5014,#3912,.T.);
#6431=EDGE_CURVE('',#4927,#4682,#620,.T.);
#6432=EDGE_CURVE('',#4681,#4745,#621,.T.);
#6433=EDGE_CURVE('',#4739,#5210,#622,.T.);
#6434=EDGE_CURVE('',#4860,#4681,#3913,.T.);
#6435=EDGE_CURVE('',#4682,#4859,#3914,.T.);
#6436=EDGE_CURVE('',#4927,#4858,#3915,.T.);
#6437=EDGE_CURVE('',#5012,#4933,#3916,.T.);
#6438=EDGE_CURVE('',#4933,#4922,#3917,.T.);
#6439=EDGE_CURVE('',#4943,#5005,#3918,.T.);
#6440=EDGE_CURVE('',#5008,#4942,#3919,.T.);
#6441=EDGE_CURVE('',#5005,#5008,#623,.T.);
#6442=EDGE_CURVE('',#4530,#5010,#3920,.T.);
#6443=EDGE_CURVE('',#4739,#5214,#624,.T.);
#6444=EDGE_CURVE('',#4852,#4745,#3921,.T.);
#6445=EDGE_CURVE('',#4928,#4857,#3922,.T.);
#6446=EDGE_CURVE('',#4934,#4928,#625,.T.);
#6447=EDGE_CURVE('',#5013,#4932,#3923,.T.);
#6448=EDGE_CURVE('',#4531,#5013,#626,.T.);
#6449=EDGE_CURVE('',#5009,#4941,#627,.T.);
#6450=EDGE_CURVE('',#5007,#4535,#3924,.T.);
#6451=EDGE_CURVE('',#4536,#5009,#3925,.T.);
#6452=EDGE_CURVE('',#5006,#5007,#3926,.T.);
#6453=EDGE_CURVE('',#4944,#5004,#3927,.T.);
#6454=EDGE_CURVE('',#4537,#4941,#3928,.T.);
#6455=EDGE_CURVE('',#4740,#4524,#3929,.T.);
#6456=EDGE_CURVE('',#4741,#4901,#3930,.T.);
#6457=EDGE_CURVE('',#4902,#4740,#628,.T.);
#6458=EDGE_CURVE('',#4853,#4744,#3931,.T.);
#6459=EDGE_CURVE('',#4855,#4735,#3932,.T.);
#6460=EDGE_CURVE('',#4736,#4854,#3933,.T.);
#6461=EDGE_CURVE('',#4934,#4856,#3934,.T.);
#6462=EDGE_CURVE('',#4531,#4931,#3935,.T.);
#6463=EDGE_CURVE('',#5006,#4535,#3936,.T.);
#6464=EDGE_CURVE('',#4944,#4938,#3937,.T.);
#6465=EDGE_CURVE('',#4938,#5004,#3938,.T.);
#6466=EDGE_CURVE('',#4825,#4946,#3939,.T.);
#6467=EDGE_CURVE('',#4686,#4824,#3940,.T.);
#6468=EDGE_CURVE('',#4946,#4686,#629,.T.);
#6469=EDGE_CURVE('',#4687,#4823,#3941,.T.);
#6470=EDGE_CURVE('',#5030,#4687,#630,.T.);
#6471=EDGE_CURVE('',#4902,#4523,#3942,.T.);
#6472=EDGE_CURVE('',#4898,#4901,#631,.T.);
#6473=EDGE_CURVE('',#4742,#4898,#3943,.T.);
#6474=EDGE_CURVE('',#4736,#4744,#632,.T.);
#6475=EDGE_CURVE('',#4532,#4930,#3944,.T.);
#6476=EDGE_CURVE('',#5003,#4446,#633,.T.);
#6477=EDGE_CURVE('',#4939,#5003,#3945,.T.);
#6478=EDGE_CURVE('',#4945,#4937,#634,.T.);
#6479=EDGE_CURVE('',#4826,#4945,#3946,.T.);
#6480=EDGE_CURVE('',#5030,#4822,#3947,.T.);
#6481=EDGE_CURVE('',#4540,#5209,#3948,.T.);
#6482=EDGE_CURVE('',#4900,#4522,#3949,.T.);
#6483=EDGE_CURVE('',#4899,#4900,#3950,.T.);
#6484=EDGE_CURVE('',#4743,#4897,#3951,.T.);
#6485=EDGE_CURVE('',#4737,#4743,#3952,.T.);
#6486=EDGE_CURVE('',#4710,#4930,#635,.T.);
#6487=EDGE_CURVE('',#4533,#4710,#3953,.T.);
#6488=EDGE_CURVE('',#4827,#4937,#3954,.T.);
#6489=EDGE_CURVE('',#5031,#4821,#3955,.T.);
#6490=EDGE_CURVE('',#5028,#4440,#636,.T.);
#6491=EDGE_CURVE('',#5103,#5027,#3956,.T.);
#6492=EDGE_CURVE('',#4701,#4908,#637,.T.);
#6493=EDGE_CURVE('',#4909,#4700,#3957,.T.);
#6494=EDGE_CURVE('',#4541,#5028,#3958,.T.);
#6495=EDGE_CURVE('',#4899,#4522,#3959,.T.);
#6496=EDGE_CURVE('',#4737,#4897,#3960,.T.);
#6497=EDGE_CURVE('',#4929,#5002,#3961,.T.);
#6498=EDGE_CURVE('',#4711,#4929,#3962,.T.);
#6499=EDGE_CURVE('',#4534,#4709,#3963,.T.);
#6500=EDGE_CURVE('',#4828,#4936,#3964,.T.);
#6501=EDGE_CURVE('',#5032,#4820,#3965,.T.);
#6502=EDGE_CURVE('',#5031,#5032,#638,.T.);
#6503=EDGE_CURVE('',#5100,#5026,#3966,.T.);
#6504=EDGE_CURVE('',#5103,#5100,#639,.T.);
#6505=EDGE_CURVE('',#4904,#4699,#3967,.T.);
#6506=EDGE_CURVE('',#4909,#4904,#640,.T.);
#6507=EDGE_CURVE('',#4701,#4515,#3968,.T.);
#6508=EDGE_CURVE('',#4516,#4908,#3969,.T.);
#6509=EDGE_CURVE('',#4905,#4698,#3970,.T.);
#6510=EDGE_CURVE('',#4907,#4903,#3971,.T.);
#6511=EDGE_CURVE('',#4517,#4907,#3972,.T.);
#6512=EDGE_CURVE('',#4896,#4521,#641,.T.);
#6513=EDGE_CURVE('',#4738,#4896,#3973,.T.);
#6514=EDGE_CURVE('',#4712,#5002,#3974,.T.);
#6515=EDGE_CURVE('',#4443,#4709,#642,.T.);
#6516=EDGE_CURVE('',#4829,#5091,#3975,.T.);
#6517=EDGE_CURVE('',#5033,#4819,#3976,.T.);
#6518=EDGE_CURVE('',#5025,#5038,#3977,.T.);
#6519=EDGE_CURVE('',#5101,#5025,#3978,.T.);
#6520=EDGE_CURVE('',#4441,#5099,#3979,.T.);
#6521=EDGE_CURVE('',#4703,#4884,#643,.T.);
#6522=EDGE_CURVE('',#4883,#5144,#644,.T.);
#6523=EDGE_CURVE('',#5138,#5200,#645,.T.);
#6524=EDGE_CURVE('',#4868,#4883,#3980,.T.);
#6525=EDGE_CURVE('',#4884,#4867,#3981,.T.);
#6526=EDGE_CURVE('',#4703,#4866,#3982,.T.);
#6527=EDGE_CURVE('',#4905,#4730,#3983,.T.);
#6528=EDGE_CURVE('',#4730,#4698,#3984,.T.);
#6529=EDGE_CURVE('',#4517,#4903,#3985,.T.);
#6530=EDGE_CURVE('',#4732,#4521,#3986,.T.);
#6531=EDGE_CURVE('',#4713,#4734,#3987,.T.);
#6532=EDGE_CURVE('',#4935,#4708,#3988,.T.);
#6533=EDGE_CURVE('',#4668,#5091,#3989,.T.);
#6534=EDGE_CURVE('',#5101,#5038,#3990,.T.);
#6535=EDGE_CURVE('',#4442,#5099,#3991,.T.);
#6536=EDGE_CURVE('',#5138,#5204,#646,.T.);
#6537=EDGE_CURVE('',#4869,#5144,#3992,.T.);
#6538=EDGE_CURVE('',#4704,#4865,#3993,.T.);
#6539=EDGE_CURVE('',#4731,#4704,#647,.T.);
#6540=EDGE_CURVE('',#4906,#4729,#3994,.T.);
#6541=EDGE_CURVE('',#4437,#4906,#648,.T.);
#6542=EDGE_CURVE('',#4733,#4520,#3995,.T.);
#6543=EDGE_CURVE('',#4714,#4733,#649,.T.);
#6544=EDGE_CURVE('',#5090,#4707,#3996,.T.);
#6545=EDGE_CURVE('',#4665,#5090,#3997,.T.);
#6546=EDGE_CURVE('',#5102,#5037,#3998,.T.);
#6547=EDGE_CURVE('',#4542,#5102,#650,.T.);
#6548=EDGE_CURVE('',#5139,#4511,#3999,.T.);
#6549=EDGE_CURVE('',#5140,#5175,#4000,.T.);
#6550=EDGE_CURVE('',#4431,#5139,#651,.T.);
#6551=EDGE_CURVE('',#4870,#5143,#4001,.T.);
#6552=EDGE_CURVE('',#4861,#4894,#4002,.T.);
#6553=EDGE_CURVE('',#5135,#4871,#4003,.T.);
#6554=EDGE_CURVE('',#4731,#4864,#4004,.T.);
#6555=EDGE_CURVE('',#4714,#4519,#4005,.T.);
#6556=EDGE_CURVE('',#4542,#5036,#4006,.T.);
#6557=EDGE_CURVE('',#5173,#5175,#652,.T.);
#6558=EDGE_CURVE('',#5141,#5173,#4007,.T.);
#6559=EDGE_CURVE('',#5135,#5143,#653,.T.);
#6560=EDGE_CURVE('',#4862,#4893,#4008,.T.);
#6561=EDGE_CURVE('',#4727,#4863,#4009,.T.);
#6562=EDGE_CURVE('',#4715,#4518,#4010,.T.);
#6563=EDGE_CURVE('',#4724,#5034,#4011,.T.);
#6564=EDGE_CURVE('',#5035,#4723,#654,.T.);
#6565=EDGE_CURVE('',#4543,#5035,#4012,.T.);
#6566=EDGE_CURVE('',#5174,#4434,#4013,.T.);
#6567=EDGE_CURVE('',#5142,#5172,#4014,.T.);
#6568=EDGE_CURVE('',#5136,#5142,#4015,.T.);
#6569=EDGE_CURVE('',#4727,#4893,#4016,.T.);
#6570=EDGE_CURVE('',#4715,#4436,#655,.T.);
#6571=EDGE_CURVE('',#4544,#4723,#4017,.T.);
#6572=EDGE_CURVE('',#5174,#4433,#4018,.T.);
#6573=EDGE_CURVE('',#5136,#5172,#4019,.T.);
#6574=EDGE_CURVE('',#4728,#4892,#4020,.T.);
#6575=EDGE_CURVE('',#4716,#4728,#4021,.T.);
#6576=EDGE_CURVE('',#4545,#4722,#4022,.T.);
#6577=EDGE_CURVE('',#5040,#4546,#4023,.T.);
#6578=EDGE_CURVE('',#4547,#5039,#4024,.T.);
#6579=EDGE_CURVE('',#5045,#5092,#4025,.T.);
#6580=EDGE_CURVE('',#5093,#5044,#4026,.T.);
#6581=EDGE_CURVE('',#4547,#5092,#656,.T.);
#6582=EDGE_CURVE('',#5171,#4510,#657,.T.);
#6583=EDGE_CURVE('',#5137,#5171,#4027,.T.);
#6584=EDGE_CURVE('',#4717,#4892,#4028,.T.);
#6585=EDGE_CURVE('',#5040,#4722,#658,.T.);
#6586=EDGE_CURVE('',#5050,#5044,#4029,.T.);
#6587=EDGE_CURVE('',#5093,#5050,#4030,.T.);
#6588=EDGE_CURVE('',#5094,#5049,#4031,.T.);
#6589=EDGE_CURVE('',#5095,#5096,#4032,.T.);
#6590=EDGE_CURVE('',#5097,#5094,#659,.T.);
#6591=EDGE_CURVE('',#4548,#5095,#4033,.T.);
#6592=EDGE_CURVE('',#5133,#4510,#4034,.T.);
#6593=EDGE_CURVE('',#4718,#4895,#4035,.T.);
#6594=EDGE_CURVE('',#5041,#4721,#4036,.T.);
#6595=EDGE_CURVE('',#5051,#5043,#660,.T.);
#6596=EDGE_CURVE('',#5097,#5048,#4037,.T.);
#6597=EDGE_CURVE('',#4548,#5096,#4038,.T.);
#6598=EDGE_CURVE('',#5134,#4509,#4039,.T.);
#6599=EDGE_CURVE('',#4719,#5134,#661,.T.);
#6600=EDGE_CURVE('',#4843,#5043,#4040,.T.);
#6601=EDGE_CURVE('',#5051,#4842,#4041,.T.);
#6602=EDGE_CURVE('',#5052,#4841,#4042,.T.);
#6603=EDGE_CURVE('',#5098,#5047,#662,.T.);
#6604=EDGE_CURVE('',#4549,#5098,#4043,.T.);
#6605=EDGE_CURVE('',#4719,#4508,#4044,.T.);
#6606=EDGE_CURVE('',#4844,#5042,#4045,.T.);
#6607=EDGE_CURVE('',#4696,#4851,#4046,.T.);
#6608=EDGE_CURVE('',#5052,#4696,#663,.T.);
#6609=EDGE_CURVE('',#4550,#5047,#4047,.T.);
#6610=EDGE_CURVE('',#4720,#4507,#4048,.T.);
#6611=EDGE_CURVE('',#5128,#4720,#664,.T.);
#6612=EDGE_CURVE('',#4845,#4428,#4049,.T.);
#6613=EDGE_CURVE('',#4697,#4850,#4050,.T.);
#6614=EDGE_CURVE('',#5126,#4697,#665,.T.);
#6615=EDGE_CURVE('',#5128,#4506,#4051,.T.);
#6616=EDGE_CURVE('',#4846,#4427,#4052,.T.);
#6617=EDGE_CURVE('',#5126,#4849,#4053,.T.);
#6618=EDGE_CURVE('',#4501,#5199,#4054,.T.);
#6619=EDGE_CURVE('',#5129,#4505,#4055,.T.);
#6620=EDGE_CURVE('',#4847,#5132,#4056,.T.);
#6621=EDGE_CURVE('',#5127,#4848,#4057,.T.);
#6622=EDGE_CURVE('',#4502,#5124,#4058,.T.);
#6623=EDGE_CURVE('',#4504,#5180,#4059,.T.);
#6624=EDGE_CURVE('',#5181,#4503,#4060,.T.);
#6625=EDGE_CURVE('',#4505,#5179,#666,.T.);
#6626=EDGE_CURVE('',#5176,#4504,#4061,.T.);
#6627=EDGE_CURVE('',#5130,#5179,#4062,.T.);
#6628=EDGE_CURVE('',#5127,#5132,#667,.T.);
#6629=EDGE_CURVE('',#5181,#5124,#668,.T.);
#6630=EDGE_CURVE('',#5176,#5180,#4063,.T.);
#6631=EDGE_CURVE('',#5131,#5178,#4064,.T.);
#6632=EDGE_CURVE('',#5121,#5131,#4065,.T.);
#6633=EDGE_CURVE('',#5182,#5123,#4066,.T.);
#6634=EDGE_CURVE('',#5177,#5182,#669,.T.);
#6635=EDGE_CURVE('',#5121,#5178,#4067,.T.);
#6636=EDGE_CURVE('',#5177,#5122,#4068,.T.);
#6637=EDGE_CURVE('',#4763,#4424,#4069,.T.);
#6638=EDGE_CURVE('',#5001,#4762,#4070,.T.);
#6639=EDGE_CURVE('',#4763,#4423,#4071,.T.);
#6640=EDGE_CURVE('',#5001,#4970,#4072,.T.);
#6641=EDGE_CURVE('',#4970,#4762,#4073,.T.);
#6642=EDGE_CURVE('',#4764,#4420,#4074,.T.);
#6643=EDGE_CURVE('',#4963,#4767,#670,.T.);
#6644=EDGE_CURVE('',#4491,#4969,#4075,.T.);
#6645=EDGE_CURVE('',#4421,#4558,#4076,.T.);
#6646=EDGE_CURVE('',#4558,#4422,#4077,.T.);
#6647=EDGE_CURVE('',#4764,#4419,#4078,.T.);
#6648=EDGE_CURVE('',#4963,#4800,#4079,.T.);
#6649=EDGE_CURVE('',#4801,#4767,#4080,.T.);
#6650=EDGE_CURVE('',#4492,#4968,#4081,.T.);
#6651=EDGE_CURVE('',#4559,#5000,#4082,.T.);
#6652=EDGE_CURVE('',#4418,#4557,#4083,.T.);
#6653=EDGE_CURVE('',#4765,#4887,#4084,.T.);
#6654=EDGE_CURVE('',#4766,#4777,#671,.T.);
#6655=EDGE_CURVE('',#4778,#4765,#4085,.T.);
#6656=EDGE_CURVE('',#4802,#4766,#4086,.T.);
#6657=EDGE_CURVE('',#4964,#4799,#4087,.T.);
#6658=EDGE_CURVE('',#4998,#4967,#4088,.T.);
#6659=EDGE_CURVE('',#4559,#4961,#4089,.T.);
#6660=EDGE_CURVE('',#4961,#5000,#4090,.T.);
#6661=EDGE_CURVE('',#4417,#4557,#4091,.T.);
#6662=EDGE_CURVE('',#4778,#4887,#4092,.T.);
#6663=EDGE_CURVE('',#4803,#4777,#4093,.T.);
#6664=EDGE_CURVE('',#4965,#4986,#4094,.T.);
#6665=EDGE_CURVE('',#4998,#4954,#4095,.T.);
#6666=EDGE_CURVE('',#4954,#4967,#4096,.T.);
#6667=EDGE_CURVE('',#4560,#4960,#672,.T.);
#6668=EDGE_CURVE('',#4886,#4563,#4097,.T.);
#6669=EDGE_CURVE('',#4779,#4565,#4098,.T.);
#6670=EDGE_CURVE('',#4804,#4776,#4099,.T.);
#6671=EDGE_CURVE('',#4966,#4985,#4100,.T.);
#6672=EDGE_CURVE('',#4955,#4966,#673,.T.);
#6673=EDGE_CURVE('',#4999,#4953,#4101,.T.);
#6674=EDGE_CURVE('',#4560,#4783,#4102,.T.);
#6675=EDGE_CURVE('',#4782,#4960,#4103,.T.);
#6676=EDGE_CURVE('',#4886,#4773,#4104,.T.);
#6677=EDGE_CURVE('',#4773,#4563,#4105,.T.);
#6678=EDGE_CURVE('',#4780,#4564,#4106,.T.);
#6679=EDGE_CURVE('',#4811,#4775,#4107,.T.);
#6680=EDGE_CURVE('',#4955,#4984,#4108,.T.);
#6681=EDGE_CURVE('',#4999,#4948,#4109,.T.);
#6682=EDGE_CURVE('',#4948,#4953,#4110,.T.);
#6683=EDGE_CURVE('',#4962,#4997,#4111,.T.);
#6684=EDGE_CURVE('',#4784,#4959,#4112,.T.);
#6685=EDGE_CURVE('',#4562,#4789,#4113,.T.);
#6686=EDGE_CURVE('',#4768,#4562,#674,.T.);
#6687=EDGE_CURVE('',#4781,#4891,#4114,.T.);
#6688=EDGE_CURVE('',#4774,#4761,#675,.T.);
#6689=EDGE_CURVE('',#4756,#4781,#4115,.T.);
#6690=EDGE_CURVE('',#4812,#4774,#4116,.T.);
#6691=EDGE_CURVE('',#4956,#4983,#4117,.T.);
#6692=EDGE_CURVE('',#4949,#4952,#4118,.T.);
#6693=EDGE_CURVE('',#4996,#4947,#4119,.T.);
#6694=EDGE_CURVE('',#4997,#4490,#4120,.T.);
#6695=EDGE_CURVE('',#4484,#4996,#4121,.T.);
#6696=EDGE_CURVE('',#4962,#4490,#4122,.T.);
#6697=EDGE_CURVE('',#4975,#4958,#4123,.T.);
#6698=EDGE_CURVE('',#4768,#4788,#4124,.T.);
#6699=EDGE_CURVE('',#4756,#4891,#4125,.T.);
#6700=EDGE_CURVE('',#4813,#4761,#4126,.T.);
#6701=EDGE_CURVE('',#4653,#4982,#4127,.T.);
#6702=EDGE_CURVE('',#4956,#4653,#676,.T.);
#6703=EDGE_CURVE('',#4949,#5088,#4128,.T.);
#6704=EDGE_CURVE('',#5088,#4952,#4129,.T.);
#6705=EDGE_CURVE('',#4484,#4947,#4130,.T.);
#6706=EDGE_CURVE('',#4957,#4489,#677,.T.);
#6707=EDGE_CURVE('',#4976,#4957,#4131,.T.);
#6708=EDGE_CURVE('',#4769,#4787,#4132,.T.);
#6709=EDGE_CURVE('',#4888,#4772,#4133,.T.);
#6710=EDGE_CURVE('',#4757,#4890,#4134,.T.);
#6711=EDGE_CURVE('',#4807,#4760,#4135,.T.);
#6712=EDGE_CURVE('',#4654,#4981,#4136,.T.);
#6713=EDGE_CURVE('',#4951,#4652,#4137,.T.);
#6714=EDGE_CURVE('',#5089,#4951,#4138,.T.);
#6715=EDGE_CURVE('',#4950,#5087,#4139,.T.);
#6716=EDGE_CURVE('',#4485,#4950,#4140,.T.);
#6717=EDGE_CURVE('',#4977,#4489,#4141,.T.);
#6718=EDGE_CURVE('',#4770,#4796,#4142,.T.);
#6719=EDGE_CURVE('',#4888,#4749,#4143,.T.);
#6720=EDGE_CURVE('',#4749,#4772,#4144,.T.);
#6721=EDGE_CURVE('',#4757,#4754,#4145,.T.);
#6722=EDGE_CURVE('',#4754,#4890,#4146,.T.);
#6723=EDGE_CURVE('',#5156,#4760,#678,.T.);
#6724=EDGE_CURVE('',#4806,#5156,#4147,.T.);
#6725=EDGE_CURVE('',#4649,#5071,#4148,.T.);
#6726=EDGE_CURVE('',#5089,#4652,#4149,.T.);
#6727=EDGE_CURVE('',#4485,#5087,#4150,.T.);
#6728=EDGE_CURVE('',#4978,#4487,#4151,.T.);
#6729=EDGE_CURVE('',#4771,#4795,#4152,.T.);
#6730=EDGE_CURVE('',#4750,#4771,#679,.T.);
#6731=EDGE_CURVE('',#4889,#4748,#4153,.T.);
#6732=EDGE_CURVE('',#4755,#4889,#4154,.T.);
#6733=EDGE_CURVE('',#4758,#4753,#4155,.T.);
#6734=EDGE_CURVE('',#4759,#5165,#4156,.T.);
#6735=EDGE_CURVE('',#5166,#4758,#4157,.T.);
#6736=EDGE_CURVE('',#5157,#4759,#4158,.T.);
#6737=EDGE_CURVE('',#4808,#5155,#4159,.T.);
#6738=EDGE_CURVE('',#4650,#5070,#4160,.T.);
#6739=EDGE_CURVE('',#4486,#5086,#4161,.T.);
#6740=EDGE_CURVE('',#4487,#4635,#680,.T.);
#6741=EDGE_CURVE('',#4636,#4486,#4162,.T.);
#6742=EDGE_CURVE('',#4971,#4635,#4163,.T.);
#6743=EDGE_CURVE('',#4750,#4794,#4164,.T.);
#6744=EDGE_CURVE('',#4755,#4748,#4165,.T.);
#6745=EDGE_CURVE('',#5166,#4753,#4166,.T.);
#6746=EDGE_CURVE('',#5157,#5165,#4167,.T.);
#6747=EDGE_CURVE('',#5066,#5154,#4168,.T.);
#6748=EDGE_CURVE('',#5055,#5069,#4169,.T.);
#6749=EDGE_CURVE('',#4650,#5055,#681,.T.);
#6750=EDGE_CURVE('',#4636,#5086,#4170,.T.);
#6751=EDGE_CURVE('',#4972,#4634,#4171,.T.);
#6752=EDGE_CURVE('',#4751,#4793,#4172,.T.);
#6753=EDGE_CURVE('',#4752,#4747,#4173,.T.);
#6754=EDGE_CURVE('',#5163,#4752,#4174,.T.);
#6755=EDGE_CURVE('',#5067,#5153,#4175,.T.);
#6756=EDGE_CURVE('',#5056,#5068,#4176,.T.);
#6757=EDGE_CURVE('',#4651,#5054,#4177,.T.);
#6758=EDGE_CURVE('',#5084,#4651,#4178,.T.);
#6759=EDGE_CURVE('',#4637,#4479,#4179,.T.);
#6760=EDGE_CURVE('',#5062,#4641,#4180,.T.);
#6761=EDGE_CURVE('',#5145,#4792,#4181,.T.);
#6762=EDGE_CURVE('',#4751,#5145,#682,.T.);
#6763=EDGE_CURVE('',#5163,#4747,#4182,.T.);
#6764=EDGE_CURVE('',#5056,#5153,#683,.T.);
#6765=EDGE_CURVE('',#5084,#5054,#4183,.T.);
#6766=EDGE_CURVE('',#4638,#4478,#4184,.T.);
#6767=EDGE_CURVE('',#5063,#4640,#4185,.T.);
#6768=EDGE_CURVE('',#5146,#4790,#4186,.T.);
#6769=EDGE_CURVE('',#4746,#5152,#4187,.T.);
#6770=EDGE_CURVE('',#5164,#4746,#4188,.T.);
#6771=EDGE_CURVE('',#5158,#5170,#4189,.T.);
#6772=EDGE_CURVE('',#5053,#5158,#4190,.T.);
#6773=EDGE_CURVE('',#5085,#4398,#4191,.T.);
#6774=EDGE_CURVE('',#4639,#5083,#4192,.T.);
#6775=EDGE_CURVE('',#4640,#4476,#684,.T.);
#6776=EDGE_CURVE('',#4477,#4639,#4193,.T.);
#6777=EDGE_CURVE('',#5064,#4476,#4194,.T.);
#6778=EDGE_CURVE('',#5147,#5059,#4195,.T.);
#6779=EDGE_CURVE('',#5164,#5152,#4196,.T.);
#6780=EDGE_CURVE('',#5053,#5170,#4197,.T.);
#6781=EDGE_CURVE('',#5085,#4400,#4198,.T.);
#6782=EDGE_CURVE('',#4477,#5083,#4199,.T.);
#6783=EDGE_CURVE('',#5058,#4474,#4200,.T.);
#6784=EDGE_CURVE('',#5148,#5057,#4201,.T.);
#6785=EDGE_CURVE('',#4465,#5151,#4202,.T.);
#6786=EDGE_CURVE('',#4397,#5169,#4203,.T.);
#6787=EDGE_CURVE('',#5082,#4394,#4204,.T.);
#6788=EDGE_CURVE('',#4396,#5082,#4205,.T.);
#6789=EDGE_CURVE('',#5148,#4474,#685,.T.);
#6790=EDGE_CURVE('',#4466,#5150,#4206,.T.);
#6791=EDGE_CURVE('',#4399,#5169,#4207,.T.);
#6792=EDGE_CURVE('',#5149,#4473,#4208,.T.);
#6793=EDGE_CURVE('',#5167,#5149,#4209,.T.);
#6794=EDGE_CURVE('',#4393,#5168,#4210,.T.);
#6795=EDGE_CURVE('',#5167,#4473,#4211,.T.);
#6796=EDGE_CURVE('',#4395,#5168,#4212,.T.);
#6797=EDGE_CURVE('',#5078,#5215,#686,.T.);
#6798=EDGE_CURVE('',#5081,#5216,#687,.T.);
#6799=EDGE_CURVE('',#5216,#5215,#688,.T.);
#6800=EDGE_CURVE('',#5216,#5075,#689,.T.);
#6801=EDGE_CURVE('',#5075,#5217,#690,.T.);
#6802=EDGE_CURVE('',#5217,#5215,#691,.T.);
#6803=EDGE_CURVE('',#5217,#4552,#692,.T.);
#6804=EDGE_CURVE('',#4499,#5215,#693,.T.);
#6805=EDGE_CURVE('',#4498,#5218,#694,.T.);
#6806=EDGE_CURVE('',#5218,#5215,#695,.T.);
#6807=EDGE_CURVE('',#5218,#5160,#696,.T.);
#6808=EDGE_CURVE('',#5219,#5160,#697,.T.);
#6809=EDGE_CURVE('',#5219,#5215,#698,.T.);
#6810=EDGE_CURVE('',#5220,#5221,#699,.T.);
#6811=EDGE_CURVE('',#5220,#4991,#700,.T.);
#6812=EDGE_CURVE('',#4992,#5221,#701,.T.);
#6813=EDGE_CURVE('',#4995,#5222,#702,.T.);
#6814=EDGE_CURVE('',#5222,#5221,#703,.T.);
#6815=EDGE_CURVE('',#5222,#4989,#704,.T.);
#6816=EDGE_CURVE('',#4989,#5223,#705,.T.);
#6817=EDGE_CURVE('',#5223,#5221,#706,.T.);
#6818=EDGE_CURVE('',#5223,#4555,#707,.T.);
#6819=EDGE_CURVE('',#4554,#5221,#708,.T.);
#6820=EDGE_CURVE('',#5224,#4553,#4213,.T.);
#6821=EDGE_CURVE('',#5224,#5221,#709,.T.);
#6822=EDGE_CURVE('',#4496,#5225,#710,.T.);
#6823=EDGE_CURVE('',#4495,#5226,#711,.T.);
#6824=EDGE_CURVE('',#5226,#5225,#712,.T.);
#6825=EDGE_CURVE('',#5226,#4873,#713,.T.);
#6826=EDGE_CURVE('',#4873,#5227,#714,.T.);
#6827=EDGE_CURVE('',#5227,#5225,#715,.T.);
#6828=EDGE_CURVE('',#5227,#4690,#716,.T.);
#6829=EDGE_CURVE('',#4688,#5225,#717,.T.);
#6830=EDGE_CURVE('',#4689,#5228,#718,.T.);
#6831=EDGE_CURVE('',#5228,#5225,#719,.T.);
#6832=EDGE_CURVE('',#5228,#5161,#720,.T.);
#6833=EDGE_CURVE('',#5229,#5161,#721,.T.);
#6834=EDGE_CURVE('',#5229,#5225,#722,.T.);
#6835=EDGE_CURVE('',#5230,#5231,#723,.T.);
#6836=EDGE_CURVE('',#5230,#4876,#724,.T.);
#6837=EDGE_CURVE('',#4877,#5231,#725,.T.);
#6838=EDGE_CURVE('',#4880,#5232,#726,.T.);
#6839=EDGE_CURVE('',#5232,#5231,#727,.T.);
#6840=EDGE_CURVE('',#5232,#4874,#728,.T.);
#6841=EDGE_CURVE('',#5233,#4874,#729,.T.);
#6842=EDGE_CURVE('',#5233,#5231,#730,.T.);
#6843=EDGE_CURVE('',#4493,#5233,#4214,.T.);
#6844=EDGE_CURVE('',#4494,#5231,#731,.T.);
#6845=EDGE_CURVE('',#5234,#4556,#4215,.T.);
#6846=EDGE_CURVE('',#5234,#5231,#732,.T.);
#6847=EDGE_CURVE('',#4616,#4878,#4216,.T.);
#6848=EDGE_CURVE('',#4879,#4615,#4217,.T.);
#6849=EDGE_CURVE('',#4987,#4878,#733,.T.);
#6850=EDGE_CURVE('',#4617,#4987,#4218,.T.);
#6851=EDGE_CURVE('',#4875,#4614,#4219,.T.);
#6852=EDGE_CURVE('',#4879,#4875,#734,.T.);
#6853=EDGE_CURVE('',#4988,#5230,#735,.T.);
#6854=EDGE_CURVE('',#4618,#4990,#4220,.T.);
#6855=EDGE_CURVE('',#4605,#4993,#4221,.T.);
#6856=EDGE_CURVE('',#4994,#4619,#4222,.T.);
#6857=EDGE_CURVE('',#4872,#4613,#4223,.T.);
#6858=EDGE_CURVE('',#4988,#5234,#736,.T.);
#6859=EDGE_CURVE('',#4994,#4990,#737,.T.);
#6860=EDGE_CURVE('',#5073,#4993,#738,.T.);
#6861=EDGE_CURVE('',#4604,#5073,#4224,.T.);
#6862=EDGE_CURVE('',#4691,#4612,#4225,.T.);
#6863=EDGE_CURVE('',#4872,#4691,#739,.T.);
#6864=EDGE_CURVE('',#5074,#5220,#740,.T.);
#6865=EDGE_CURVE('',#4606,#5076,#4226,.T.);
#6866=EDGE_CURVE('',#4692,#4611,#4227,.T.);
#6867=EDGE_CURVE('',#5162,#4692,#741,.T.);
#6868=EDGE_CURVE('',#4497,#5229,#4228,.T.);
#6869=EDGE_CURVE('',#5074,#5224,#742,.T.);
#6870=EDGE_CURVE('',#5080,#5076,#743,.T.);
#6871=EDGE_CURVE('',#4607,#5080,#4229,.T.);
#6872=EDGE_CURVE('',#5162,#4610,#4230,.T.);
#6873=EDGE_CURVE('',#4608,#5079,#4231,.T.);
#6874=EDGE_CURVE('',#5159,#4609,#4232,.T.);
#6875=EDGE_CURVE('',#5077,#5219,#4233,.T.);
#6876=EDGE_CURVE('',#5159,#5079,#744,.T.);
#6877=EDGE_CURVE('',#4814,#4974,#4234,.T.);
#6878=EDGE_CURVE('',#4785,#4840,#4235,.T.);
#6879=EDGE_CURVE('',#4786,#4839,#4236,.T.);
#6880=EDGE_CURVE('',#4815,#4973,#4237,.T.);
#6881=EDGE_CURVE('',#4797,#4838,#4238,.T.);
#6882=EDGE_CURVE('',#4835,#5061,#4239,.T.);
#6883=EDGE_CURVE('',#4791,#4837,#4240,.T.);
#6884=EDGE_CURVE('',#4836,#5060,#4241,.T.);
#6885=EDGE_CURVE('',#4979,#4583,#4242,.T.);
#6886=EDGE_CURVE('',#4584,#4798,#4243,.T.);
#6887=EDGE_CURVE('',#4585,#4805,#4244,.T.);
#6888=EDGE_CURVE('',#4980,#4582,#4245,.T.);
#6889=EDGE_CURVE('',#4586,#4810,#4246,.T.);
#6890=EDGE_CURVE('',#5072,#4589,#4247,.T.);
#6891=EDGE_CURVE('',#4587,#4809,#4248,.T.);
#6892=EDGE_CURVE('',#5065,#4588,#4249,.T.);
#6893=EDGE_CURVE('',#4574,#4472,#4250,.T.);
#6894=EDGE_CURVE('',#4575,#5110,#4251,.T.);
#6895=EDGE_CURVE('',#4580,#5107,#4252,.T.);
#6896=EDGE_CURVE('',#4469,#4579,#4253,.T.);
#6897=EDGE_CURVE('',#4576,#5109,#4254,.T.);
#6898=EDGE_CURVE('',#4470,#4578,#4255,.T.);
#6899=EDGE_CURVE('',#4577,#5104,#4256,.T.);
#6900=EDGE_CURVE('',#4471,#5119,#4257,.T.);
#6901=EDGE_CURVE('',#5111,#5118,#4258,.T.);
#6902=EDGE_CURVE('',#5112,#5106,#4259,.T.);
#6903=EDGE_CURVE('',#5114,#4468,#4260,.T.);
#6904=EDGE_CURVE('',#5108,#5117,#4261,.T.);
#6905=EDGE_CURVE('',#5115,#4467,#4262,.T.);
#6906=EDGE_CURVE('',#5105,#5116,#4263,.T.);
#6907=EDGE_CURVE('',#5018,#4598,#4264,.T.);
#6908=EDGE_CURVE('',#4599,#5019,#4265,.T.);
#6909=EDGE_CURVE('',#4482,#4597,#4266,.T.);
#6910=EDGE_CURVE('',#4483,#4596,#4267,.T.);
#6911=EDGE_CURVE('',#5021,#5017,#4268,.T.);
#6912=EDGE_CURVE('',#5020,#5024,#4269,.T.);
#6913=EDGE_CURVE('',#5022,#4481,#4270,.T.);
#6914=EDGE_CURVE('',#5023,#4480,#4271,.T.);
#6915=EDGE_CURVE('',#4913,#4601,#4272,.T.);
#6916=EDGE_CURVE('',#4602,#4916,#4273,.T.);
#6917=EDGE_CURVE('',#4603,#4915,#4274,.T.);
#6918=EDGE_CURVE('',#4600,#4910,#4275,.T.);
#6919=EDGE_CURVE('',#4918,#4912,#4276,.T.);
#6920=EDGE_CURVE('',#4917,#4921,#4277,.T.);
#6921=EDGE_CURVE('',#4914,#4920,#4278,.T.);
#6922=EDGE_CURVE('',#4911,#4919,#4279,.T.);
#6923=EDGE_CURVE('',#4675,#4726,#2940,.T.);
#6924=EDGE_CURVE('',#4676,#4725,#2941,.T.);
#6925=EDGE_CURVE('',#4706,#4674,#2942,.T.);
#6926=EDGE_CURVE('',#4673,#4705,#2943,.T.);
#6927=EDGE_CURVE('',#4831,#4629,#2944,.T.);
#6928=EDGE_CURVE('',#4830,#4677,#2945,.T.);
#6929=EDGE_CURVE('',#5235,#4566,#2946,.T.);
#6930=EDGE_CURVE('',#4630,#5235,#2947,.T.);
#6931=EDGE_CURVE('',#5236,#4818,#2948,.T.);
#6932=EDGE_CURVE('',#4567,#5236,#2949,.T.);
#6933=EDGE_CURVE('',#4633,#4816,#2950,.T.);
#6934=EDGE_CURVE('',#4632,#4817,#2951,.T.);
#6935=EDGE_CURVE('',#4631,#5237,#2952,.T.);
#6936=EDGE_CURVE('',#5236,#5237,#2953,.T.);
#6937=EDGE_CURVE('',#5235,#5237,#2954,.T.);
#6938=EDGE_CURVE('',#4644,#4834,#2955,.T.);
#6939=EDGE_CURVE('',#4645,#4833,#2956,.T.);
#6940=EDGE_CURVE('',#4628,#4832,#2957,.T.);
#6941=EDGE_CURVE('',#4572,#4647,#2958,.T.);
#6942=EDGE_CURVE('',#4573,#4659,#2959,.T.);
#6943=EDGE_CURVE('',#5120,#4658,#2960,.T.);
#6944=EDGE_CURVE('',#4581,#4655,#2961,.T.);
#6945=EDGE_CURVE('',#4580,#4656,#2962,.T.);
#6946=EDGE_CURVE('',#5113,#4657,#2963,.T.);
#6947=EDGE_CURVE('',#5238,#5238,#4280,.T.);
#6948=EDGE_CURVE('',#5238,#5239,#2964,.T.);
#6949=EDGE_CURVE('',#5239,#5240,#745,.T.);
#6950=EDGE_CURVE('',#5240,#5241,#4281,.T.);
#6951=EDGE_CURVE('',#5241,#5242,#746,.T.);
#6952=EDGE_CURVE('',#5242,#5243,#747,.T.);
#6953=EDGE_CURVE('',#5243,#5244,#4282,.T.);
#6954=EDGE_CURVE('',#5244,#5245,#748,.T.);
#6955=EDGE_CURVE('',#5245,#5246,#749,.T.);
#6956=EDGE_CURVE('',#5246,#5247,#4283,.T.);
#6957=EDGE_CURVE('',#5247,#5248,#4284,.T.);
#6958=EDGE_CURVE('',#5248,#5249,#750,.T.);
#6959=EDGE_CURVE('',#5249,#5250,#751,.F.);
#6960=EDGE_CURVE('',#5250,#5251,#4285,.T.);
#6961=EDGE_CURVE('',#5251,#5252,#752,.T.);
#6962=EDGE_CURVE('',#5252,#5253,#753,.T.);
#6963=EDGE_CURVE('',#5253,#5254,#4286,.T.);
#6964=EDGE_CURVE('',#5254,#5255,#754,.T.);
#6965=EDGE_CURVE('',#5255,#5256,#755,.T.);
#6966=EDGE_CURVE('',#5256,#5257,#4287,.T.);
#6967=EDGE_CURVE('',#5257,#5258,#756,.T.);
#6968=EDGE_CURVE('',#5258,#5259,#757,.T.);
#6969=EDGE_CURVE('',#5259,#5260,#4288,.T.);
#6970=EDGE_CURVE('',#5261,#5260,#2965,.T.);
#6971=EDGE_CURVE('',#5261,#5262,#758,.T.);
#6972=EDGE_CURVE('',#5262,#5239,#759,.T.);
#6973=EDGE_CURVE('',#5263,#5263,#4289,.T.);
#6974=EDGE_CURVE('',#5263,#5264,#4290,.T.);
#6975=EDGE_CURVE('',#5264,#5264,#4291,.T.);
#6976=EDGE_CURVE('',#5265,#5265,#4292,.T.);
#6977=EDGE_CURVE('',#5265,#5266,#2966,.T.);
#6978=EDGE_CURVE('',#5266,#5266,#4293,.T.);
#6979=EDGE_CURVE('',#5267,#5267,#4294,.T.);
#6980=EDGE_CURVE('',#5267,#5268,#4295,.T.);
#6981=EDGE_CURVE('',#5268,#5268,#4296,.T.);
#6982=EDGE_CURVE('',#5268,#5269,#2967,.T.);
#6983=EDGE_CURVE('',#5269,#5269,#4297,.T.);
#6984=EDGE_CURVE('',#5270,#5271,#760,.F.);
#6985=EDGE_CURVE('',#5272,#5270,#2968,.T.);
#6986=EDGE_CURVE('',#5271,#5272,#761,.F.);
#6987=EDGE_CURVE('',#5273,#5273,#4298,.T.);
#6988=EDGE_CURVE('',#5273,#5247,#4299,.T.);
#6989=EDGE_CURVE('',#5274,#5246,#762,.T.);
#6990=EDGE_CURVE('',#5275,#5274,#763,.T.);
#6991=EDGE_CURVE('',#5244,#5275,#764,.T.);
#6992=EDGE_CURVE('',#5276,#5243,#765,.T.);
#6993=EDGE_CURVE('',#5277,#5276,#766,.T.);
#6994=EDGE_CURVE('',#5241,#5277,#767,.T.);
#6995=EDGE_CURVE('',#5278,#5240,#768,.T.);
#6996=EDGE_CURVE('',#5279,#5278,#769,.T.);
#6997=EDGE_CURVE('',#5280,#5279,#770,.T.);
#6998=EDGE_CURVE('',#5260,#5280,#4300,.T.);
#6999=EDGE_CURVE('',#5281,#5259,#771,.T.);
#7000=EDGE_CURVE('',#5282,#5281,#772,.T.);
#7001=EDGE_CURVE('',#5257,#5282,#773,.T.);
#7002=EDGE_CURVE('',#5283,#5256,#774,.T.);
#7003=EDGE_CURVE('',#5284,#5283,#775,.T.);
#7004=EDGE_CURVE('',#5254,#5284,#776,.T.);
#7005=EDGE_CURVE('',#5285,#5253,#777,.T.);
#7006=EDGE_CURVE('',#5286,#5285,#778,.T.);
#7007=EDGE_CURVE('',#5251,#5286,#779,.T.);
#7008=EDGE_CURVE('',#5287,#5250,#780,.T.);
#7009=EDGE_CURVE('',#5288,#5287,#781,.T.);
#7010=EDGE_CURVE('',#5248,#5288,#782,.T.);
#7011=EDGE_CURVE('',#5280,#5261,#783,.T.);
#7012=EDGE_CURVE('',#5281,#5289,#784,.T.);
#7013=EDGE_CURVE('',#5289,#5290,#2969,.T.);
#7014=EDGE_CURVE('',#5290,#5282,#785,.T.);
#7015=EDGE_CURVE('',#5291,#5258,#786,.T.);
#7016=EDGE_CURVE('',#5291,#5289,#787,.T.);
#7017=EDGE_CURVE('',#5290,#5291,#788,.T.);
#7018=EDGE_CURVE('',#5292,#5279,#789,.T.);
#7019=EDGE_CURVE('',#5292,#5293,#790,.T.);
#7020=EDGE_CURVE('',#5293,#5262,#791,.T.);
#7021=EDGE_CURVE('',#5293,#5294,#792,.T.);
#7022=EDGE_CURVE('',#5278,#5294,#793,.T.);
#7023=EDGE_CURVE('',#5294,#5292,#2970,.T.);
#7024=EDGE_CURVE('',#5295,#5277,#794,.T.);
#7025=EDGE_CURVE('',#5295,#5296,#795,.T.);
#7026=EDGE_CURVE('',#5296,#5242,#796,.T.);
#7027=EDGE_CURVE('',#5296,#5297,#797,.T.);
#7028=EDGE_CURVE('',#5276,#5297,#798,.T.);
#7029=EDGE_CURVE('',#5297,#5295,#2971,.T.);
#7030=EDGE_CURVE('',#5298,#5275,#799,.T.);
#7031=EDGE_CURVE('',#5298,#5299,#800,.T.);
#7032=EDGE_CURVE('',#5299,#5245,#801,.T.);
#7033=EDGE_CURVE('',#5299,#5300,#802,.T.);
#7034=EDGE_CURVE('',#5274,#5300,#803,.T.);
#7035=EDGE_CURVE('',#5300,#5298,#2972,.T.);
#7036=EDGE_CURVE('',#5270,#5288,#804,.T.);
#7037=EDGE_CURVE('',#5271,#5249,#805,.T.);
#7038=EDGE_CURVE('',#5287,#5272,#806,.T.);
#7039=EDGE_CURVE('',#5301,#5286,#807,.T.);
#7040=EDGE_CURVE('',#5301,#5302,#808,.T.);
#7041=EDGE_CURVE('',#5302,#5252,#809,.T.);
#7042=EDGE_CURVE('',#5302,#5303,#810,.T.);
#7043=EDGE_CURVE('',#5285,#5303,#811,.T.);
#7044=EDGE_CURVE('',#5303,#5301,#2973,.T.);
#7045=EDGE_CURVE('',#5304,#5284,#812,.T.);
#7046=EDGE_CURVE('',#5304,#5305,#813,.T.);
#7047=EDGE_CURVE('',#5305,#5255,#814,.T.);
#7048=EDGE_CURVE('',#5305,#5306,#815,.T.);
#7049=EDGE_CURVE('',#5283,#5306,#816,.T.);
#7050=EDGE_CURVE('',#5306,#5304,#2974,.T.);
#7051=ORIENTED_EDGE('',*,*,#5307,.F.);
#7052=ORIENTED_EDGE('',*,*,#5308,.T.);
#7053=ORIENTED_EDGE('',*,*,#5309,.T.);
#7054=ORIENTED_EDGE('',*,*,#5308,.F.);
#7055=ORIENTED_EDGE('',*,*,#5310,.F.);
#7056=ORIENTED_EDGE('',*,*,#5311,.T.);
#7057=ORIENTED_EDGE('',*,*,#5312,.T.);
#7058=ORIENTED_EDGE('',*,*,#5311,.F.);
#7059=ORIENTED_EDGE('',*,*,#5313,.F.);
#7060=ORIENTED_EDGE('',*,*,#5314,.T.);
#7061=ORIENTED_EDGE('',*,*,#5315,.T.);
#7062=ORIENTED_EDGE('',*,*,#5314,.F.);
#7063=ORIENTED_EDGE('',*,*,#5316,.F.);
#7064=ORIENTED_EDGE('',*,*,#5317,.T.);
#7065=ORIENTED_EDGE('',*,*,#5318,.T.);
#7066=ORIENTED_EDGE('',*,*,#5317,.F.);
#7067=ORIENTED_EDGE('',*,*,#5319,.F.);
#7068=ORIENTED_EDGE('',*,*,#5320,.F.);
#7069=ORIENTED_EDGE('',*,*,#5321,.T.);
#7070=ORIENTED_EDGE('',*,*,#5322,.F.);
#7071=ORIENTED_EDGE('',*,*,#5321,.F.);
#7072=ORIENTED_EDGE('',*,*,#5323,.F.);
#7073=ORIENTED_EDGE('',*,*,#5324,.T.);
#7074=ORIENTED_EDGE('',*,*,#5325,.F.);
#7075=ORIENTED_EDGE('',*,*,#5326,.F.);
#7076=ORIENTED_EDGE('',*,*,#5324,.F.);
#7077=ORIENTED_EDGE('',*,*,#5327,.F.);
#7078=ORIENTED_EDGE('',*,*,#5328,.T.);
#7079=ORIENTED_EDGE('',*,*,#5329,.F.);
#7080=ORIENTED_EDGE('',*,*,#5328,.F.);
#7081=ORIENTED_EDGE('',*,*,#5330,.F.);
#7082=ORIENTED_EDGE('',*,*,#5331,.T.);
#7083=ORIENTED_EDGE('',*,*,#5332,.F.);
#7084=ORIENTED_EDGE('',*,*,#5333,.F.);
#7085=ORIENTED_EDGE('',*,*,#5331,.F.);
#7086=ORIENTED_EDGE('',*,*,#5334,.F.);
#7087=ORIENTED_EDGE('',*,*,#5335,.T.);
#7088=ORIENTED_EDGE('',*,*,#5336,.F.);
#7089=ORIENTED_EDGE('',*,*,#5337,.F.);
#7090=ORIENTED_EDGE('',*,*,#5338,.F.);
#7091=ORIENTED_EDGE('',*,*,#5339,.F.);
#7092=ORIENTED_EDGE('',*,*,#5340,.F.);
#7093=ORIENTED_EDGE('',*,*,#5341,.F.);
#7094=ORIENTED_EDGE('',*,*,#5342,.F.);
#7095=ORIENTED_EDGE('',*,*,#5343,.F.);
#7096=ORIENTED_EDGE('',*,*,#5344,.F.);
#7097=ORIENTED_EDGE('',*,*,#5345,.T.);
#7098=ORIENTED_EDGE('',*,*,#5346,.F.);
#7099=ORIENTED_EDGE('',*,*,#5347,.F.);
#7100=ORIENTED_EDGE('',*,*,#5348,.F.);
#7101=ORIENTED_EDGE('',*,*,#5349,.F.);
#7102=ORIENTED_EDGE('',*,*,#5350,.F.);
#7103=ORIENTED_EDGE('',*,*,#5351,.F.);
#7104=ORIENTED_EDGE('',*,*,#5352,.T.);
#7105=ORIENTED_EDGE('',*,*,#5353,.F.);
#7106=ORIENTED_EDGE('',*,*,#5352,.F.);
#7107=ORIENTED_EDGE('',*,*,#5354,.F.);
#7108=ORIENTED_EDGE('',*,*,#5355,.T.);
#7109=ORIENTED_EDGE('',*,*,#5356,.F.);
#7110=ORIENTED_EDGE('',*,*,#5357,.F.);
#7111=ORIENTED_EDGE('',*,*,#5355,.F.);
#7112=ORIENTED_EDGE('',*,*,#5358,.F.);
#7113=ORIENTED_EDGE('',*,*,#5359,.T.);
#7114=ORIENTED_EDGE('',*,*,#5360,.F.);
#7115=ORIENTED_EDGE('',*,*,#5361,.F.);
#7116=ORIENTED_EDGE('',*,*,#5359,.F.);
#7117=ORIENTED_EDGE('',*,*,#5362,.F.);
#7118=ORIENTED_EDGE('',*,*,#5363,.T.);
#7119=ORIENTED_EDGE('',*,*,#5364,.F.);
#7120=ORIENTED_EDGE('',*,*,#5365,.F.);
#7121=ORIENTED_EDGE('',*,*,#5363,.F.);
#7122=ORIENTED_EDGE('',*,*,#5366,.F.);
#7123=ORIENTED_EDGE('',*,*,#5367,.F.);
#7124=ORIENTED_EDGE('',*,*,#5368,.F.);
#7125=ORIENTED_EDGE('',*,*,#5369,.T.);
#7126=ORIENTED_EDGE('',*,*,#5370,.F.);
#7127=ORIENTED_EDGE('',*,*,#5371,.F.);
#7128=ORIENTED_EDGE('',*,*,#5372,.F.);
#7129=ORIENTED_EDGE('',*,*,#5373,.F.);
#7130=ORIENTED_EDGE('',*,*,#5374,.F.);
#7131=ORIENTED_EDGE('',*,*,#5375,.T.);
#7132=ORIENTED_EDGE('',*,*,#5376,.F.);
#7133=ORIENTED_EDGE('',*,*,#5377,.F.);
#7134=ORIENTED_EDGE('',*,*,#5378,.F.);
#7135=ORIENTED_EDGE('',*,*,#5379,.F.);
#7136=ORIENTED_EDGE('',*,*,#5380,.F.);
#7137=ORIENTED_EDGE('',*,*,#5381,.F.);
#7138=ORIENTED_EDGE('',*,*,#5382,.F.);
#7139=ORIENTED_EDGE('',*,*,#5383,.T.);
#7140=ORIENTED_EDGE('',*,*,#5384,.F.);
#7141=ORIENTED_EDGE('',*,*,#5383,.F.);
#7142=ORIENTED_EDGE('',*,*,#5385,.F.);
#7143=ORIENTED_EDGE('',*,*,#5386,.T.);
#7144=ORIENTED_EDGE('',*,*,#5387,.F.);
#7145=ORIENTED_EDGE('',*,*,#5386,.F.);
#7146=ORIENTED_EDGE('',*,*,#5388,.F.);
#7147=ORIENTED_EDGE('',*,*,#5389,.T.);
#7148=ORIENTED_EDGE('',*,*,#5390,.F.);
#7149=ORIENTED_EDGE('',*,*,#5391,.F.);
#7150=ORIENTED_EDGE('',*,*,#5389,.F.);
#7151=ORIENTED_EDGE('',*,*,#5392,.F.);
#7152=ORIENTED_EDGE('',*,*,#5393,.T.);
#7153=ORIENTED_EDGE('',*,*,#5394,.F.);
#7154=ORIENTED_EDGE('',*,*,#5393,.F.);
#7155=ORIENTED_EDGE('',*,*,#5395,.F.);
#7156=ORIENTED_EDGE('',*,*,#5396,.T.);
#7157=ORIENTED_EDGE('',*,*,#5397,.F.);
#7158=ORIENTED_EDGE('',*,*,#5398,.F.);
#7159=ORIENTED_EDGE('',*,*,#5399,.F.);
#7160=ORIENTED_EDGE('',*,*,#5400,.F.);
#7161=ORIENTED_EDGE('',*,*,#5401,.F.);
#7162=ORIENTED_EDGE('',*,*,#5402,.T.);
#7163=ORIENTED_EDGE('',*,*,#5403,.F.);
#7164=ORIENTED_EDGE('',*,*,#5404,.T.);
#7165=ORIENTED_EDGE('',*,*,#5405,.F.);
#7166=ORIENTED_EDGE('',*,*,#5404,.F.);
#7167=ORIENTED_EDGE('',*,*,#5406,.F.);
#7168=ORIENTED_EDGE('',*,*,#5407,.F.);
#7169=ORIENTED_EDGE('',*,*,#5408,.T.);
#7170=ORIENTED_EDGE('',*,*,#5409,.F.);
#7171=ORIENTED_EDGE('',*,*,#5410,.F.);
#7172=ORIENTED_EDGE('',*,*,#5408,.F.);
#7173=ORIENTED_EDGE('',*,*,#5411,.F.);
#7174=ORIENTED_EDGE('',*,*,#5412,.T.);
#7175=ORIENTED_EDGE('',*,*,#5413,.F.);
#7176=ORIENTED_EDGE('',*,*,#5414,.F.);
#7177=ORIENTED_EDGE('',*,*,#5412,.F.);
#7178=ORIENTED_EDGE('',*,*,#5415,.F.);
#7179=ORIENTED_EDGE('',*,*,#5416,.T.);
#7180=ORIENTED_EDGE('',*,*,#5417,.F.);
#7181=ORIENTED_EDGE('',*,*,#5418,.F.);
#7182=ORIENTED_EDGE('',*,*,#5416,.F.);
#7183=ORIENTED_EDGE('',*,*,#5419,.F.);
#7184=ORIENTED_EDGE('',*,*,#5420,.F.);
#7185=ORIENTED_EDGE('',*,*,#5421,.F.);
#7186=ORIENTED_EDGE('',*,*,#5422,.T.);
#7187=ORIENTED_EDGE('',*,*,#5423,.F.);
#7188=ORIENTED_EDGE('',*,*,#5424,.F.);
#7189=ORIENTED_EDGE('',*,*,#5425,.F.);
#7190=ORIENTED_EDGE('',*,*,#5426,.T.);
#7191=ORIENTED_EDGE('',*,*,#5427,.F.);
#7192=ORIENTED_EDGE('',*,*,#5428,.T.);
#7193=ORIENTED_EDGE('',*,*,#5429,.F.);
#7194=ORIENTED_EDGE('',*,*,#5430,.F.);
#7195=ORIENTED_EDGE('',*,*,#5431,.F.);
#7196=ORIENTED_EDGE('',*,*,#5432,.F.);
#7197=ORIENTED_EDGE('',*,*,#5433,.F.);
#7198=ORIENTED_EDGE('',*,*,#5434,.T.);
#7199=ORIENTED_EDGE('',*,*,#5435,.F.);
#7200=ORIENTED_EDGE('',*,*,#5436,.F.);
#7201=ORIENTED_EDGE('',*,*,#5437,.F.);
#7202=ORIENTED_EDGE('',*,*,#5438,.T.);
#7203=ORIENTED_EDGE('',*,*,#5439,.F.);
#7204=ORIENTED_EDGE('',*,*,#5440,.T.);
#7205=ORIENTED_EDGE('',*,*,#5441,.F.);
#7206=ORIENTED_EDGE('',*,*,#5442,.F.);
#7207=ORIENTED_EDGE('',*,*,#5443,.F.);
#7208=ORIENTED_EDGE('',*,*,#5444,.F.);
#7209=ORIENTED_EDGE('',*,*,#5445,.T.);
#7210=ORIENTED_EDGE('',*,*,#5446,.F.);
#7211=ORIENTED_EDGE('',*,*,#5447,.F.);
#7212=ORIENTED_EDGE('',*,*,#5448,.F.);
#7213=ORIENTED_EDGE('',*,*,#5449,.T.);
#7214=ORIENTED_EDGE('',*,*,#5450,.F.);
#7215=ORIENTED_EDGE('',*,*,#5451,.T.);
#7216=ORIENTED_EDGE('',*,*,#5452,.F.);
#7217=ORIENTED_EDGE('',*,*,#5453,.F.);
#7218=ORIENTED_EDGE('',*,*,#5454,.F.);
#7219=ORIENTED_EDGE('',*,*,#5451,.F.);
#7220=ORIENTED_EDGE('',*,*,#5455,.T.);
#7221=ORIENTED_EDGE('',*,*,#5456,.F.);
#7222=ORIENTED_EDGE('',*,*,#5457,.F.);
#7223=ORIENTED_EDGE('',*,*,#5458,.T.);
#7224=ORIENTED_EDGE('',*,*,#5459,.F.);
#7225=ORIENTED_EDGE('',*,*,#5460,.F.);
#7226=ORIENTED_EDGE('',*,*,#5461,.F.);
#7227=ORIENTED_EDGE('',*,*,#5462,.F.);
#7228=ORIENTED_EDGE('',*,*,#5463,.F.);
#7229=ORIENTED_EDGE('',*,*,#5464,.T.);
#7230=ORIENTED_EDGE('',*,*,#5465,.F.);
#7231=ORIENTED_EDGE('',*,*,#5466,.T.);
#7232=ORIENTED_EDGE('',*,*,#5467,.F.);
#7233=ORIENTED_EDGE('',*,*,#5468,.F.);
#7234=ORIENTED_EDGE('',*,*,#5469,.F.);
#7235=ORIENTED_EDGE('',*,*,#5470,.F.);
#7236=ORIENTED_EDGE('',*,*,#5471,.F.);
#7237=ORIENTED_EDGE('',*,*,#5472,.T.);
#7238=ORIENTED_EDGE('',*,*,#5473,.F.);
#7239=ORIENTED_EDGE('',*,*,#5474,.F.);
#7240=ORIENTED_EDGE('',*,*,#5475,.T.);
#7241=ORIENTED_EDGE('',*,*,#5476,.F.);
#7242=ORIENTED_EDGE('',*,*,#5477,.T.);
#7243=ORIENTED_EDGE('',*,*,#5478,.F.);
#7244=ORIENTED_EDGE('',*,*,#5479,.F.);
#7245=ORIENTED_EDGE('',*,*,#5480,.F.);
#7246=ORIENTED_EDGE('',*,*,#5481,.T.);
#7247=ORIENTED_EDGE('',*,*,#5482,.F.);
#7248=ORIENTED_EDGE('',*,*,#5483,.T.);
#7249=ORIENTED_EDGE('',*,*,#5484,.F.);
#7250=ORIENTED_EDGE('',*,*,#5485,.F.);
#7251=ORIENTED_EDGE('',*,*,#5486,.T.);
#7252=ORIENTED_EDGE('',*,*,#5487,.F.);
#7253=ORIENTED_EDGE('',*,*,#5488,.T.);
#7254=ORIENTED_EDGE('',*,*,#5489,.F.);
#7255=ORIENTED_EDGE('',*,*,#5490,.T.);
#7256=ORIENTED_EDGE('',*,*,#5491,.T.);
#7257=ORIENTED_EDGE('',*,*,#5492,.T.);
#7258=ORIENTED_EDGE('',*,*,#5493,.T.);
#7259=ORIENTED_EDGE('',*,*,#5403,.T.);
#7260=ORIENTED_EDGE('',*,*,#5494,.T.);
#7261=ORIENTED_EDGE('',*,*,#5417,.T.);
#7262=ORIENTED_EDGE('',*,*,#5418,.T.);
#7263=ORIENTED_EDGE('',*,*,#5494,.F.);
#7264=ORIENTED_EDGE('',*,*,#5406,.T.);
#7265=ORIENTED_EDGE('',*,*,#5413,.T.);
#7266=ORIENTED_EDGE('',*,*,#5414,.T.);
#7267=ORIENTED_EDGE('',*,*,#5495,.T.);
#7268=ORIENTED_EDGE('',*,*,#5409,.T.);
#7269=ORIENTED_EDGE('',*,*,#5410,.T.);
#7270=ORIENTED_EDGE('',*,*,#5495,.F.);
#7271=ORIENTED_EDGE('',*,*,#5429,.T.);
#7272=ORIENTED_EDGE('',*,*,#5496,.F.);
#7273=ORIENTED_EDGE('',*,*,#5497,.T.);
#7274=ORIENTED_EDGE('',*,*,#5498,.F.);
#7275=ORIENTED_EDGE('',*,*,#5499,.T.);
#7276=ORIENTED_EDGE('',*,*,#5500,.F.);
#7277=ORIENTED_EDGE('',*,*,#5501,.T.);
#7278=ORIENTED_EDGE('',*,*,#5502,.F.);
#7279=ORIENTED_EDGE('',*,*,#5503,.T.);
#7280=ORIENTED_EDGE('',*,*,#5504,.T.);
#7281=ORIENTED_EDGE('',*,*,#5505,.T.);
#7282=ORIENTED_EDGE('',*,*,#5506,.T.);
#7283=ORIENTED_EDGE('',*,*,#5382,.T.);
#7284=ORIENTED_EDGE('',*,*,#5507,.T.);
#7285=ORIENTED_EDGE('',*,*,#5394,.T.);
#7286=ORIENTED_EDGE('',*,*,#5507,.F.);
#7287=ORIENTED_EDGE('',*,*,#5390,.T.);
#7288=ORIENTED_EDGE('',*,*,#5391,.T.);
#7289=ORIENTED_EDGE('',*,*,#5508,.T.);
#7290=ORIENTED_EDGE('',*,*,#5387,.T.);
#7291=ORIENTED_EDGE('',*,*,#5508,.F.);
#7292=ORIENTED_EDGE('',*,*,#5421,.T.);
#7293=ORIENTED_EDGE('',*,*,#5509,.T.);
#7294=ORIENTED_EDGE('',*,*,#5510,.T.);
#7295=ORIENTED_EDGE('',*,*,#5511,.T.);
#7296=ORIENTED_EDGE('',*,*,#5512,.T.);
#7297=ORIENTED_EDGE('',*,*,#5513,.T.);
#7298=ORIENTED_EDGE('',*,*,#5514,.T.);
#7299=ORIENTED_EDGE('',*,*,#5433,.T.);
#7300=ORIENTED_EDGE('',*,*,#5515,.F.);
#7301=ORIENTED_EDGE('',*,*,#5516,.T.);
#7302=ORIENTED_EDGE('',*,*,#5517,.F.);
#7303=ORIENTED_EDGE('',*,*,#5518,.T.);
#7304=ORIENTED_EDGE('',*,*,#5519,.F.);
#7305=ORIENTED_EDGE('',*,*,#5520,.T.);
#7306=ORIENTED_EDGE('',*,*,#5521,.F.);
#7307=ORIENTED_EDGE('',*,*,#5370,.T.);
#7308=ORIENTED_EDGE('',*,*,#5522,.T.);
#7309=ORIENTED_EDGE('',*,*,#5378,.T.);
#7310=ORIENTED_EDGE('',*,*,#5523,.T.);
#7311=ORIENTED_EDGE('',*,*,#5350,.T.);
#7312=ORIENTED_EDGE('',*,*,#5351,.T.);
#7313=ORIENTED_EDGE('',*,*,#5524,.T.);
#7314=ORIENTED_EDGE('',*,*,#5364,.T.);
#7315=ORIENTED_EDGE('',*,*,#5365,.T.);
#7316=ORIENTED_EDGE('',*,*,#5524,.F.);
#7317=ORIENTED_EDGE('',*,*,#5361,.T.);
#7318=ORIENTED_EDGE('',*,*,#5525,.T.);
#7319=ORIENTED_EDGE('',*,*,#5356,.T.);
#7320=ORIENTED_EDGE('',*,*,#5357,.T.);
#7321=ORIENTED_EDGE('',*,*,#5525,.F.);
#7322=ORIENTED_EDGE('',*,*,#5360,.T.);
#7323=ORIENTED_EDGE('',*,*,#5526,.T.);
#7324=ORIENTED_EDGE('',*,*,#5527,.T.);
#7325=ORIENTED_EDGE('',*,*,#5528,.T.);
#7326=ORIENTED_EDGE('',*,*,#5529,.T.);
#7327=ORIENTED_EDGE('',*,*,#5530,.T.);
#7328=ORIENTED_EDGE('',*,*,#5531,.T.);
#7329=ORIENTED_EDGE('',*,*,#5532,.T.);
#7330=ORIENTED_EDGE('',*,*,#5533,.T.);
#7331=ORIENTED_EDGE('',*,*,#5534,.F.);
#7332=ORIENTED_EDGE('',*,*,#5441,.T.);
#7333=ORIENTED_EDGE('',*,*,#5535,.F.);
#7334=ORIENTED_EDGE('',*,*,#5336,.T.);
#7335=ORIENTED_EDGE('',*,*,#5536,.F.);
#7336=ORIENTED_EDGE('',*,*,#5344,.T.);
#7337=ORIENTED_EDGE('',*,*,#5537,.F.);
#7338=ORIENTED_EDGE('',*,*,#5338,.T.);
#7339=ORIENTED_EDGE('',*,*,#5538,.T.);
#7340=ORIENTED_EDGE('',*,*,#5346,.T.);
#7341=ORIENTED_EDGE('',*,*,#5539,.T.);
#7342=ORIENTED_EDGE('',*,*,#5540,.F.);
#7343=ORIENTED_EDGE('',*,*,#5541,.T.);
#7344=ORIENTED_EDGE('',*,*,#5542,.F.);
#7345=ORIENTED_EDGE('',*,*,#5543,.F.);
#7346=ORIENTED_EDGE('',*,*,#5544,.T.);
#7347=ORIENTED_EDGE('',*,*,#5545,.F.);
#7348=ORIENTED_EDGE('',*,*,#5546,.T.);
#7349=ORIENTED_EDGE('',*,*,#5547,.F.);
#7350=ORIENTED_EDGE('',*,*,#5548,.T.);
#7351=ORIENTED_EDGE('',*,*,#5549,.F.);
#7352=ORIENTED_EDGE('',*,*,#5550,.T.);
#7353=ORIENTED_EDGE('',*,*,#5551,.T.);
#7354=ORIENTED_EDGE('',*,*,#5552,.T.);
#7355=ORIENTED_EDGE('',*,*,#5553,.F.);
#7356=ORIENTED_EDGE('',*,*,#5554,.T.);
#7357=ORIENTED_EDGE('',*,*,#5555,.F.);
#7358=ORIENTED_EDGE('',*,*,#5556,.T.);
#7359=ORIENTED_EDGE('',*,*,#5557,.T.);
#7360=ORIENTED_EDGE('',*,*,#5459,.T.);
#7361=ORIENTED_EDGE('',*,*,#5558,.T.);
#7362=ORIENTED_EDGE('',*,*,#5559,.T.);
#7363=ORIENTED_EDGE('',*,*,#5560,.F.);
#7364=ORIENTED_EDGE('',*,*,#5561,.F.);
#7365=ORIENTED_EDGE('',*,*,#5562,.T.);
#7366=ORIENTED_EDGE('',*,*,#5563,.F.);
#7367=ORIENTED_EDGE('',*,*,#5564,.T.);
#7368=ORIENTED_EDGE('',*,*,#5565,.T.);
#7369=ORIENTED_EDGE('',*,*,#5463,.T.);
#7370=ORIENTED_EDGE('',*,*,#5566,.F.);
#7371=ORIENTED_EDGE('',*,*,#5567,.T.);
#7372=ORIENTED_EDGE('',*,*,#5568,.F.);
#7373=ORIENTED_EDGE('',*,*,#5569,.T.);
#7374=ORIENTED_EDGE('',*,*,#5570,.T.);
#7375=ORIENTED_EDGE('',*,*,#5571,.T.);
#7376=ORIENTED_EDGE('',*,*,#5572,.T.);
#7377=ORIENTED_EDGE('',*,*,#5573,.T.);
#7378=ORIENTED_EDGE('',*,*,#5574,.F.);
#7379=ORIENTED_EDGE('',*,*,#5575,.F.);
#7380=ORIENTED_EDGE('',*,*,#5576,.T.);
#7381=ORIENTED_EDGE('',*,*,#5577,.F.);
#7382=ORIENTED_EDGE('',*,*,#5578,.T.);
#7383=ORIENTED_EDGE('',*,*,#5579,.T.);
#7384=ORIENTED_EDGE('',*,*,#5580,.T.);
#7385=ORIENTED_EDGE('',*,*,#5581,.F.);
#7386=ORIENTED_EDGE('',*,*,#5582,.T.);
#7387=ORIENTED_EDGE('',*,*,#5583,.F.);
#7388=ORIENTED_EDGE('',*,*,#5473,.T.);
#7389=ORIENTED_EDGE('',*,*,#5584,.T.);
#7390=ORIENTED_EDGE('',*,*,#5585,.T.);
#7391=ORIENTED_EDGE('',*,*,#5586,.T.);
#7392=ORIENTED_EDGE('',*,*,#5587,.T.);
#7393=ORIENTED_EDGE('',*,*,#5588,.F.);
#7394=ORIENTED_EDGE('',*,*,#5589,.F.);
#7395=ORIENTED_EDGE('',*,*,#5590,.T.);
#7396=ORIENTED_EDGE('',*,*,#5591,.F.);
#7397=ORIENTED_EDGE('',*,*,#5469,.T.);
#7398=ORIENTED_EDGE('',*,*,#5592,.T.);
#7399=ORIENTED_EDGE('',*,*,#5593,.T.);
#7400=ORIENTED_EDGE('',*,*,#5594,.F.);
#7401=ORIENTED_EDGE('',*,*,#5595,.T.);
#7402=ORIENTED_EDGE('',*,*,#5596,.F.);
#7403=ORIENTED_EDGE('',*,*,#5597,.T.);
#7404=ORIENTED_EDGE('',*,*,#5598,.T.);
#7405=ORIENTED_EDGE('',*,*,#5599,.T.);
#7406=ORIENTED_EDGE('',*,*,#5600,.T.);
#7407=ORIENTED_EDGE('',*,*,#5601,.T.);
#7408=ORIENTED_EDGE('',*,*,#5602,.F.);
#7409=ORIENTED_EDGE('',*,*,#5546,.F.);
#7410=ORIENTED_EDGE('',*,*,#5603,.F.);
#7411=ORIENTED_EDGE('',*,*,#5604,.T.);
#7412=ORIENTED_EDGE('',*,*,#5605,.F.);
#7413=ORIENTED_EDGE('',*,*,#5606,.F.);
#7414=ORIENTED_EDGE('',*,*,#5607,.T.);
#7415=ORIENTED_EDGE('',*,*,#5608,.F.);
#7416=ORIENTED_EDGE('',*,*,#5319,.T.);
#7417=ORIENTED_EDGE('',*,*,#5320,.T.);
#7418=ORIENTED_EDGE('',*,*,#5609,.T.);
#7419=ORIENTED_EDGE('',*,*,#5332,.T.);
#7420=ORIENTED_EDGE('',*,*,#5333,.T.);
#7421=ORIENTED_EDGE('',*,*,#5609,.F.);
#7422=ORIENTED_EDGE('',*,*,#5329,.T.);
#7423=ORIENTED_EDGE('',*,*,#5610,.T.);
#7424=ORIENTED_EDGE('',*,*,#5325,.T.);
#7425=ORIENTED_EDGE('',*,*,#5326,.T.);
#7426=ORIENTED_EDGE('',*,*,#5610,.F.);
#7427=ORIENTED_EDGE('',*,*,#5611,.T.);
#7428=ORIENTED_EDGE('',*,*,#5612,.T.);
#7429=ORIENTED_EDGE('',*,*,#5613,.T.);
#7430=ORIENTED_EDGE('',*,*,#5614,.T.);
#7431=ORIENTED_EDGE('',*,*,#5615,.T.);
#7432=ORIENTED_EDGE('',*,*,#5616,.T.);
#7433=ORIENTED_EDGE('',*,*,#5617,.T.);
#7434=ORIENTED_EDGE('',*,*,#5618,.T.);
#7435=ORIENTED_EDGE('',*,*,#5619,.F.);
#7436=ORIENTED_EDGE('',*,*,#5437,.T.);
#7437=ORIENTED_EDGE('',*,*,#5620,.F.);
#7438=ORIENTED_EDGE('',*,*,#5621,.F.);
#7439=ORIENTED_EDGE('',*,*,#5622,.T.);
#7440=ORIENTED_EDGE('',*,*,#5623,.T.);
#7441=ORIENTED_EDGE('',*,*,#5624,.F.);
#7442=ORIENTED_EDGE('',*,*,#5625,.T.);
#7443=ORIENTED_EDGE('',*,*,#5626,.F.);
#7444=ORIENTED_EDGE('',*,*,#5627,.F.);
#7445=ORIENTED_EDGE('',*,*,#5628,.T.);
#7446=ORIENTED_EDGE('',*,*,#5399,.T.);
#7447=ORIENTED_EDGE('',*,*,#5629,.T.);
#7448=ORIENTED_EDGE('',*,*,#5630,.T.);
#7449=ORIENTED_EDGE('',*,*,#5631,.T.);
#7450=ORIENTED_EDGE('',*,*,#5632,.T.);
#7451=ORIENTED_EDGE('',*,*,#5633,.T.);
#7452=ORIENTED_EDGE('',*,*,#5634,.T.);
#7453=ORIENTED_EDGE('',*,*,#5635,.T.);
#7454=ORIENTED_EDGE('',*,*,#5636,.F.);
#7455=ORIENTED_EDGE('',*,*,#5637,.T.);
#7456=ORIENTED_EDGE('',*,*,#5638,.T.);
#7457=ORIENTED_EDGE('',*,*,#5639,.T.);
#7458=ORIENTED_EDGE('',*,*,#5640,.T.);
#7459=ORIENTED_EDGE('',*,*,#5641,.T.);
#7460=ORIENTED_EDGE('',*,*,#5642,.T.);
#7461=ORIENTED_EDGE('',*,*,#5643,.T.);
#7462=ORIENTED_EDGE('',*,*,#5644,.T.);
#7463=ORIENTED_EDGE('',*,*,#5645,.T.);
#7464=ORIENTED_EDGE('',*,*,#5405,.T.);
#7465=ORIENTED_EDGE('',*,*,#5646,.T.);
#7466=ORIENTED_EDGE('',*,*,#5647,.T.);
#7467=ORIENTED_EDGE('',*,*,#5648,.T.);
#7468=ORIENTED_EDGE('',*,*,#5649,.T.);
#7469=ORIENTED_EDGE('',*,*,#5650,.T.);
#7470=ORIENTED_EDGE('',*,*,#5482,.T.);
#7471=ORIENTED_EDGE('',*,*,#5651,.T.);
#7472=ORIENTED_EDGE('',*,*,#5652,.T.);
#7473=ORIENTED_EDGE('',*,*,#5384,.T.);
#7474=ORIENTED_EDGE('',*,*,#5353,.T.);
#7475=ORIENTED_EDGE('',*,*,#5653,.T.);
#7476=ORIENTED_EDGE('',*,*,#5654,.T.);
#7477=ORIENTED_EDGE('',*,*,#5655,.T.);
#7478=ORIENTED_EDGE('',*,*,#5656,.T.);
#7479=ORIENTED_EDGE('',*,*,#5380,.T.);
#7480=ORIENTED_EDGE('',*,*,#5657,.T.);
#7481=ORIENTED_EDGE('',*,*,#5658,.T.);
#7482=ORIENTED_EDGE('',*,*,#5374,.T.);
#7483=ORIENTED_EDGE('',*,*,#5659,.T.);
#7484=ORIENTED_EDGE('',*,*,#5342,.T.);
#7485=ORIENTED_EDGE('',*,*,#5660,.T.);
#7486=ORIENTED_EDGE('',*,*,#5661,.T.);
#7487=ORIENTED_EDGE('',*,*,#5348,.T.);
#7488=ORIENTED_EDGE('',*,*,#5662,.T.);
#7489=ORIENTED_EDGE('',*,*,#5663,.T.);
#7490=ORIENTED_EDGE('',*,*,#5664,.T.);
#7491=ORIENTED_EDGE('',*,*,#5322,.T.);
#7492=ORIENTED_EDGE('',*,*,#5665,.F.);
#7493=ORIENTED_EDGE('',*,*,#5666,.T.);
#7494=ORIENTED_EDGE('',*,*,#5667,.F.);
#7495=ORIENTED_EDGE('',*,*,#5668,.T.);
#7496=ORIENTED_EDGE('',*,*,#5669,.F.);
#7497=ORIENTED_EDGE('',*,*,#5670,.T.);
#7498=ORIENTED_EDGE('',*,*,#5671,.F.);
#7499=ORIENTED_EDGE('',*,*,#5672,.T.);
#7500=ORIENTED_EDGE('',*,*,#5673,.F.);
#7501=ORIENTED_EDGE('',*,*,#5674,.T.);
#7502=ORIENTED_EDGE('',*,*,#5675,.F.);
#7503=ORIENTED_EDGE('',*,*,#5676,.T.);
#7504=ORIENTED_EDGE('',*,*,#5677,.F.);
#7505=ORIENTED_EDGE('',*,*,#5678,.T.);
#7506=ORIENTED_EDGE('',*,*,#5679,.F.);
#7507=ORIENTED_EDGE('',*,*,#5680,.T.);
#7508=ORIENTED_EDGE('',*,*,#5681,.F.);
#7509=ORIENTED_EDGE('',*,*,#5682,.T.);
#7510=ORIENTED_EDGE('',*,*,#5683,.T.);
#7511=ORIENTED_EDGE('',*,*,#5684,.T.);
#7512=ORIENTED_EDGE('',*,*,#5685,.F.);
#7513=ORIENTED_EDGE('',*,*,#5686,.T.);
#7514=ORIENTED_EDGE('',*,*,#5687,.T.);
#7515=ORIENTED_EDGE('',*,*,#5688,.T.);
#7516=ORIENTED_EDGE('',*,*,#5689,.T.);
#7517=ORIENTED_EDGE('',*,*,#5690,.F.);
#7518=ORIENTED_EDGE('',*,*,#5691,.F.);
#7519=ORIENTED_EDGE('',*,*,#5692,.F.);
#7520=ORIENTED_EDGE('',*,*,#5693,.F.);
#7521=ORIENTED_EDGE('',*,*,#5694,.T.);
#7522=ORIENTED_EDGE('',*,*,#5695,.T.);
#7523=ORIENTED_EDGE('',*,*,#5696,.T.);
#7524=ORIENTED_EDGE('',*,*,#5697,.T.);
#7525=ORIENTED_EDGE('',*,*,#5698,.T.);
#7526=ORIENTED_EDGE('',*,*,#5699,.T.);
#7527=ORIENTED_EDGE('',*,*,#5700,.T.);
#7528=ORIENTED_EDGE('',*,*,#5701,.T.);
#7529=ORIENTED_EDGE('',*,*,#5702,.T.);
#7530=ORIENTED_EDGE('',*,*,#5703,.T.);
#7531=ORIENTED_EDGE('',*,*,#5704,.F.);
#7532=ORIENTED_EDGE('',*,*,#5705,.F.);
#7533=ORIENTED_EDGE('',*,*,#5706,.F.);
#7534=ORIENTED_EDGE('',*,*,#5388,.T.);
#7535=ORIENTED_EDGE('',*,*,#5707,.F.);
#7536=ORIENTED_EDGE('',*,*,#5708,.T.);
#7537=ORIENTED_EDGE('',*,*,#5709,.T.);
#7538=ORIENTED_EDGE('',*,*,#5710,.T.);
#7539=ORIENTED_EDGE('',*,*,#5711,.T.);
#7540=ORIENTED_EDGE('',*,*,#5712,.T.);
#7541=ORIENTED_EDGE('',*,*,#5431,.T.);
#7542=ORIENTED_EDGE('',*,*,#5713,.T.);
#7543=ORIENTED_EDGE('',*,*,#5714,.T.);
#7544=ORIENTED_EDGE('',*,*,#5715,.T.);
#7545=ORIENTED_EDGE('',*,*,#5716,.T.);
#7546=ORIENTED_EDGE('',*,*,#5717,.F.);
#7547=ORIENTED_EDGE('',*,*,#5718,.T.);
#7548=ORIENTED_EDGE('',*,*,#5719,.T.);
#7549=ORIENTED_EDGE('',*,*,#5720,.F.);
#7550=ORIENTED_EDGE('',*,*,#5721,.F.);
#7551=ORIENTED_EDGE('',*,*,#5392,.T.);
#7552=ORIENTED_EDGE('',*,*,#5722,.F.);
#7553=ORIENTED_EDGE('',*,*,#5723,.T.);
#7554=ORIENTED_EDGE('',*,*,#5724,.T.);
#7555=ORIENTED_EDGE('',*,*,#5725,.T.);
#7556=ORIENTED_EDGE('',*,*,#5708,.F.);
#7557=ORIENTED_EDGE('',*,*,#5726,.T.);
#7558=ORIENTED_EDGE('',*,*,#5688,.F.);
#7559=ORIENTED_EDGE('',*,*,#5727,.F.);
#7560=ORIENTED_EDGE('',*,*,#5682,.F.);
#7561=ORIENTED_EDGE('',*,*,#5728,.T.);
#7562=ORIENTED_EDGE('',*,*,#5703,.F.);
#7563=ORIENTED_EDGE('',*,*,#5729,.F.);
#7564=ORIENTED_EDGE('',*,*,#5730,.F.);
#7565=ORIENTED_EDGE('',*,*,#5731,.T.);
#7566=ORIENTED_EDGE('',*,*,#5684,.F.);
#7567=ORIENTED_EDGE('',*,*,#5732,.F.);
#7568=ORIENTED_EDGE('',*,*,#5686,.F.);
#7569=ORIENTED_EDGE('',*,*,#5733,.T.);
#7570=ORIENTED_EDGE('',*,*,#5625,.F.);
#7571=ORIENTED_EDGE('',*,*,#5734,.F.);
#7572=ORIENTED_EDGE('',*,*,#5628,.F.);
#7573=ORIENTED_EDGE('',*,*,#5735,.T.);
#7574=ORIENTED_EDGE('',*,*,#5725,.F.);
#7575=ORIENTED_EDGE('',*,*,#5400,.T.);
#7576=ORIENTED_EDGE('',*,*,#5736,.F.);
#7577=ORIENTED_EDGE('',*,*,#5737,.F.);
#7578=ORIENTED_EDGE('',*,*,#5398,.T.);
#7579=ORIENTED_EDGE('',*,*,#5723,.F.);
#7580=ORIENTED_EDGE('',*,*,#5738,.T.);
#7581=ORIENTED_EDGE('',*,*,#5739,.T.);
#7582=ORIENTED_EDGE('',*,*,#5740,.T.);
#7583=ORIENTED_EDGE('',*,*,#5741,.T.);
#7584=ORIENTED_EDGE('',*,*,#5742,.F.);
#7585=ORIENTED_EDGE('',*,*,#5743,.F.);
#7586=ORIENTED_EDGE('',*,*,#5744,.F.);
#7587=ORIENTED_EDGE('',*,*,#5740,.F.);
#7588=ORIENTED_EDGE('',*,*,#5745,.F.);
#7589=ORIENTED_EDGE('',*,*,#5738,.F.);
#7590=ORIENTED_EDGE('',*,*,#5746,.T.);
#7591=ORIENTED_EDGE('',*,*,#5747,.F.);
#7592=ORIENTED_EDGE('',*,*,#5748,.T.);
#7593=ORIENTED_EDGE('',*,*,#5749,.T.);
#7594=ORIENTED_EDGE('',*,*,#5750,.T.);
#7595=ORIENTED_EDGE('',*,*,#5751,.F.);
#7596=ORIENTED_EDGE('',*,*,#5752,.F.);
#7597=ORIENTED_EDGE('',*,*,#5315,.F.);
#7598=ORIENTED_EDGE('',*,*,#5753,.F.);
#7599=ORIENTED_EDGE('',*,*,#5754,.F.);
#7600=ORIENTED_EDGE('',*,*,#5755,.T.);
#7601=ORIENTED_EDGE('',*,*,#5756,.T.);
#7602=ORIENTED_EDGE('',*,*,#5757,.T.);
#7603=ORIENTED_EDGE('',*,*,#5758,.F.);
#7604=ORIENTED_EDGE('',*,*,#5759,.F.);
#7605=ORIENTED_EDGE('',*,*,#5760,.T.);
#7606=ORIENTED_EDGE('',*,*,#5761,.T.);
#7607=ORIENTED_EDGE('',*,*,#5762,.T.);
#7608=ORIENTED_EDGE('',*,*,#5763,.F.);
#7609=ORIENTED_EDGE('',*,*,#5764,.F.);
#7610=ORIENTED_EDGE('',*,*,#5765,.T.);
#7611=ORIENTED_EDGE('',*,*,#5766,.T.);
#7612=ORIENTED_EDGE('',*,*,#5767,.T.);
#7613=ORIENTED_EDGE('',*,*,#5768,.F.);
#7614=ORIENTED_EDGE('',*,*,#5769,.F.);
#7615=ORIENTED_EDGE('',*,*,#5770,.T.);
#7616=ORIENTED_EDGE('',*,*,#5771,.T.);
#7617=ORIENTED_EDGE('',*,*,#5772,.T.);
#7618=ORIENTED_EDGE('',*,*,#5773,.T.);
#7619=ORIENTED_EDGE('',*,*,#5774,.T.);
#7620=ORIENTED_EDGE('',*,*,#5775,.T.);
#7621=ORIENTED_EDGE('',*,*,#5776,.T.);
#7622=ORIENTED_EDGE('',*,*,#5777,.T.);
#7623=ORIENTED_EDGE('',*,*,#5778,.T.);
#7624=ORIENTED_EDGE('',*,*,#5779,.T.);
#7625=ORIENTED_EDGE('',*,*,#5780,.F.);
#7626=ORIENTED_EDGE('',*,*,#5781,.F.);
#7627=ORIENTED_EDGE('',*,*,#5747,.T.);
#7628=ORIENTED_EDGE('',*,*,#5782,.T.);
#7629=ORIENTED_EDGE('',*,*,#5783,.T.);
#7630=ORIENTED_EDGE('',*,*,#5784,.T.);
#7631=ORIENTED_EDGE('',*,*,#5785,.T.);
#7632=ORIENTED_EDGE('',*,*,#5786,.T.);
#7633=ORIENTED_EDGE('',*,*,#5787,.T.);
#7634=ORIENTED_EDGE('',*,*,#5788,.T.);
#7635=ORIENTED_EDGE('',*,*,#5789,.T.);
#7636=ORIENTED_EDGE('',*,*,#5790,.T.);
#7637=ORIENTED_EDGE('',*,*,#5791,.T.);
#7638=ORIENTED_EDGE('',*,*,#5792,.T.);
#7639=ORIENTED_EDGE('',*,*,#5793,.T.);
#7640=ORIENTED_EDGE('',*,*,#5794,.T.);
#7641=ORIENTED_EDGE('',*,*,#5795,.T.);
#7642=ORIENTED_EDGE('',*,*,#5796,.T.);
#7643=ORIENTED_EDGE('',*,*,#5456,.T.);
#7644=ORIENTED_EDGE('',*,*,#5797,.T.);
#7645=ORIENTED_EDGE('',*,*,#5798,.T.);
#7646=ORIENTED_EDGE('',*,*,#5799,.T.);
#7647=ORIENTED_EDGE('',*,*,#5800,.T.);
#7648=ORIENTED_EDGE('',*,*,#5801,.F.);
#7649=ORIENTED_EDGE('',*,*,#5623,.F.);
#7650=ORIENTED_EDGE('',*,*,#5802,.T.);
#7651=ORIENTED_EDGE('',*,*,#5803,.F.);
#7652=ORIENTED_EDGE('',*,*,#5804,.T.);
#7653=ORIENTED_EDGE('',*,*,#5805,.T.);
#7654=ORIENTED_EDGE('',*,*,#5806,.T.);
#7655=ORIENTED_EDGE('',*,*,#5465,.T.);
#7656=ORIENTED_EDGE('',*,*,#5807,.F.);
#7657=ORIENTED_EDGE('',*,*,#5808,.T.);
#7658=ORIENTED_EDGE('',*,*,#5809,.T.);
#7659=ORIENTED_EDGE('',*,*,#5810,.T.);
#7660=ORIENTED_EDGE('',*,*,#5811,.T.);
#7661=ORIENTED_EDGE('',*,*,#5812,.T.);
#7662=ORIENTED_EDGE('',*,*,#5813,.T.);
#7663=ORIENTED_EDGE('',*,*,#5814,.T.);
#7664=ORIENTED_EDGE('',*,*,#5815,.T.);
#7665=ORIENTED_EDGE('',*,*,#5816,.T.);
#7666=ORIENTED_EDGE('',*,*,#5817,.F.);
#7667=ORIENTED_EDGE('',*,*,#5818,.T.);
#7668=ORIENTED_EDGE('',*,*,#5819,.T.);
#7669=ORIENTED_EDGE('',*,*,#5820,.F.);
#7670=ORIENTED_EDGE('',*,*,#5821,.T.);
#7671=ORIENTED_EDGE('',*,*,#5822,.T.);
#7672=ORIENTED_EDGE('',*,*,#5823,.T.);
#7673=ORIENTED_EDGE('',*,*,#5824,.T.);
#7674=ORIENTED_EDGE('',*,*,#5825,.T.);
#7675=ORIENTED_EDGE('',*,*,#5826,.T.);
#7676=ORIENTED_EDGE('',*,*,#5827,.T.);
#7677=ORIENTED_EDGE('',*,*,#5828,.T.);
#7678=ORIENTED_EDGE('',*,*,#5829,.T.);
#7679=ORIENTED_EDGE('',*,*,#5830,.T.);
#7680=ORIENTED_EDGE('',*,*,#5831,.T.);
#7681=ORIENTED_EDGE('',*,*,#5832,.T.);
#7682=ORIENTED_EDGE('',*,*,#5833,.T.);
#7683=ORIENTED_EDGE('',*,*,#5834,.T.);
#7684=ORIENTED_EDGE('',*,*,#5446,.T.);
#7685=ORIENTED_EDGE('',*,*,#5835,.T.);
#7686=ORIENTED_EDGE('',*,*,#5448,.T.);
#7687=ORIENTED_EDGE('',*,*,#5836,.T.);
#7688=ORIENTED_EDGE('',*,*,#5837,.T.);
#7689=ORIENTED_EDGE('',*,*,#5838,.T.);
#7690=ORIENTED_EDGE('',*,*,#5839,.T.);
#7691=ORIENTED_EDGE('',*,*,#5840,.T.);
#7692=ORIENTED_EDGE('',*,*,#5841,.T.);
#7693=ORIENTED_EDGE('',*,*,#5842,.T.);
#7694=ORIENTED_EDGE('',*,*,#5843,.T.);
#7695=ORIENTED_EDGE('',*,*,#5844,.T.);
#7696=ORIENTED_EDGE('',*,*,#5845,.T.);
#7697=ORIENTED_EDGE('',*,*,#5846,.T.);
#7698=ORIENTED_EDGE('',*,*,#5847,.T.);
#7699=ORIENTED_EDGE('',*,*,#5848,.T.);
#7700=ORIENTED_EDGE('',*,*,#5849,.T.);
#7701=ORIENTED_EDGE('',*,*,#5850,.T.);
#7702=ORIENTED_EDGE('',*,*,#5851,.T.);
#7703=ORIENTED_EDGE('',*,*,#5852,.T.);
#7704=ORIENTED_EDGE('',*,*,#5853,.T.);
#7705=ORIENTED_EDGE('',*,*,#5435,.T.);
#7706=ORIENTED_EDGE('',*,*,#5854,.T.);
#7707=ORIENTED_EDGE('',*,*,#5855,.T.);
#7708=ORIENTED_EDGE('',*,*,#5327,.T.);
#7709=ORIENTED_EDGE('',*,*,#5856,.T.);
#7710=ORIENTED_EDGE('',*,*,#5857,.T.);
#7711=ORIENTED_EDGE('',*,*,#5858,.T.);
#7712=ORIENTED_EDGE('',*,*,#5859,.T.);
#7713=ORIENTED_EDGE('',*,*,#5860,.T.);
#7714=ORIENTED_EDGE('',*,*,#5861,.T.);
#7715=ORIENTED_EDGE('',*,*,#5862,.T.);
#7716=ORIENTED_EDGE('',*,*,#5863,.T.);
#7717=ORIENTED_EDGE('',*,*,#5330,.T.);
#7718=ORIENTED_EDGE('',*,*,#5864,.F.);
#7719=ORIENTED_EDGE('',*,*,#5865,.T.);
#7720=ORIENTED_EDGE('',*,*,#5866,.T.);
#7721=ORIENTED_EDGE('',*,*,#5867,.T.);
#7722=ORIENTED_EDGE('',*,*,#5868,.F.);
#7723=ORIENTED_EDGE('',*,*,#5869,.T.);
#7724=ORIENTED_EDGE('',*,*,#5870,.F.);
#7725=ORIENTED_EDGE('',*,*,#5871,.T.);
#7726=ORIENTED_EDGE('',*,*,#5872,.F.);
#7727=ORIENTED_EDGE('',*,*,#5873,.T.);
#7728=ORIENTED_EDGE('',*,*,#5874,.F.);
#7729=ORIENTED_EDGE('',*,*,#5875,.T.);
#7730=ORIENTED_EDGE('',*,*,#5876,.F.);
#7731=ORIENTED_EDGE('',*,*,#5877,.T.);
#7732=ORIENTED_EDGE('',*,*,#5878,.T.);
#7733=ORIENTED_EDGE('',*,*,#5879,.T.);
#7734=ORIENTED_EDGE('',*,*,#5878,.F.);
#7735=ORIENTED_EDGE('',*,*,#5880,.T.);
#7736=ORIENTED_EDGE('',*,*,#5868,.T.);
#7737=ORIENTED_EDGE('',*,*,#5881,.T.);
#7738=ORIENTED_EDGE('',*,*,#5882,.T.);
#7739=ORIENTED_EDGE('',*,*,#5883,.T.);
#7740=ORIENTED_EDGE('',*,*,#5884,.F.);
#7741=ORIENTED_EDGE('',*,*,#5885,.T.);
#7742=ORIENTED_EDGE('',*,*,#5886,.F.);
#7743=ORIENTED_EDGE('',*,*,#5887,.T.);
#7744=ORIENTED_EDGE('',*,*,#5888,.F.);
#7745=ORIENTED_EDGE('',*,*,#5889,.T.);
#7746=ORIENTED_EDGE('',*,*,#5890,.F.);
#7747=ORIENTED_EDGE('',*,*,#5891,.T.);
#7748=ORIENTED_EDGE('',*,*,#5892,.F.);
#7749=ORIENTED_EDGE('',*,*,#5893,.T.);
#7750=ORIENTED_EDGE('',*,*,#5894,.T.);
#7751=ORIENTED_EDGE('',*,*,#5895,.T.);
#7752=ORIENTED_EDGE('',*,*,#5896,.F.);
#7753=ORIENTED_EDGE('',*,*,#5897,.T.);
#7754=ORIENTED_EDGE('',*,*,#5898,.T.);
#7755=ORIENTED_EDGE('',*,*,#5899,.F.);
#7756=ORIENTED_EDGE('',*,*,#5900,.F.);
#7757=ORIENTED_EDGE('',*,*,#5901,.F.);
#7758=ORIENTED_EDGE('',*,*,#5902,.T.);
#7759=ORIENTED_EDGE('',*,*,#5903,.T.);
#7760=ORIENTED_EDGE('',*,*,#5904,.F.);
#7761=ORIENTED_EDGE('',*,*,#5905,.T.);
#7762=ORIENTED_EDGE('',*,*,#5906,.F.);
#7763=ORIENTED_EDGE('',*,*,#5907,.T.);
#7764=ORIENTED_EDGE('',*,*,#5908,.F.);
#7765=ORIENTED_EDGE('',*,*,#5909,.T.);
#7766=ORIENTED_EDGE('',*,*,#5910,.T.);
#7767=ORIENTED_EDGE('',*,*,#5911,.T.);
#7768=ORIENTED_EDGE('',*,*,#5912,.T.);
#7769=ORIENTED_EDGE('',*,*,#5913,.T.);
#7770=ORIENTED_EDGE('',*,*,#5743,.T.);
#7771=ORIENTED_EDGE('',*,*,#5914,.T.);
#7772=ORIENTED_EDGE('',*,*,#5915,.T.);
#7773=ORIENTED_EDGE('',*,*,#5916,.F.);
#7774=ORIENTED_EDGE('',*,*,#5917,.T.);
#7775=ORIENTED_EDGE('',*,*,#5918,.T.);
#7776=ORIENTED_EDGE('',*,*,#5919,.T.);
#7777=ORIENTED_EDGE('',*,*,#5730,.T.);
#7778=ORIENTED_EDGE('',*,*,#5920,.T.);
#7779=ORIENTED_EDGE('',*,*,#5921,.T.);
#7780=ORIENTED_EDGE('',*,*,#5922,.T.);
#7781=ORIENTED_EDGE('',*,*,#5923,.T.);
#7782=ORIENTED_EDGE('',*,*,#5924,.T.);
#7783=ORIENTED_EDGE('',*,*,#5925,.T.);
#7784=ORIENTED_EDGE('',*,*,#5926,.T.);
#7785=ORIENTED_EDGE('',*,*,#5307,.T.);
#7786=ORIENTED_EDGE('',*,*,#5407,.T.);
#7787=ORIENTED_EDGE('',*,*,#5927,.T.);
#7788=ORIENTED_EDGE('',*,*,#5928,.T.);
#7789=ORIENTED_EDGE('',*,*,#5929,.T.);
#7790=ORIENTED_EDGE('',*,*,#5930,.T.);
#7791=ORIENTED_EDGE('',*,*,#5931,.T.);
#7792=ORIENTED_EDGE('',*,*,#5932,.T.);
#7793=ORIENTED_EDGE('',*,*,#5933,.F.);
#7794=ORIENTED_EDGE('',*,*,#5934,.T.);
#7795=ORIENTED_EDGE('',*,*,#5935,.F.);
#7796=ORIENTED_EDGE('',*,*,#5936,.T.);
#7797=ORIENTED_EDGE('',*,*,#5937,.F.);
#7798=ORIENTED_EDGE('',*,*,#5385,.T.);
#7799=ORIENTED_EDGE('',*,*,#5354,.T.);
#7800=ORIENTED_EDGE('',*,*,#5938,.T.);
#7801=ORIENTED_EDGE('',*,*,#5939,.T.);
#7802=ORIENTED_EDGE('',*,*,#5940,.T.);
#7803=ORIENTED_EDGE('',*,*,#5941,.T.);
#7804=ORIENTED_EDGE('',*,*,#5476,.T.);
#7805=ORIENTED_EDGE('',*,*,#5942,.T.);
#7806=ORIENTED_EDGE('',*,*,#5943,.F.);
#7807=ORIENTED_EDGE('',*,*,#5944,.T.);
#7808=ORIENTED_EDGE('',*,*,#5945,.F.);
#7809=ORIENTED_EDGE('',*,*,#5946,.T.);
#7810=ORIENTED_EDGE('',*,*,#5947,.F.);
#7811=ORIENTED_EDGE('',*,*,#5948,.T.);
#7812=ORIENTED_EDGE('',*,*,#5949,.T.);
#7813=ORIENTED_EDGE('',*,*,#5950,.T.);
#7814=ORIENTED_EDGE('',*,*,#5951,.F.);
#7815=ORIENTED_EDGE('',*,*,#5952,.T.);
#7816=ORIENTED_EDGE('',*,*,#5953,.F.);
#7817=ORIENTED_EDGE('',*,*,#5954,.T.);
#7818=ORIENTED_EDGE('',*,*,#5955,.F.);
#7819=ORIENTED_EDGE('',*,*,#5956,.T.);
#7820=ORIENTED_EDGE('',*,*,#5957,.T.);
#7821=ORIENTED_EDGE('',*,*,#5958,.T.);
#7822=ORIENTED_EDGE('',*,*,#5323,.T.);
#7823=ORIENTED_EDGE('',*,*,#5888,.T.);
#7824=ORIENTED_EDGE('',*,*,#5959,.T.);
#7825=ORIENTED_EDGE('',*,*,#5894,.F.);
#7826=ORIENTED_EDGE('',*,*,#5960,.T.);
#7827=ORIENTED_EDGE('',*,*,#5961,.T.);
#7828=ORIENTED_EDGE('',*,*,#5962,.T.);
#7829=ORIENTED_EDGE('',*,*,#5963,.T.);
#7830=ORIENTED_EDGE('',*,*,#5964,.T.);
#7831=ORIENTED_EDGE('',*,*,#5965,.F.);
#7832=ORIENTED_EDGE('',*,*,#5966,.T.);
#7833=ORIENTED_EDGE('',*,*,#5967,.T.);
#7834=ORIENTED_EDGE('',*,*,#5968,.T.);
#7835=ORIENTED_EDGE('',*,*,#5969,.F.);
#7836=ORIENTED_EDGE('',*,*,#5970,.F.);
#7837=ORIENTED_EDGE('',*,*,#5971,.T.);
#7838=ORIENTED_EDGE('',*,*,#5972,.T.);
#7839=ORIENTED_EDGE('',*,*,#5973,.T.);
#7840=ORIENTED_EDGE('',*,*,#5974,.F.);
#7841=ORIENTED_EDGE('',*,*,#5975,.T.);
#7842=ORIENTED_EDGE('',*,*,#5976,.T.);
#7843=ORIENTED_EDGE('',*,*,#5619,.T.);
#7844=ORIENTED_EDGE('',*,*,#5977,.T.);
#7845=ORIENTED_EDGE('',*,*,#5978,.T.);
#7846=ORIENTED_EDGE('',*,*,#5444,.T.);
#7847=ORIENTED_EDGE('',*,*,#5620,.T.);
#7848=ORIENTED_EDGE('',*,*,#5979,.T.);
#7849=ORIENTED_EDGE('',*,*,#5980,.T.);
#7850=ORIENTED_EDGE('',*,*,#5981,.T.);
#7851=ORIENTED_EDGE('',*,*,#5982,.T.);
#7852=ORIENTED_EDGE('',*,*,#5983,.T.);
#7853=ORIENTED_EDGE('',*,*,#5984,.T.);
#7854=ORIENTED_EDGE('',*,*,#5985,.T.);
#7855=ORIENTED_EDGE('',*,*,#5986,.F.);
#7856=ORIENTED_EDGE('',*,*,#5987,.T.);
#7857=ORIENTED_EDGE('',*,*,#5988,.T.);
#7858=ORIENTED_EDGE('',*,*,#5989,.T.);
#7859=ORIENTED_EDGE('',*,*,#5990,.T.);
#7860=ORIENTED_EDGE('',*,*,#5991,.T.);
#7861=ORIENTED_EDGE('',*,*,#5992,.T.);
#7862=ORIENTED_EDGE('',*,*,#5993,.T.);
#7863=ORIENTED_EDGE('',*,*,#5994,.T.);
#7864=ORIENTED_EDGE('',*,*,#5995,.T.);
#7865=ORIENTED_EDGE('',*,*,#5996,.T.);
#7866=ORIENTED_EDGE('',*,*,#5997,.T.);
#7867=ORIENTED_EDGE('',*,*,#5998,.T.);
#7868=ORIENTED_EDGE('',*,*,#5999,.T.);
#7869=ORIENTED_EDGE('',*,*,#6000,.T.);
#7870=ORIENTED_EDGE('',*,*,#6001,.T.);
#7871=ORIENTED_EDGE('',*,*,#5537,.T.);
#7872=ORIENTED_EDGE('',*,*,#6002,.T.);
#7873=ORIENTED_EDGE('',*,*,#6003,.T.);
#7874=ORIENTED_EDGE('',*,*,#6004,.T.);
#7875=ORIENTED_EDGE('',*,*,#6005,.T.);
#7876=ORIENTED_EDGE('',*,*,#6006,.T.);
#7877=ORIENTED_EDGE('',*,*,#5536,.T.);
#7878=ORIENTED_EDGE('',*,*,#6007,.T.);
#7879=ORIENTED_EDGE('',*,*,#6008,.T.);
#7880=ORIENTED_EDGE('',*,*,#6009,.T.);
#7881=ORIENTED_EDGE('',*,*,#6010,.T.);
#7882=ORIENTED_EDGE('',*,*,#6011,.T.);
#7883=ORIENTED_EDGE('',*,*,#5340,.T.);
#7884=ORIENTED_EDGE('',*,*,#6012,.T.);
#7885=ORIENTED_EDGE('',*,*,#6013,.T.);
#7886=ORIENTED_EDGE('',*,*,#5334,.T.);
#7887=ORIENTED_EDGE('',*,*,#6014,.T.);
#7888=ORIENTED_EDGE('',*,*,#6015,.T.);
#7889=ORIENTED_EDGE('',*,*,#6016,.T.);
#7890=ORIENTED_EDGE('',*,*,#6017,.T.);
#7891=ORIENTED_EDGE('',*,*,#6008,.F.);
#7892=ORIENTED_EDGE('',*,*,#6018,.T.);
#7893=ORIENTED_EDGE('',*,*,#6003,.F.);
#7894=ORIENTED_EDGE('',*,*,#6019,.T.);
#7895=ORIENTED_EDGE('',*,*,#6005,.F.);
#7896=ORIENTED_EDGE('',*,*,#6020,.T.);
#7897=ORIENTED_EDGE('',*,*,#5539,.F.);
#7898=ORIENTED_EDGE('',*,*,#6021,.T.);
#7899=ORIENTED_EDGE('',*,*,#5538,.F.);
#7900=ORIENTED_EDGE('',*,*,#6022,.T.);
#7901=ORIENTED_EDGE('',*,*,#6010,.F.);
#7902=ORIENTED_EDGE('',*,*,#6023,.T.);
#7903=ORIENTED_EDGE('',*,*,#6024,.T.);
#7904=ORIENTED_EDGE('',*,*,#6025,.T.);
#7905=ORIENTED_EDGE('',*,*,#6026,.T.);
#7906=ORIENTED_EDGE('',*,*,#6027,.T.);
#7907=ORIENTED_EDGE('',*,*,#6028,.T.);
#7908=ORIENTED_EDGE('',*,*,#6029,.T.);
#7909=ORIENTED_EDGE('',*,*,#6030,.T.);
#7910=ORIENTED_EDGE('',*,*,#6031,.T.);
#7911=ORIENTED_EDGE('',*,*,#6032,.T.);
#7912=ORIENTED_EDGE('',*,*,#6033,.T.);
#7913=ORIENTED_EDGE('',*,*,#6034,.F.);
#7914=ORIENTED_EDGE('',*,*,#6035,.T.);
#7915=ORIENTED_EDGE('',*,*,#6036,.T.);
#7916=ORIENTED_EDGE('',*,*,#6037,.T.);
#7917=ORIENTED_EDGE('',*,*,#5471,.T.);
#7918=ORIENTED_EDGE('',*,*,#6038,.T.);
#7919=ORIENTED_EDGE('',*,*,#6039,.T.);
#7920=ORIENTED_EDGE('',*,*,#6040,.T.);
#7921=ORIENTED_EDGE('',*,*,#6041,.T.);
#7922=ORIENTED_EDGE('',*,*,#6042,.T.);
#7923=ORIENTED_EDGE('',*,*,#6043,.F.);
#7924=ORIENTED_EDGE('',*,*,#6044,.T.);
#7925=ORIENTED_EDGE('',*,*,#6045,.T.);
#7926=ORIENTED_EDGE('',*,*,#6046,.F.);
#7927=ORIENTED_EDGE('',*,*,#6047,.T.);
#7928=ORIENTED_EDGE('',*,*,#6048,.T.);
#7929=ORIENTED_EDGE('',*,*,#6049,.T.);
#7930=ORIENTED_EDGE('',*,*,#6050,.T.);
#7931=ORIENTED_EDGE('',*,*,#6051,.T.);
#7932=ORIENTED_EDGE('',*,*,#6052,.T.);
#7933=ORIENTED_EDGE('',*,*,#6053,.T.);
#7934=ORIENTED_EDGE('',*,*,#6054,.T.);
#7935=ORIENTED_EDGE('',*,*,#6055,.T.);
#7936=ORIENTED_EDGE('',*,*,#6056,.T.);
#7937=ORIENTED_EDGE('',*,*,#6057,.T.);
#7938=ORIENTED_EDGE('',*,*,#6058,.T.);
#7939=ORIENTED_EDGE('',*,*,#6059,.T.);
#7940=ORIENTED_EDGE('',*,*,#6060,.T.);
#7941=ORIENTED_EDGE('',*,*,#6061,.T.);
#7942=ORIENTED_EDGE('',*,*,#6062,.T.);
#7943=ORIENTED_EDGE('',*,*,#6063,.T.);
#7944=ORIENTED_EDGE('',*,*,#6064,.T.);
#7945=ORIENTED_EDGE('',*,*,#6065,.T.);
#7946=ORIENTED_EDGE('',*,*,#5439,.T.);
#7947=ORIENTED_EDGE('',*,*,#6066,.T.);
#7948=ORIENTED_EDGE('',*,*,#6067,.T.);
#7949=ORIENTED_EDGE('',*,*,#5358,.T.);
#7950=ORIENTED_EDGE('',*,*,#6068,.T.);
#7951=ORIENTED_EDGE('',*,*,#6069,.T.);
#7952=ORIENTED_EDGE('',*,*,#6070,.T.);
#7953=ORIENTED_EDGE('',*,*,#6071,.T.);
#7954=ORIENTED_EDGE('',*,*,#6072,.T.);
#7955=ORIENTED_EDGE('',*,*,#6073,.T.);
#7956=ORIENTED_EDGE('',*,*,#6074,.T.);
#7957=ORIENTED_EDGE('',*,*,#6075,.T.);
#7958=ORIENTED_EDGE('',*,*,#5362,.T.);
#7959=ORIENTED_EDGE('',*,*,#6076,.T.);
#7960=ORIENTED_EDGE('',*,*,#6077,.T.);
#7961=ORIENTED_EDGE('',*,*,#6078,.T.);
#7962=ORIENTED_EDGE('',*,*,#6079,.F.);
#7963=ORIENTED_EDGE('',*,*,#6080,.T.);
#7964=ORIENTED_EDGE('',*,*,#6081,.F.);
#7965=ORIENTED_EDGE('',*,*,#6082,.T.);
#7966=ORIENTED_EDGE('',*,*,#6083,.F.);
#7967=ORIENTED_EDGE('',*,*,#5866,.F.);
#7968=ORIENTED_EDGE('',*,*,#6084,.T.);
#7969=ORIENTED_EDGE('',*,*,#6079,.T.);
#7970=ORIENTED_EDGE('',*,*,#6085,.T.);
#7971=ORIENTED_EDGE('',*,*,#6086,.T.);
#7972=ORIENTED_EDGE('',*,*,#6087,.T.);
#7973=ORIENTED_EDGE('',*,*,#6088,.T.);
#7974=ORIENTED_EDGE('',*,*,#6089,.F.);
#7975=ORIENTED_EDGE('',*,*,#6090,.T.);
#7976=ORIENTED_EDGE('',*,*,#6091,.F.);
#7977=ORIENTED_EDGE('',*,*,#6092,.T.);
#7978=ORIENTED_EDGE('',*,*,#6093,.F.);
#7979=ORIENTED_EDGE('',*,*,#6093,.T.);
#7980=ORIENTED_EDGE('',*,*,#6094,.T.);
#7981=ORIENTED_EDGE('',*,*,#5882,.F.);
#7982=ORIENTED_EDGE('',*,*,#6095,.T.);
#7983=ORIENTED_EDGE('',*,*,#6096,.T.);
#7984=ORIENTED_EDGE('',*,*,#6097,.T.);
#7985=ORIENTED_EDGE('',*,*,#6098,.T.);
#7986=ORIENTED_EDGE('',*,*,#6099,.T.);
#7987=ORIENTED_EDGE('',*,*,#6100,.F.);
#7988=ORIENTED_EDGE('',*,*,#6101,.T.);
#7989=ORIENTED_EDGE('',*,*,#6102,.T.);
#7990=ORIENTED_EDGE('',*,*,#6103,.T.);
#7991=ORIENTED_EDGE('',*,*,#6104,.F.);
#7992=ORIENTED_EDGE('',*,*,#6105,.T.);
#7993=ORIENTED_EDGE('',*,*,#6106,.T.);
#7994=ORIENTED_EDGE('',*,*,#5534,.T.);
#7995=ORIENTED_EDGE('',*,*,#6107,.T.);
#7996=ORIENTED_EDGE('',*,*,#6108,.T.);
#7997=ORIENTED_EDGE('',*,*,#6109,.T.);
#7998=ORIENTED_EDGE('',*,*,#5535,.T.);
#7999=ORIENTED_EDGE('',*,*,#6110,.T.);
#8000=ORIENTED_EDGE('',*,*,#6111,.T.);
#8001=ORIENTED_EDGE('',*,*,#5450,.T.);
#8002=ORIENTED_EDGE('',*,*,#6112,.T.);
#8003=ORIENTED_EDGE('',*,*,#6113,.T.);
#8004=ORIENTED_EDGE('',*,*,#6114,.T.);
#8005=ORIENTED_EDGE('',*,*,#6115,.T.);
#8006=ORIENTED_EDGE('',*,*,#5813,.F.);
#8007=ORIENTED_EDGE('',*,*,#6116,.T.);
#8008=ORIENTED_EDGE('',*,*,#6117,.T.);
#8009=ORIENTED_EDGE('',*,*,#6118,.T.);
#8010=ORIENTED_EDGE('',*,*,#6119,.T.);
#8011=ORIENTED_EDGE('',*,*,#6120,.T.);
#8012=ORIENTED_EDGE('',*,*,#6121,.T.);
#8013=ORIENTED_EDGE('',*,*,#6122,.T.);
#8014=ORIENTED_EDGE('',*,*,#6123,.T.);
#8015=ORIENTED_EDGE('',*,*,#6124,.T.);
#8016=ORIENTED_EDGE('',*,*,#6125,.T.);
#8017=ORIENTED_EDGE('',*,*,#6126,.T.);
#8018=ORIENTED_EDGE('',*,*,#6127,.T.);
#8019=ORIENTED_EDGE('',*,*,#6128,.T.);
#8020=ORIENTED_EDGE('',*,*,#6129,.T.);
#8021=ORIENTED_EDGE('',*,*,#6130,.T.);
#8022=ORIENTED_EDGE('',*,*,#5521,.T.);
#8023=ORIENTED_EDGE('',*,*,#6131,.T.);
#8024=ORIENTED_EDGE('',*,*,#6132,.T.);
#8025=ORIENTED_EDGE('',*,*,#6133,.T.);
#8026=ORIENTED_EDGE('',*,*,#6134,.T.);
#8027=ORIENTED_EDGE('',*,*,#6135,.T.);
#8028=ORIENTED_EDGE('',*,*,#5519,.T.);
#8029=ORIENTED_EDGE('',*,*,#6136,.T.);
#8030=ORIENTED_EDGE('',*,*,#6137,.T.);
#8031=ORIENTED_EDGE('',*,*,#6138,.T.);
#8032=ORIENTED_EDGE('',*,*,#6139,.T.);
#8033=ORIENTED_EDGE('',*,*,#6140,.T.);
#8034=ORIENTED_EDGE('',*,*,#5372,.T.);
#8035=ORIENTED_EDGE('',*,*,#6141,.T.);
#8036=ORIENTED_EDGE('',*,*,#6142,.T.);
#8037=ORIENTED_EDGE('',*,*,#6143,.T.);
#8038=ORIENTED_EDGE('',*,*,#6144,.T.);
#8039=ORIENTED_EDGE('',*,*,#5366,.T.);
#8040=ORIENTED_EDGE('',*,*,#6145,.T.);
#8041=ORIENTED_EDGE('',*,*,#6146,.T.);
#8042=ORIENTED_EDGE('',*,*,#6137,.F.);
#8043=ORIENTED_EDGE('',*,*,#5368,.T.);
#8044=ORIENTED_EDGE('',*,*,#6132,.F.);
#8045=ORIENTED_EDGE('',*,*,#5376,.T.);
#8046=ORIENTED_EDGE('',*,*,#6134,.F.);
#8047=ORIENTED_EDGE('',*,*,#6147,.T.);
#8048=ORIENTED_EDGE('',*,*,#5523,.F.);
#8049=ORIENTED_EDGE('',*,*,#6148,.T.);
#8050=ORIENTED_EDGE('',*,*,#5522,.F.);
#8051=ORIENTED_EDGE('',*,*,#6149,.T.);
#8052=ORIENTED_EDGE('',*,*,#6139,.F.);
#8053=ORIENTED_EDGE('',*,*,#6150,.T.);
#8054=ORIENTED_EDGE('',*,*,#6151,.T.);
#8055=ORIENTED_EDGE('',*,*,#6152,.T.);
#8056=ORIENTED_EDGE('',*,*,#6153,.T.);
#8057=ORIENTED_EDGE('',*,*,#6154,.T.);
#8058=ORIENTED_EDGE('',*,*,#6155,.T.);
#8059=ORIENTED_EDGE('',*,*,#6156,.T.);
#8060=ORIENTED_EDGE('',*,*,#6157,.T.);
#8061=ORIENTED_EDGE('',*,*,#6158,.T.);
#8062=ORIENTED_EDGE('',*,*,#6159,.T.);
#8063=ORIENTED_EDGE('',*,*,#6160,.T.);
#8064=ORIENTED_EDGE('',*,*,#6161,.T.);
#8065=ORIENTED_EDGE('',*,*,#6162,.F.);
#8066=ORIENTED_EDGE('',*,*,#6163,.T.);
#8067=ORIENTED_EDGE('',*,*,#6164,.T.);
#8068=ORIENTED_EDGE('',*,*,#6165,.T.);
#8069=ORIENTED_EDGE('',*,*,#6166,.T.);
#8070=ORIENTED_EDGE('',*,*,#6167,.T.);
#8071=ORIENTED_EDGE('',*,*,#6168,.T.);
#8072=ORIENTED_EDGE('',*,*,#6169,.T.);
#8073=ORIENTED_EDGE('',*,*,#6170,.T.);
#8074=ORIENTED_EDGE('',*,*,#6171,.F.);
#8075=ORIENTED_EDGE('',*,*,#6172,.T.);
#8076=ORIENTED_EDGE('',*,*,#6173,.T.);
#8077=ORIENTED_EDGE('',*,*,#6174,.F.);
#8078=ORIENTED_EDGE('',*,*,#6175,.T.);
#8079=ORIENTED_EDGE('',*,*,#6176,.T.);
#8080=ORIENTED_EDGE('',*,*,#6177,.T.);
#8081=ORIENTED_EDGE('',*,*,#6178,.T.);
#8082=ORIENTED_EDGE('',*,*,#6179,.T.);
#8083=ORIENTED_EDGE('',*,*,#5425,.T.);
#8084=ORIENTED_EDGE('',*,*,#6180,.T.);
#8085=ORIENTED_EDGE('',*,*,#5419,.T.);
#8086=ORIENTED_EDGE('',*,*,#6181,.T.);
#8087=ORIENTED_EDGE('',*,*,#5423,.T.);
#8088=ORIENTED_EDGE('',*,*,#6182,.T.);
#8089=ORIENTED_EDGE('',*,*,#6183,.T.);
#8090=ORIENTED_EDGE('',*,*,#6184,.T.);
#8091=ORIENTED_EDGE('',*,*,#6185,.T.);
#8092=ORIENTED_EDGE('',*,*,#6186,.F.);
#8093=ORIENTED_EDGE('',*,*,#6187,.T.);
#8094=ORIENTED_EDGE('',*,*,#6188,.T.);
#8095=ORIENTED_EDGE('',*,*,#6189,.T.);
#8096=ORIENTED_EDGE('',*,*,#6190,.F.);
#8097=ORIENTED_EDGE('',*,*,#6191,.T.);
#8098=ORIENTED_EDGE('',*,*,#6192,.F.);
#8099=ORIENTED_EDGE('',*,*,#6193,.T.);
#8100=ORIENTED_EDGE('',*,*,#5683,.F.);
#8101=ORIENTED_EDGE('',*,*,#6194,.T.);
#8102=ORIENTED_EDGE('',*,*,#6190,.T.);
#8103=ORIENTED_EDGE('',*,*,#6195,.T.);
#8104=ORIENTED_EDGE('',*,*,#6196,.T.);
#8105=ORIENTED_EDGE('',*,*,#6197,.T.);
#8106=ORIENTED_EDGE('',*,*,#6198,.F.);
#8107=ORIENTED_EDGE('',*,*,#6199,.T.);
#8108=ORIENTED_EDGE('',*,*,#6200,.F.);
#8109=ORIENTED_EDGE('',*,*,#6201,.T.);
#8110=ORIENTED_EDGE('',*,*,#6202,.F.);
#8111=ORIENTED_EDGE('',*,*,#6203,.T.);
#8112=ORIENTED_EDGE('',*,*,#6202,.T.);
#8113=ORIENTED_EDGE('',*,*,#6204,.T.);
#8114=ORIENTED_EDGE('',*,*,#5687,.F.);
#8115=ORIENTED_EDGE('',*,*,#6205,.T.);
#8116=ORIENTED_EDGE('',*,*,#6206,.T.);
#8117=ORIENTED_EDGE('',*,*,#6207,.T.);
#8118=ORIENTED_EDGE('',*,*,#6208,.T.);
#8119=ORIENTED_EDGE('',*,*,#6209,.T.);
#8120=ORIENTED_EDGE('',*,*,#6210,.F.);
#8121=ORIENTED_EDGE('',*,*,#6211,.T.);
#8122=ORIENTED_EDGE('',*,*,#6212,.T.);
#8123=ORIENTED_EDGE('',*,*,#6213,.T.);
#8124=ORIENTED_EDGE('',*,*,#6214,.F.);
#8125=ORIENTED_EDGE('',*,*,#6215,.T.);
#8126=ORIENTED_EDGE('',*,*,#6216,.T.);
#8127=ORIENTED_EDGE('',*,*,#5515,.T.);
#8128=ORIENTED_EDGE('',*,*,#6217,.T.);
#8129=ORIENTED_EDGE('',*,*,#6218,.T.);
#8130=ORIENTED_EDGE('',*,*,#6219,.T.);
#8131=ORIENTED_EDGE('',*,*,#5517,.T.);
#8132=ORIENTED_EDGE('',*,*,#6220,.T.);
#8133=ORIENTED_EDGE('',*,*,#6221,.T.);
#8134=ORIENTED_EDGE('',*,*,#6222,.T.);
#8135=ORIENTED_EDGE('',*,*,#6223,.T.);
#8136=ORIENTED_EDGE('',*,*,#6224,.T.);
#8137=ORIENTED_EDGE('',*,*,#6225,.T.);
#8138=ORIENTED_EDGE('',*,*,#6226,.T.);
#8139=ORIENTED_EDGE('',*,*,#6039,.F.);
#8140=ORIENTED_EDGE('',*,*,#6227,.T.);
#8141=ORIENTED_EDGE('',*,*,#6228,.T.);
#8142=ORIENTED_EDGE('',*,*,#6229,.T.);
#8143=ORIENTED_EDGE('',*,*,#6230,.T.);
#8144=ORIENTED_EDGE('',*,*,#6231,.T.);
#8145=ORIENTED_EDGE('',*,*,#6232,.T.);
#8146=ORIENTED_EDGE('',*,*,#6233,.T.);
#8147=ORIENTED_EDGE('',*,*,#6234,.T.);
#8148=ORIENTED_EDGE('',*,*,#6235,.T.);
#8149=ORIENTED_EDGE('',*,*,#6236,.T.);
#8150=ORIENTED_EDGE('',*,*,#6237,.T.);
#8151=ORIENTED_EDGE('',*,*,#6238,.T.);
#8152=ORIENTED_EDGE('',*,*,#5467,.T.);
#8153=ORIENTED_EDGE('',*,*,#6239,.T.);
#8154=ORIENTED_EDGE('',*,*,#6240,.T.);
#8155=ORIENTED_EDGE('',*,*,#5502,.T.);
#8156=ORIENTED_EDGE('',*,*,#6241,.T.);
#8157=ORIENTED_EDGE('',*,*,#6242,.T.);
#8158=ORIENTED_EDGE('',*,*,#6243,.T.);
#8159=ORIENTED_EDGE('',*,*,#6244,.T.);
#8160=ORIENTED_EDGE('',*,*,#6245,.T.);
#8161=ORIENTED_EDGE('',*,*,#6246,.T.);
#8162=ORIENTED_EDGE('',*,*,#5500,.T.);
#8163=ORIENTED_EDGE('',*,*,#6247,.T.);
#8164=ORIENTED_EDGE('',*,*,#6248,.T.);
#8165=ORIENTED_EDGE('',*,*,#6249,.T.);
#8166=ORIENTED_EDGE('',*,*,#6250,.T.);
#8167=ORIENTED_EDGE('',*,*,#6251,.F.);
#8168=ORIENTED_EDGE('',*,*,#6252,.T.);
#8169=ORIENTED_EDGE('',*,*,#6253,.T.);
#8170=ORIENTED_EDGE('',*,*,#6254,.T.);
#8171=ORIENTED_EDGE('',*,*,#6255,.T.);
#8172=ORIENTED_EDGE('',*,*,#6256,.T.);
#8173=ORIENTED_EDGE('',*,*,#6257,.T.);
#8174=ORIENTED_EDGE('',*,*,#6258,.T.);
#8175=ORIENTED_EDGE('',*,*,#5395,.T.);
#8176=ORIENTED_EDGE('',*,*,#5737,.T.);
#8177=ORIENTED_EDGE('',*,*,#6259,.T.);
#8178=ORIENTED_EDGE('',*,*,#6260,.F.);
#8179=ORIENTED_EDGE('',*,*,#6247,.F.);
#8180=ORIENTED_EDGE('',*,*,#6261,.T.);
#8181=ORIENTED_EDGE('',*,*,#6242,.F.);
#8182=ORIENTED_EDGE('',*,*,#6262,.T.);
#8183=ORIENTED_EDGE('',*,*,#5724,.F.);
#8184=ORIENTED_EDGE('',*,*,#5397,.T.);
#8185=ORIENTED_EDGE('',*,*,#5506,.F.);
#8186=ORIENTED_EDGE('',*,*,#5401,.T.);
#8187=ORIENTED_EDGE('',*,*,#5504,.F.);
#8188=ORIENTED_EDGE('',*,*,#6263,.T.);
#8189=ORIENTED_EDGE('',*,*,#6249,.F.);
#8190=ORIENTED_EDGE('',*,*,#6264,.T.);
#8191=ORIENTED_EDGE('',*,*,#6265,.T.);
#8192=ORIENTED_EDGE('',*,*,#6266,.T.);
#8193=ORIENTED_EDGE('',*,*,#6267,.T.);
#8194=ORIENTED_EDGE('',*,*,#6268,.T.);
#8195=ORIENTED_EDGE('',*,*,#6269,.T.);
#8196=ORIENTED_EDGE('',*,*,#6270,.T.);
#8197=ORIENTED_EDGE('',*,*,#6271,.T.);
#8198=ORIENTED_EDGE('',*,*,#5452,.T.);
#8199=ORIENTED_EDGE('',*,*,#6272,.T.);
#8200=ORIENTED_EDGE('',*,*,#6273,.T.);
#8201=ORIENTED_EDGE('',*,*,#6274,.F.);
#8202=ORIENTED_EDGE('',*,*,#6275,.T.);
#8203=ORIENTED_EDGE('',*,*,#6276,.T.);
#8204=ORIENTED_EDGE('',*,*,#6277,.T.);
#8205=ORIENTED_EDGE('',*,*,#6278,.T.);
#8206=ORIENTED_EDGE('',*,*,#6279,.T.);
#8207=ORIENTED_EDGE('',*,*,#5986,.T.);
#8208=ORIENTED_EDGE('',*,*,#6280,.T.);
#8209=ORIENTED_EDGE('',*,*,#6281,.T.);
#8210=ORIENTED_EDGE('',*,*,#6282,.T.);
#8211=ORIENTED_EDGE('',*,*,#6283,.F.);
#8212=ORIENTED_EDGE('',*,*,#6284,.T.);
#8213=ORIENTED_EDGE('',*,*,#6285,.T.);
#8214=ORIENTED_EDGE('',*,*,#6286,.F.);
#8215=ORIENTED_EDGE('',*,*,#6287,.T.);
#8216=ORIENTED_EDGE('',*,*,#6288,.T.);
#8217=ORIENTED_EDGE('',*,*,#6289,.T.);
#8218=ORIENTED_EDGE('',*,*,#6290,.T.);
#8219=ORIENTED_EDGE('',*,*,#6291,.T.);
#8220=ORIENTED_EDGE('',*,*,#6292,.T.);
#8221=ORIENTED_EDGE('',*,*,#6293,.T.);
#8222=ORIENTED_EDGE('',*,*,#6294,.T.);
#8223=ORIENTED_EDGE('',*,*,#6295,.T.);
#8224=ORIENTED_EDGE('',*,*,#6296,.T.);
#8225=ORIENTED_EDGE('',*,*,#6297,.T.);
#8226=ORIENTED_EDGE('',*,*,#6298,.T.);
#8227=ORIENTED_EDGE('',*,*,#5411,.T.);
#8228=ORIENTED_EDGE('',*,*,#6299,.T.);
#8229=ORIENTED_EDGE('',*,*,#6300,.T.);
#8230=ORIENTED_EDGE('',*,*,#6301,.T.);
#8231=ORIENTED_EDGE('',*,*,#6302,.T.);
#8232=ORIENTED_EDGE('',*,*,#6303,.T.);
#8233=ORIENTED_EDGE('',*,*,#5427,.T.);
#8234=ORIENTED_EDGE('',*,*,#6304,.T.);
#8235=ORIENTED_EDGE('',*,*,#6305,.T.);
#8236=ORIENTED_EDGE('',*,*,#5415,.T.);
#8237=ORIENTED_EDGE('',*,*,#6188,.F.);
#8238=ORIENTED_EDGE('',*,*,#6306,.T.);
#8239=ORIENTED_EDGE('',*,*,#5872,.T.);
#8240=ORIENTED_EDGE('',*,*,#6307,.T.);
#8241=ORIENTED_EDGE('',*,*,#5892,.T.);
#8242=ORIENTED_EDGE('',*,*,#6308,.T.);
#8243=ORIENTED_EDGE('',*,*,#6196,.F.);
#8244=ORIENTED_EDGE('',*,*,#6309,.T.);
#8245=ORIENTED_EDGE('',*,*,#6310,.T.);
#8246=ORIENTED_EDGE('',*,*,#6311,.T.);
#8247=ORIENTED_EDGE('',*,*,#6312,.T.);
#8248=ORIENTED_EDGE('',*,*,#6313,.T.);
#8249=ORIENTED_EDGE('',*,*,#6314,.T.);
#8250=ORIENTED_EDGE('',*,*,#6315,.T.);
#8251=ORIENTED_EDGE('',*,*,#5496,.T.);
#8252=ORIENTED_EDGE('',*,*,#6316,.T.);
#8253=ORIENTED_EDGE('',*,*,#6317,.T.);
#8254=ORIENTED_EDGE('',*,*,#6318,.T.);
#8255=ORIENTED_EDGE('',*,*,#5498,.T.);
#8256=ORIENTED_EDGE('',*,*,#6319,.T.);
#8257=ORIENTED_EDGE('',*,*,#6320,.T.);
#8258=ORIENTED_EDGE('',*,*,#6321,.T.);
#8259=ORIENTED_EDGE('',*,*,#6322,.T.);
#8260=ORIENTED_EDGE('',*,*,#6323,.T.);
#8261=ORIENTED_EDGE('',*,*,#5454,.T.);
#8262=ORIENTED_EDGE('',*,*,#6324,.T.);
#8263=ORIENTED_EDGE('',*,*,#6167,.F.);
#8264=ORIENTED_EDGE('',*,*,#6325,.T.);
#8265=ORIENTED_EDGE('',*,*,#6326,.T.);
#8266=ORIENTED_EDGE('',*,*,#6327,.T.);
#8267=ORIENTED_EDGE('',*,*,#6328,.T.);
#8268=ORIENTED_EDGE('',*,*,#6329,.T.);
#8269=ORIENTED_EDGE('',*,*,#6330,.T.);
#8270=ORIENTED_EDGE('',*,*,#6331,.T.);
#8271=ORIENTED_EDGE('',*,*,#5461,.T.);
#8272=ORIENTED_EDGE('',*,*,#6332,.T.);
#8273=ORIENTED_EDGE('',*,*,#6333,.T.);
#8274=ORIENTED_EDGE('',*,*,#6334,.T.);
#8275=ORIENTED_EDGE('',*,*,#6335,.T.);
#8276=ORIENTED_EDGE('',*,*,#6336,.T.);
#8277=ORIENTED_EDGE('',*,*,#6337,.T.);
#8278=ORIENTED_EDGE('',*,*,#6338,.T.);
#8279=ORIENTED_EDGE('',*,*,#5489,.T.);
#8280=ORIENTED_EDGE('',*,*,#6339,.T.);
#8281=ORIENTED_EDGE('',*,*,#6340,.T.);
#8282=ORIENTED_EDGE('',*,*,#6341,.T.);
#8283=ORIENTED_EDGE('',*,*,#6342,.T.);
#8284=ORIENTED_EDGE('',*,*,#6343,.T.);
#8285=ORIENTED_EDGE('',*,*,#5487,.T.);
#8286=ORIENTED_EDGE('',*,*,#6344,.T.);
#8287=ORIENTED_EDGE('',*,*,#6345,.T.);
#8288=ORIENTED_EDGE('',*,*,#6346,.T.);
#8289=ORIENTED_EDGE('',*,*,#6347,.T.);
#8290=ORIENTED_EDGE('',*,*,#6348,.T.);
#8291=ORIENTED_EDGE('',*,*,#6349,.T.);
#8292=ORIENTED_EDGE('',*,*,#6350,.T.);
#8293=ORIENTED_EDGE('',*,*,#6351,.T.);
#8294=ORIENTED_EDGE('',*,*,#6352,.T.);
#8295=ORIENTED_EDGE('',*,*,#6353,.T.);
#8296=ORIENTED_EDGE('',*,*,#6354,.T.);
#8297=ORIENTED_EDGE('',*,*,#6355,.T.);
#8298=ORIENTED_EDGE('',*,*,#5478,.T.);
#8299=ORIENTED_EDGE('',*,*,#6345,.F.);
#8300=ORIENTED_EDGE('',*,*,#6356,.T.);
#8301=ORIENTED_EDGE('',*,*,#6340,.F.);
#8302=ORIENTED_EDGE('',*,*,#6357,.T.);
#8303=ORIENTED_EDGE('',*,*,#6342,.F.);
#8304=ORIENTED_EDGE('',*,*,#6358,.T.);
#8305=ORIENTED_EDGE('',*,*,#5493,.F.);
#8306=ORIENTED_EDGE('',*,*,#6359,.T.);
#8307=ORIENTED_EDGE('',*,*,#5491,.F.);
#8308=ORIENTED_EDGE('',*,*,#5480,.T.);
#8309=ORIENTED_EDGE('',*,*,#6347,.F.);
#8310=ORIENTED_EDGE('',*,*,#5484,.T.);
#8311=ORIENTED_EDGE('',*,*,#5483,.F.);
#8312=ORIENTED_EDGE('',*,*,#5650,.F.);
#8313=ORIENTED_EDGE('',*,*,#6360,.F.);
#8314=ORIENTED_EDGE('',*,*,#5492,.F.);
#8315=ORIENTED_EDGE('',*,*,#6360,.T.);
#8316=ORIENTED_EDGE('',*,*,#5649,.F.);
#8317=ORIENTED_EDGE('',*,*,#6361,.F.);
#8318=ORIENTED_EDGE('',*,*,#6359,.F.);
#8319=ORIENTED_EDGE('',*,*,#6361,.T.);
#8320=ORIENTED_EDGE('',*,*,#5648,.F.);
#8321=ORIENTED_EDGE('',*,*,#6362,.F.);
#8322=ORIENTED_EDGE('',*,*,#6343,.F.);
#8323=ORIENTED_EDGE('',*,*,#5485,.T.);
#8324=ORIENTED_EDGE('',*,*,#6346,.F.);
#8325=ORIENTED_EDGE('',*,*,#6363,.F.);
#8326=ORIENTED_EDGE('',*,*,#5651,.F.);
#8327=ORIENTED_EDGE('',*,*,#6362,.T.);
#8328=ORIENTED_EDGE('',*,*,#5647,.F.);
#8329=ORIENTED_EDGE('',*,*,#6364,.F.);
#8330=ORIENTED_EDGE('',*,*,#5488,.F.);
#8331=ORIENTED_EDGE('',*,*,#6363,.T.);
#8332=ORIENTED_EDGE('',*,*,#6357,.F.);
#8333=ORIENTED_EDGE('',*,*,#6365,.F.);
#8334=ORIENTED_EDGE('',*,*,#5652,.F.);
#8335=ORIENTED_EDGE('',*,*,#6364,.T.);
#8336=ORIENTED_EDGE('',*,*,#5646,.F.);
#8337=ORIENTED_EDGE('',*,*,#6365,.T.);
#8338=ORIENTED_EDGE('',*,*,#6339,.F.);
#8339=ORIENTED_EDGE('',*,*,#5481,.F.);
#8340=ORIENTED_EDGE('',*,*,#5490,.F.);
#8341=ORIENTED_EDGE('',*,*,#6366,.F.);
#8342=ORIENTED_EDGE('',*,*,#6349,.F.);
#8343=ORIENTED_EDGE('',*,*,#6366,.T.);
#8344=ORIENTED_EDGE('',*,*,#6358,.F.);
#8345=ORIENTED_EDGE('',*,*,#6367,.F.);
#8346=ORIENTED_EDGE('',*,*,#6350,.F.);
#8347=ORIENTED_EDGE('',*,*,#6367,.T.);
#8348=ORIENTED_EDGE('',*,*,#6344,.F.);
#8349=ORIENTED_EDGE('',*,*,#6368,.F.);
#8350=ORIENTED_EDGE('',*,*,#6351,.F.);
#8351=ORIENTED_EDGE('',*,*,#5479,.T.);
#8352=ORIENTED_EDGE('',*,*,#6355,.F.);
#8353=ORIENTED_EDGE('',*,*,#6369,.F.);
#8354=ORIENTED_EDGE('',*,*,#6348,.F.);
#8355=ORIENTED_EDGE('',*,*,#6368,.T.);
#8356=ORIENTED_EDGE('',*,*,#5486,.F.);
#8357=ORIENTED_EDGE('',*,*,#6370,.F.);
#8358=ORIENTED_EDGE('',*,*,#6352,.F.);
#8359=ORIENTED_EDGE('',*,*,#6369,.T.);
#8360=ORIENTED_EDGE('',*,*,#6354,.F.);
#8361=ORIENTED_EDGE('',*,*,#6371,.F.);
#8362=ORIENTED_EDGE('',*,*,#6356,.F.);
#8363=ORIENTED_EDGE('',*,*,#6370,.T.);
#8364=ORIENTED_EDGE('',*,*,#6341,.F.);
#8365=ORIENTED_EDGE('',*,*,#6371,.T.);
#8366=ORIENTED_EDGE('',*,*,#6353,.F.);
#8367=ORIENTED_EDGE('',*,*,#6372,.F.);
#8368=ORIENTED_EDGE('',*,*,#5602,.T.);
#8369=ORIENTED_EDGE('',*,*,#6373,.T.);
#8370=ORIENTED_EDGE('',*,*,#6374,.T.);
#8371=ORIENTED_EDGE('',*,*,#6374,.F.);
#8372=ORIENTED_EDGE('',*,*,#6375,.T.);
#8373=ORIENTED_EDGE('',*,*,#6376,.T.);
#8374=ORIENTED_EDGE('',*,*,#6377,.T.);
#8375=ORIENTED_EDGE('',*,*,#6377,.F.);
#8376=ORIENTED_EDGE('',*,*,#6378,.T.);
#8377=ORIENTED_EDGE('',*,*,#5769,.T.);
#8378=ORIENTED_EDGE('',*,*,#6379,.T.);
#8379=ORIENTED_EDGE('',*,*,#6379,.F.);
#8380=ORIENTED_EDGE('',*,*,#5768,.T.);
#8381=ORIENTED_EDGE('',*,*,#6380,.T.);
#8382=ORIENTED_EDGE('',*,*,#6381,.T.);
#8383=ORIENTED_EDGE('',*,*,#6381,.F.);
#8384=ORIENTED_EDGE('',*,*,#6382,.T.);
#8385=ORIENTED_EDGE('',*,*,#6383,.F.);
#8386=ORIENTED_EDGE('',*,*,#6384,.T.);
#8387=ORIENTED_EDGE('',*,*,#6385,.F.);
#8388=ORIENTED_EDGE('',*,*,#6386,.T.);
#8389=ORIENTED_EDGE('',*,*,#5970,.T.);
#8390=ORIENTED_EDGE('',*,*,#6387,.T.);
#8391=ORIENTED_EDGE('',*,*,#6387,.F.);
#8392=ORIENTED_EDGE('',*,*,#5974,.T.);
#8393=ORIENTED_EDGE('',*,*,#6388,.T.);
#8394=ORIENTED_EDGE('',*,*,#6389,.T.);
#8395=ORIENTED_EDGE('',*,*,#6389,.F.);
#8396=ORIENTED_EDGE('',*,*,#6390,.T.);
#8397=ORIENTED_EDGE('',*,*,#6391,.T.);
#8398=ORIENTED_EDGE('',*,*,#6392,.T.);
#8399=ORIENTED_EDGE('',*,*,#6392,.F.);
#8400=ORIENTED_EDGE('',*,*,#6393,.T.);
#8401=ORIENTED_EDGE('',*,*,#5561,.T.);
#8402=ORIENTED_EDGE('',*,*,#6394,.T.);
#8403=ORIENTED_EDGE('',*,*,#6394,.F.);
#8404=ORIENTED_EDGE('',*,*,#5560,.T.);
#8405=ORIENTED_EDGE('',*,*,#6395,.F.);
#8406=ORIENTED_EDGE('',*,*,#6396,.T.);
#8407=ORIENTED_EDGE('',*,*,#6397,.F.);
#8408=ORIENTED_EDGE('',*,*,#5588,.T.);
#8409=ORIENTED_EDGE('',*,*,#6398,.T.);
#8410=ORIENTED_EDGE('',*,*,#6399,.T.);
#8411=ORIENTED_EDGE('',*,*,#6399,.F.);
#8412=ORIENTED_EDGE('',*,*,#6400,.T.);
#8413=ORIENTED_EDGE('',*,*,#6401,.T.);
#8414=ORIENTED_EDGE('',*,*,#6402,.T.);
#8415=ORIENTED_EDGE('',*,*,#6402,.F.);
#8416=ORIENTED_EDGE('',*,*,#6403,.T.);
#8417=ORIENTED_EDGE('',*,*,#5759,.T.);
#8418=ORIENTED_EDGE('',*,*,#6404,.T.);
#8419=ORIENTED_EDGE('',*,*,#6404,.F.);
#8420=ORIENTED_EDGE('',*,*,#5758,.T.);
#8421=ORIENTED_EDGE('',*,*,#6405,.T.);
#8422=ORIENTED_EDGE('',*,*,#6406,.T.);
#8423=ORIENTED_EDGE('',*,*,#6406,.F.);
#8424=ORIENTED_EDGE('',*,*,#6407,.T.);
#8425=ORIENTED_EDGE('',*,*,#6408,.F.);
#8426=ORIENTED_EDGE('',*,*,#6409,.T.);
#8427=ORIENTED_EDGE('',*,*,#6410,.F.);
#8428=ORIENTED_EDGE('',*,*,#6411,.T.);
#8429=ORIENTED_EDGE('',*,*,#5754,.T.);
#8430=ORIENTED_EDGE('',*,*,#6412,.T.);
#8431=ORIENTED_EDGE('',*,*,#6412,.F.);
#8432=ORIENTED_EDGE('',*,*,#5753,.T.);
#8433=ORIENTED_EDGE('',*,*,#6413,.T.);
#8434=ORIENTED_EDGE('',*,*,#6414,.T.);
#8435=ORIENTED_EDGE('',*,*,#6414,.F.);
#8436=ORIENTED_EDGE('',*,*,#6415,.T.);
#8437=ORIENTED_EDGE('',*,*,#6416,.T.);
#8438=ORIENTED_EDGE('',*,*,#6417,.T.);
#8439=ORIENTED_EDGE('',*,*,#6417,.F.);
#8440=ORIENTED_EDGE('',*,*,#6418,.T.);
#8441=ORIENTED_EDGE('',*,*,#5575,.T.);
#8442=ORIENTED_EDGE('',*,*,#6419,.T.);
#8443=ORIENTED_EDGE('',*,*,#6419,.F.);
#8444=ORIENTED_EDGE('',*,*,#5574,.T.);
#8445=ORIENTED_EDGE('',*,*,#6420,.F.);
#8446=ORIENTED_EDGE('',*,*,#6421,.T.);
#8447=ORIENTED_EDGE('',*,*,#6422,.F.);
#8448=ORIENTED_EDGE('',*,*,#6026,.F.);
#8449=ORIENTED_EDGE('',*,*,#6423,.F.);
#8450=ORIENTED_EDGE('',*,*,#6129,.F.);
#8451=ORIENTED_EDGE('',*,*,#6423,.T.);
#8452=ORIENTED_EDGE('',*,*,#6025,.F.);
#8453=ORIENTED_EDGE('',*,*,#6424,.F.);
#8454=ORIENTED_EDGE('',*,*,#6425,.F.);
#8455=ORIENTED_EDGE('',*,*,#6426,.F.);
#8456=ORIENTED_EDGE('',*,*,#6422,.T.);
#8457=ORIENTED_EDGE('',*,*,#6427,.F.);
#8458=ORIENTED_EDGE('',*,*,#5577,.T.);
#8459=ORIENTED_EDGE('',*,*,#6424,.T.);
#8460=ORIENTED_EDGE('',*,*,#6024,.F.);
#8461=ORIENTED_EDGE('',*,*,#6428,.F.);
#8462=ORIENTED_EDGE('',*,*,#6125,.F.);
#8463=ORIENTED_EDGE('',*,*,#6425,.T.);
#8464=ORIENTED_EDGE('',*,*,#6124,.F.);
#8465=ORIENTED_EDGE('',*,*,#6429,.F.);
#8466=ORIENTED_EDGE('',*,*,#6130,.F.);
#8467=ORIENTED_EDGE('',*,*,#6427,.T.);
#8468=ORIENTED_EDGE('',*,*,#6128,.F.);
#8469=ORIENTED_EDGE('',*,*,#6430,.F.);
#8470=ORIENTED_EDGE('',*,*,#5578,.F.);
#8471=ORIENTED_EDGE('',*,*,#6426,.T.);
#8472=ORIENTED_EDGE('',*,*,#5576,.F.);
#8473=ORIENTED_EDGE('',*,*,#6418,.F.);
#8474=ORIENTED_EDGE('',*,*,#6416,.F.);
#8475=ORIENTED_EDGE('',*,*,#6027,.F.);
#8476=ORIENTED_EDGE('',*,*,#6413,.F.);
#8477=ORIENTED_EDGE('',*,*,#5757,.F.);
#8478=ORIENTED_EDGE('',*,*,#6431,.F.);
#8479=ORIENTED_EDGE('',*,*,#6028,.F.);
#8480=ORIENTED_EDGE('',*,*,#6415,.F.);
#8481=ORIENTED_EDGE('',*,*,#6432,.F.);
#8482=ORIENTED_EDGE('',*,*,#5755,.F.);
#8483=ORIENTED_EDGE('',*,*,#6411,.F.);
#8484=ORIENTED_EDGE('',*,*,#6433,.F.);
#8485=ORIENTED_EDGE('',*,*,#5824,.F.);
#8486=ORIENTED_EDGE('',*,*,#6434,.F.);
#8487=ORIENTED_EDGE('',*,*,#5946,.F.);
#8488=ORIENTED_EDGE('',*,*,#6435,.F.);
#8489=ORIENTED_EDGE('',*,*,#5756,.F.);
#8490=ORIENTED_EDGE('',*,*,#6435,.T.);
#8491=ORIENTED_EDGE('',*,*,#5945,.T.);
#8492=ORIENTED_EDGE('',*,*,#6436,.F.);
#8493=ORIENTED_EDGE('',*,*,#6431,.T.);
#8494=ORIENTED_EDGE('',*,*,#6437,.F.);
#8495=ORIENTED_EDGE('',*,*,#6428,.T.);
#8496=ORIENTED_EDGE('',*,*,#6438,.F.);
#8497=ORIENTED_EDGE('',*,*,#6439,.F.);
#8498=ORIENTED_EDGE('',*,*,#6046,.T.);
#8499=ORIENTED_EDGE('',*,*,#6440,.F.);
#8500=ORIENTED_EDGE('',*,*,#6441,.F.);
#8501=ORIENTED_EDGE('',*,*,#6430,.T.);
#8502=ORIENTED_EDGE('',*,*,#6429,.T.);
#8503=ORIENTED_EDGE('',*,*,#6442,.F.);
#8504=ORIENTED_EDGE('',*,*,#6433,.T.);
#8505=ORIENTED_EDGE('',*,*,#6410,.T.);
#8506=ORIENTED_EDGE('',*,*,#6421,.F.);
#8507=ORIENTED_EDGE('',*,*,#6443,.F.);
#8508=ORIENTED_EDGE('',*,*,#6434,.T.);
#8509=ORIENTED_EDGE('',*,*,#6432,.T.);
#8510=ORIENTED_EDGE('',*,*,#6444,.F.);
#8511=ORIENTED_EDGE('',*,*,#5947,.T.);
#8512=ORIENTED_EDGE('',*,*,#6436,.T.);
#8513=ORIENTED_EDGE('',*,*,#5944,.F.);
#8514=ORIENTED_EDGE('',*,*,#6445,.F.);
#8515=ORIENTED_EDGE('',*,*,#6029,.F.);
#8516=ORIENTED_EDGE('',*,*,#6438,.T.);
#8517=ORIENTED_EDGE('',*,*,#6030,.F.);
#8518=ORIENTED_EDGE('',*,*,#6446,.F.);
#8519=ORIENTED_EDGE('',*,*,#6036,.F.);
#8520=ORIENTED_EDGE('',*,*,#6437,.T.);
#8521=ORIENTED_EDGE('',*,*,#6035,.F.);
#8522=ORIENTED_EDGE('',*,*,#6447,.F.);
#8523=ORIENTED_EDGE('',*,*,#6126,.F.);
#8524=ORIENTED_EDGE('',*,*,#6442,.T.);
#8525=ORIENTED_EDGE('',*,*,#6127,.F.);
#8526=ORIENTED_EDGE('',*,*,#6448,.F.);
#8527=ORIENTED_EDGE('',*,*,#5579,.F.);
#8528=ORIENTED_EDGE('',*,*,#6440,.T.);
#8529=ORIENTED_EDGE('',*,*,#6045,.F.);
#8530=ORIENTED_EDGE('',*,*,#6449,.F.);
#8531=ORIENTED_EDGE('',*,*,#6122,.F.);
#8532=ORIENTED_EDGE('',*,*,#6450,.F.);
#8533=ORIENTED_EDGE('',*,*,#6123,.F.);
#8534=ORIENTED_EDGE('',*,*,#6451,.F.);
#8535=ORIENTED_EDGE('',*,*,#5585,.F.);
#8536=ORIENTED_EDGE('',*,*,#6441,.T.);
#8537=ORIENTED_EDGE('',*,*,#6121,.F.);
#8538=ORIENTED_EDGE('',*,*,#6452,.F.);
#8539=ORIENTED_EDGE('',*,*,#6119,.F.);
#8540=ORIENTED_EDGE('',*,*,#6439,.T.);
#8541=ORIENTED_EDGE('',*,*,#6118,.F.);
#8542=ORIENTED_EDGE('',*,*,#6453,.F.);
#8543=ORIENTED_EDGE('',*,*,#6047,.F.);
#8544=ORIENTED_EDGE('',*,*,#6451,.T.);
#8545=ORIENTED_EDGE('',*,*,#6449,.T.);
#8546=ORIENTED_EDGE('',*,*,#6454,.F.);
#8547=ORIENTED_EDGE('',*,*,#5586,.F.);
#8548=ORIENTED_EDGE('',*,*,#6420,.T.);
#8549=ORIENTED_EDGE('',*,*,#5573,.F.);
#8550=ORIENTED_EDGE('',*,*,#6455,.F.);
#8551=ORIENTED_EDGE('',*,*,#5818,.F.);
#8552=ORIENTED_EDGE('',*,*,#6443,.T.);
#8553=ORIENTED_EDGE('',*,*,#6456,.F.);
#8554=ORIENTED_EDGE('',*,*,#5819,.F.);
#8555=ORIENTED_EDGE('',*,*,#6457,.F.);
#8556=ORIENTED_EDGE('',*,*,#5993,.F.);
#8557=ORIENTED_EDGE('',*,*,#6444,.T.);
#8558=ORIENTED_EDGE('',*,*,#5823,.F.);
#8559=ORIENTED_EDGE('',*,*,#6458,.F.);
#8560=ORIENTED_EDGE('',*,*,#5938,.F.);
#8561=ORIENTED_EDGE('',*,*,#6459,.F.);
#8562=ORIENTED_EDGE('',*,*,#5940,.F.);
#8563=ORIENTED_EDGE('',*,*,#6460,.F.);
#8564=ORIENTED_EDGE('',*,*,#5814,.F.);
#8565=ORIENTED_EDGE('',*,*,#6445,.T.);
#8566=ORIENTED_EDGE('',*,*,#5943,.T.);
#8567=ORIENTED_EDGE('',*,*,#6461,.F.);
#8568=ORIENTED_EDGE('',*,*,#6446,.T.);
#8569=ORIENTED_EDGE('',*,*,#6447,.T.);
#8570=ORIENTED_EDGE('',*,*,#6034,.T.);
#8571=ORIENTED_EDGE('',*,*,#6462,.F.);
#8572=ORIENTED_EDGE('',*,*,#6448,.T.);
#8573=ORIENTED_EDGE('',*,*,#6452,.T.);
#8574=ORIENTED_EDGE('',*,*,#6450,.T.);
#8575=ORIENTED_EDGE('',*,*,#6463,.F.);
#8576=ORIENTED_EDGE('',*,*,#6464,.F.);
#8577=ORIENTED_EDGE('',*,*,#6453,.T.);
#8578=ORIENTED_EDGE('',*,*,#6465,.F.);
#8579=ORIENTED_EDGE('',*,*,#6466,.F.);
#8580=ORIENTED_EDGE('',*,*,#5908,.T.);
#8581=ORIENTED_EDGE('',*,*,#6467,.F.);
#8582=ORIENTED_EDGE('',*,*,#6468,.F.);
#8583=ORIENTED_EDGE('',*,*,#6467,.T.);
#8584=ORIENTED_EDGE('',*,*,#5907,.F.);
#8585=ORIENTED_EDGE('',*,*,#6469,.F.);
#8586=ORIENTED_EDGE('',*,*,#5761,.F.);
#8587=ORIENTED_EDGE('',*,*,#6405,.F.);
#8588=ORIENTED_EDGE('',*,*,#5762,.F.);
#8589=ORIENTED_EDGE('',*,*,#6470,.F.);
#8590=ORIENTED_EDGE('',*,*,#6155,.F.);
#8591=ORIENTED_EDGE('',*,*,#6407,.F.);
#8592=ORIENTED_EDGE('',*,*,#6468,.T.);
#8593=ORIENTED_EDGE('',*,*,#5760,.F.);
#8594=ORIENTED_EDGE('',*,*,#6403,.F.);
#8595=ORIENTED_EDGE('',*,*,#6401,.F.);
#8596=ORIENTED_EDGE('',*,*,#6050,.F.);
#8597=ORIENTED_EDGE('',*,*,#6454,.T.);
#8598=ORIENTED_EDGE('',*,*,#6044,.F.);
#8599=ORIENTED_EDGE('',*,*,#6400,.F.);
#8600=ORIENTED_EDGE('',*,*,#6398,.F.);
#8601=ORIENTED_EDGE('',*,*,#5587,.F.);
#8602=ORIENTED_EDGE('',*,*,#6455,.T.);
#8603=ORIENTED_EDGE('',*,*,#5572,.F.);
#8604=ORIENTED_EDGE('',*,*,#6471,.F.);
#8605=ORIENTED_EDGE('',*,*,#6457,.T.);
#8606=ORIENTED_EDGE('',*,*,#5820,.T.);
#8607=ORIENTED_EDGE('',*,*,#6456,.T.);
#8608=ORIENTED_EDGE('',*,*,#6472,.F.);
#8609=ORIENTED_EDGE('',*,*,#6473,.F.);
#8610=ORIENTED_EDGE('',*,*,#5939,.F.);
#8611=ORIENTED_EDGE('',*,*,#6458,.T.);
#8612=ORIENTED_EDGE('',*,*,#6474,.F.);
#8613=ORIENTED_EDGE('',*,*,#6460,.T.);
#8614=ORIENTED_EDGE('',*,*,#6459,.T.);
#8615=ORIENTED_EDGE('',*,*,#6115,.F.);
#8616=ORIENTED_EDGE('',*,*,#5477,.F.);
#8617=ORIENTED_EDGE('',*,*,#5941,.F.);
#8618=ORIENTED_EDGE('',*,*,#6461,.T.);
#8619=ORIENTED_EDGE('',*,*,#5942,.F.);
#8620=ORIENTED_EDGE('',*,*,#5475,.F.);
#8621=ORIENTED_EDGE('',*,*,#6037,.F.);
#8622=ORIENTED_EDGE('',*,*,#6462,.T.);
#8623=ORIENTED_EDGE('',*,*,#6033,.F.);
#8624=ORIENTED_EDGE('',*,*,#6475,.F.);
#8625=ORIENTED_EDGE('',*,*,#5580,.F.);
#8626=ORIENTED_EDGE('',*,*,#6463,.T.);
#8627=ORIENTED_EDGE('',*,*,#5584,.F.);
#8628=ORIENTED_EDGE('',*,*,#6476,.F.);
#8629=ORIENTED_EDGE('',*,*,#6120,.F.);
#8630=ORIENTED_EDGE('',*,*,#6465,.T.);
#8631=ORIENTED_EDGE('',*,*,#6117,.F.);
#8632=ORIENTED_EDGE('',*,*,#6477,.F.);
#8633=ORIENTED_EDGE('',*,*,#6042,.F.);
#8634=ORIENTED_EDGE('',*,*,#6464,.T.);
#8635=ORIENTED_EDGE('',*,*,#6041,.F.);
#8636=ORIENTED_EDGE('',*,*,#6478,.F.);
#8637=ORIENTED_EDGE('',*,*,#6048,.F.);
#8638=ORIENTED_EDGE('',*,*,#6466,.T.);
#8639=ORIENTED_EDGE('',*,*,#6049,.F.);
#8640=ORIENTED_EDGE('',*,*,#6479,.F.);
#8641=ORIENTED_EDGE('',*,*,#5909,.F.);
#8642=ORIENTED_EDGE('',*,*,#6469,.T.);
#8643=ORIENTED_EDGE('',*,*,#5906,.T.);
#8644=ORIENTED_EDGE('',*,*,#6480,.F.);
#8645=ORIENTED_EDGE('',*,*,#6470,.T.);
#8646=ORIENTED_EDGE('',*,*,#5589,.T.);
#8647=ORIENTED_EDGE('',*,*,#6397,.T.);
#8648=ORIENTED_EDGE('',*,*,#6409,.F.);
#8649=ORIENTED_EDGE('',*,*,#6481,.F.);
#8650=ORIENTED_EDGE('',*,*,#6471,.T.);
#8651=ORIENTED_EDGE('',*,*,#5571,.F.);
#8652=ORIENTED_EDGE('',*,*,#6482,.F.);
#8653=ORIENTED_EDGE('',*,*,#5994,.F.);
#8654=ORIENTED_EDGE('',*,*,#6472,.T.);
#8655=ORIENTED_EDGE('',*,*,#5992,.F.);
#8656=ORIENTED_EDGE('',*,*,#6483,.F.);
#8657=ORIENTED_EDGE('',*,*,#5990,.F.);
#8658=ORIENTED_EDGE('',*,*,#6473,.T.);
#8659=ORIENTED_EDGE('',*,*,#5989,.F.);
#8660=ORIENTED_EDGE('',*,*,#6484,.F.);
#8661=ORIENTED_EDGE('',*,*,#5821,.F.);
#8662=ORIENTED_EDGE('',*,*,#6474,.T.);
#8663=ORIENTED_EDGE('',*,*,#5822,.F.);
#8664=ORIENTED_EDGE('',*,*,#6485,.F.);
#8665=ORIENTED_EDGE('',*,*,#5815,.F.);
#8666=ORIENTED_EDGE('',*,*,#5581,.T.);
#8667=ORIENTED_EDGE('',*,*,#6475,.T.);
#8668=ORIENTED_EDGE('',*,*,#6486,.F.);
#8669=ORIENTED_EDGE('',*,*,#6487,.F.);
#8670=ORIENTED_EDGE('',*,*,#6477,.T.);
#8671=ORIENTED_EDGE('',*,*,#6476,.T.);
#8672=ORIENTED_EDGE('',*,*,#5472,.F.);
#8673=ORIENTED_EDGE('',*,*,#6043,.T.);
#8674=ORIENTED_EDGE('',*,*,#6479,.T.);
#8675=ORIENTED_EDGE('',*,*,#6478,.T.);
#8676=ORIENTED_EDGE('',*,*,#6488,.F.);
#8677=ORIENTED_EDGE('',*,*,#5910,.F.);
#8678=ORIENTED_EDGE('',*,*,#6480,.T.);
#8679=ORIENTED_EDGE('',*,*,#5905,.F.);
#8680=ORIENTED_EDGE('',*,*,#6489,.F.);
#8681=ORIENTED_EDGE('',*,*,#6156,.F.);
#8682=ORIENTED_EDGE('',*,*,#6490,.F.);
#8683=ORIENTED_EDGE('',*,*,#6153,.F.);
#8684=ORIENTED_EDGE('',*,*,#6491,.F.);
#8685=ORIENTED_EDGE('',*,*,#6239,.F.);
#8686=ORIENTED_EDGE('',*,*,#6492,.F.);
#8687=ORIENTED_EDGE('',*,*,#5775,.F.);
#8688=ORIENTED_EDGE('',*,*,#6493,.F.);
#8689=ORIENTED_EDGE('',*,*,#6000,.F.);
#8690=ORIENTED_EDGE('',*,*,#6408,.T.);
#8691=ORIENTED_EDGE('',*,*,#6154,.F.);
#8692=ORIENTED_EDGE('',*,*,#6494,.F.);
#8693=ORIENTED_EDGE('',*,*,#5590,.F.);
#8694=ORIENTED_EDGE('',*,*,#6481,.T.);
#8695=ORIENTED_EDGE('',*,*,#6483,.T.);
#8696=ORIENTED_EDGE('',*,*,#6482,.T.);
#8697=ORIENTED_EDGE('',*,*,#6495,.F.);
#8698=ORIENTED_EDGE('',*,*,#6485,.T.);
#8699=ORIENTED_EDGE('',*,*,#6484,.T.);
#8700=ORIENTED_EDGE('',*,*,#6496,.F.);
#8701=ORIENTED_EDGE('',*,*,#5474,.T.);
#8702=ORIENTED_EDGE('',*,*,#6114,.F.);
#8703=ORIENTED_EDGE('',*,*,#6497,.F.);
#8704=ORIENTED_EDGE('',*,*,#6031,.F.);
#8705=ORIENTED_EDGE('',*,*,#6486,.T.);
#8706=ORIENTED_EDGE('',*,*,#6032,.F.);
#8707=ORIENTED_EDGE('',*,*,#6498,.F.);
#8708=ORIENTED_EDGE('',*,*,#5786,.F.);
#8709=ORIENTED_EDGE('',*,*,#6487,.T.);
#8710=ORIENTED_EDGE('',*,*,#5785,.F.);
#8711=ORIENTED_EDGE('',*,*,#6499,.F.);
#8712=ORIENTED_EDGE('',*,*,#5582,.F.);
#8713=ORIENTED_EDGE('',*,*,#6488,.T.);
#8714=ORIENTED_EDGE('',*,*,#6040,.F.);
#8715=ORIENTED_EDGE('',*,*,#6500,.F.);
#8716=ORIENTED_EDGE('',*,*,#5911,.F.);
#8717=ORIENTED_EDGE('',*,*,#6489,.T.);
#8718=ORIENTED_EDGE('',*,*,#5904,.T.);
#8719=ORIENTED_EDGE('',*,*,#6501,.F.);
#8720=ORIENTED_EDGE('',*,*,#6502,.F.);
#8721=ORIENTED_EDGE('',*,*,#6491,.T.);
#8722=ORIENTED_EDGE('',*,*,#6152,.F.);
#8723=ORIENTED_EDGE('',*,*,#6503,.F.);
#8724=ORIENTED_EDGE('',*,*,#6504,.F.);
#8725=ORIENTED_EDGE('',*,*,#6494,.T.);
#8726=ORIENTED_EDGE('',*,*,#6490,.T.);
#8727=ORIENTED_EDGE('',*,*,#5466,.F.);
#8728=ORIENTED_EDGE('',*,*,#5591,.T.);
#8729=ORIENTED_EDGE('',*,*,#6493,.T.);
#8730=ORIENTED_EDGE('',*,*,#5774,.F.);
#8731=ORIENTED_EDGE('',*,*,#6505,.F.);
#8732=ORIENTED_EDGE('',*,*,#6506,.F.);
#8733=ORIENTED_EDGE('',*,*,#6507,.F.);
#8734=ORIENTED_EDGE('',*,*,#6492,.T.);
#8735=ORIENTED_EDGE('',*,*,#6508,.F.);
#8736=ORIENTED_EDGE('',*,*,#5563,.T.);
#8737=ORIENTED_EDGE('',*,*,#6505,.T.);
#8738=ORIENTED_EDGE('',*,*,#5773,.F.);
#8739=ORIENTED_EDGE('',*,*,#6509,.F.);
#8740=ORIENTED_EDGE('',*,*,#5996,.F.);
#8741=ORIENTED_EDGE('',*,*,#6506,.T.);
#8742=ORIENTED_EDGE('',*,*,#5995,.F.);
#8743=ORIENTED_EDGE('',*,*,#6510,.F.);
#8744=ORIENTED_EDGE('',*,*,#6001,.F.);
#8745=ORIENTED_EDGE('',*,*,#6508,.T.);
#8746=ORIENTED_EDGE('',*,*,#5999,.F.);
#8747=ORIENTED_EDGE('',*,*,#6511,.F.);
#8748=ORIENTED_EDGE('',*,*,#5564,.F.);
#8749=ORIENTED_EDGE('',*,*,#6495,.T.);
#8750=ORIENTED_EDGE('',*,*,#5570,.F.);
#8751=ORIENTED_EDGE('',*,*,#6512,.F.);
#8752=ORIENTED_EDGE('',*,*,#5991,.F.);
#8753=ORIENTED_EDGE('',*,*,#6496,.T.);
#8754=ORIENTED_EDGE('',*,*,#5988,.F.);
#8755=ORIENTED_EDGE('',*,*,#6513,.F.);
#8756=ORIENTED_EDGE('',*,*,#5816,.F.);
#8757=ORIENTED_EDGE('',*,*,#6498,.T.);
#8758=ORIENTED_EDGE('',*,*,#6497,.T.);
#8759=ORIENTED_EDGE('',*,*,#6514,.F.);
#8760=ORIENTED_EDGE('',*,*,#5787,.F.);
#8761=ORIENTED_EDGE('',*,*,#5583,.T.);
#8762=ORIENTED_EDGE('',*,*,#6499,.T.);
#8763=ORIENTED_EDGE('',*,*,#6515,.F.);
#8764=ORIENTED_EDGE('',*,*,#5470,.T.);
#8765=ORIENTED_EDGE('',*,*,#6500,.T.);
#8766=ORIENTED_EDGE('',*,*,#6226,.F.);
#8767=ORIENTED_EDGE('',*,*,#6516,.F.);
#8768=ORIENTED_EDGE('',*,*,#5912,.F.);
#8769=ORIENTED_EDGE('',*,*,#6517,.F.);
#8770=ORIENTED_EDGE('',*,*,#6158,.F.);
#8771=ORIENTED_EDGE('',*,*,#6501,.T.);
#8772=ORIENTED_EDGE('',*,*,#5903,.F.);
#8773=ORIENTED_EDGE('',*,*,#6502,.T.);
#8774=ORIENTED_EDGE('',*,*,#6164,.F.);
#8775=ORIENTED_EDGE('',*,*,#6518,.F.);
#8776=ORIENTED_EDGE('',*,*,#6157,.F.);
#8777=ORIENTED_EDGE('',*,*,#6503,.T.);
#8778=ORIENTED_EDGE('',*,*,#6151,.F.);
#8779=ORIENTED_EDGE('',*,*,#6519,.F.);
#8780=ORIENTED_EDGE('',*,*,#6236,.F.);
#8781=ORIENTED_EDGE('',*,*,#6504,.T.);
#8782=ORIENTED_EDGE('',*,*,#6235,.F.);
#8783=ORIENTED_EDGE('',*,*,#6520,.F.);
#8784=ORIENTED_EDGE('',*,*,#6240,.F.);
#8785=ORIENTED_EDGE('',*,*,#6507,.T.);
#8786=ORIENTED_EDGE('',*,*,#5562,.F.);
#8787=ORIENTED_EDGE('',*,*,#6393,.F.);
#8788=ORIENTED_EDGE('',*,*,#6391,.F.);
#8789=ORIENTED_EDGE('',*,*,#5776,.F.);
#8790=ORIENTED_EDGE('',*,*,#6388,.F.);
#8791=ORIENTED_EDGE('',*,*,#5973,.F.);
#8792=ORIENTED_EDGE('',*,*,#6521,.F.);
#8793=ORIENTED_EDGE('',*,*,#5777,.F.);
#8794=ORIENTED_EDGE('',*,*,#6390,.F.);
#8795=ORIENTED_EDGE('',*,*,#6522,.F.);
#8796=ORIENTED_EDGE('',*,*,#5971,.F.);
#8797=ORIENTED_EDGE('',*,*,#6386,.F.);
#8798=ORIENTED_EDGE('',*,*,#6523,.F.);
#8799=ORIENTED_EDGE('',*,*,#6290,.F.);
#8800=ORIENTED_EDGE('',*,*,#6524,.F.);
#8801=ORIENTED_EDGE('',*,*,#5954,.F.);
#8802=ORIENTED_EDGE('',*,*,#6525,.F.);
#8803=ORIENTED_EDGE('',*,*,#5972,.F.);
#8804=ORIENTED_EDGE('',*,*,#6525,.T.);
#8805=ORIENTED_EDGE('',*,*,#5953,.T.);
#8806=ORIENTED_EDGE('',*,*,#6526,.F.);
#8807=ORIENTED_EDGE('',*,*,#6521,.T.);
#8808=ORIENTED_EDGE('',*,*,#6527,.F.);
#8809=ORIENTED_EDGE('',*,*,#6509,.T.);
#8810=ORIENTED_EDGE('',*,*,#6528,.F.);
#8811=ORIENTED_EDGE('',*,*,#6511,.T.);
#8812=ORIENTED_EDGE('',*,*,#6510,.T.);
#8813=ORIENTED_EDGE('',*,*,#6529,.F.);
#8814=ORIENTED_EDGE('',*,*,#6513,.T.);
#8815=ORIENTED_EDGE('',*,*,#6512,.T.);
#8816=ORIENTED_EDGE('',*,*,#6530,.F.);
#8817=ORIENTED_EDGE('',*,*,#5817,.T.);
#8818=ORIENTED_EDGE('',*,*,#6514,.T.);
#8819=ORIENTED_EDGE('',*,*,#6116,.F.);
#8820=ORIENTED_EDGE('',*,*,#6531,.F.);
#8821=ORIENTED_EDGE('',*,*,#5788,.F.);
#8822=ORIENTED_EDGE('',*,*,#6515,.T.);
#8823=ORIENTED_EDGE('',*,*,#5784,.F.);
#8824=ORIENTED_EDGE('',*,*,#6532,.F.);
#8825=ORIENTED_EDGE('',*,*,#6038,.F.);
#8826=ORIENTED_EDGE('',*,*,#5913,.F.);
#8827=ORIENTED_EDGE('',*,*,#6516,.T.);
#8828=ORIENTED_EDGE('',*,*,#6533,.F.);
#8829=ORIENTED_EDGE('',*,*,#5744,.T.);
#8830=ORIENTED_EDGE('',*,*,#6519,.T.);
#8831=ORIENTED_EDGE('',*,*,#6518,.T.);
#8832=ORIENTED_EDGE('',*,*,#6534,.F.);
#8833=ORIENTED_EDGE('',*,*,#5468,.T.);
#8834=ORIENTED_EDGE('',*,*,#6520,.T.);
#8835=ORIENTED_EDGE('',*,*,#6535,.F.);
#8836=ORIENTED_EDGE('',*,*,#6523,.T.);
#8837=ORIENTED_EDGE('',*,*,#6385,.T.);
#8838=ORIENTED_EDGE('',*,*,#6396,.F.);
#8839=ORIENTED_EDGE('',*,*,#6536,.F.);
#8840=ORIENTED_EDGE('',*,*,#6524,.T.);
#8841=ORIENTED_EDGE('',*,*,#6522,.T.);
#8842=ORIENTED_EDGE('',*,*,#6537,.F.);
#8843=ORIENTED_EDGE('',*,*,#5955,.T.);
#8844=ORIENTED_EDGE('',*,*,#6526,.T.);
#8845=ORIENTED_EDGE('',*,*,#5952,.F.);
#8846=ORIENTED_EDGE('',*,*,#6538,.F.);
#8847=ORIENTED_EDGE('',*,*,#5778,.F.);
#8848=ORIENTED_EDGE('',*,*,#6528,.T.);
#8849=ORIENTED_EDGE('',*,*,#5779,.F.);
#8850=ORIENTED_EDGE('',*,*,#6539,.F.);
#8851=ORIENTED_EDGE('',*,*,#5809,.F.);
#8852=ORIENTED_EDGE('',*,*,#6527,.T.);
#8853=ORIENTED_EDGE('',*,*,#5808,.F.);
#8854=ORIENTED_EDGE('',*,*,#6540,.F.);
#8855=ORIENTED_EDGE('',*,*,#5997,.F.);
#8856=ORIENTED_EDGE('',*,*,#6529,.T.);
#8857=ORIENTED_EDGE('',*,*,#5998,.F.);
#8858=ORIENTED_EDGE('',*,*,#6541,.F.);
#8859=ORIENTED_EDGE('',*,*,#5565,.F.);
#8860=ORIENTED_EDGE('',*,*,#6530,.T.);
#8861=ORIENTED_EDGE('',*,*,#5569,.F.);
#8862=ORIENTED_EDGE('',*,*,#6542,.F.);
#8863=ORIENTED_EDGE('',*,*,#5811,.F.);
#8864=ORIENTED_EDGE('',*,*,#6531,.T.);
#8865=ORIENTED_EDGE('',*,*,#5812,.F.);
#8866=ORIENTED_EDGE('',*,*,#6543,.F.);
#8867=ORIENTED_EDGE('',*,*,#5789,.F.);
#8868=ORIENTED_EDGE('',*,*,#6532,.T.);
#8869=ORIENTED_EDGE('',*,*,#5783,.F.);
#8870=ORIENTED_EDGE('',*,*,#6544,.F.);
#8871=ORIENTED_EDGE('',*,*,#6227,.F.);
#8872=ORIENTED_EDGE('',*,*,#6533,.T.);
#8873=ORIENTED_EDGE('',*,*,#6225,.F.);
#8874=ORIENTED_EDGE('',*,*,#6545,.F.);
#8875=ORIENTED_EDGE('',*,*,#5741,.F.);
#8876=ORIENTED_EDGE('',*,*,#6534,.T.);
#8877=ORIENTED_EDGE('',*,*,#6163,.F.);
#8878=ORIENTED_EDGE('',*,*,#6546,.F.);
#8879=ORIENTED_EDGE('',*,*,#6237,.F.);
#8880=ORIENTED_EDGE('',*,*,#6535,.T.);
#8881=ORIENTED_EDGE('',*,*,#6238,.F.);
#8882=ORIENTED_EDGE('',*,*,#6547,.F.);
#8883=ORIENTED_EDGE('',*,*,#5592,.F.);
#8884=ORIENTED_EDGE('',*,*,#6395,.T.);
#8885=ORIENTED_EDGE('',*,*,#5559,.F.);
#8886=ORIENTED_EDGE('',*,*,#6548,.F.);
#8887=ORIENTED_EDGE('',*,*,#6284,.F.);
#8888=ORIENTED_EDGE('',*,*,#6536,.T.);
#8889=ORIENTED_EDGE('',*,*,#6549,.F.);
#8890=ORIENTED_EDGE('',*,*,#6285,.F.);
#8891=ORIENTED_EDGE('',*,*,#6550,.F.);
#8892=ORIENTED_EDGE('',*,*,#6331,.F.);
#8893=ORIENTED_EDGE('',*,*,#6537,.T.);
#8894=ORIENTED_EDGE('',*,*,#6289,.F.);
#8895=ORIENTED_EDGE('',*,*,#6551,.F.);
#8896=ORIENTED_EDGE('',*,*,#5956,.F.);
#8897=ORIENTED_EDGE('',*,*,#6552,.F.);
#8898=ORIENTED_EDGE('',*,*,#5958,.F.);
#8899=ORIENTED_EDGE('',*,*,#6553,.F.);
#8900=ORIENTED_EDGE('',*,*,#6280,.F.);
#8901=ORIENTED_EDGE('',*,*,#6538,.T.);
#8902=ORIENTED_EDGE('',*,*,#5951,.T.);
#8903=ORIENTED_EDGE('',*,*,#6554,.F.);
#8904=ORIENTED_EDGE('',*,*,#6539,.T.);
#8905=ORIENTED_EDGE('',*,*,#6540,.T.);
#8906=ORIENTED_EDGE('',*,*,#5807,.T.);
#8907=ORIENTED_EDGE('',*,*,#5464,.F.);
#8908=ORIENTED_EDGE('',*,*,#6541,.T.);
#8909=ORIENTED_EDGE('',*,*,#6542,.T.);
#8910=ORIENTED_EDGE('',*,*,#5568,.T.);
#8911=ORIENTED_EDGE('',*,*,#6555,.F.);
#8912=ORIENTED_EDGE('',*,*,#6543,.T.);
#8913=ORIENTED_EDGE('',*,*,#6544,.T.);
#8914=ORIENTED_EDGE('',*,*,#5782,.F.);
#8915=ORIENTED_EDGE('',*,*,#5746,.F.);
#8916=ORIENTED_EDGE('',*,*,#6545,.T.);
#8917=ORIENTED_EDGE('',*,*,#6546,.T.);
#8918=ORIENTED_EDGE('',*,*,#6162,.T.);
#8919=ORIENTED_EDGE('',*,*,#6556,.F.);
#8920=ORIENTED_EDGE('',*,*,#6547,.T.);
#8921=ORIENTED_EDGE('',*,*,#6548,.T.);
#8922=ORIENTED_EDGE('',*,*,#5558,.F.);
#8923=ORIENTED_EDGE('',*,*,#5458,.F.);
#8924=ORIENTED_EDGE('',*,*,#6550,.T.);
#8925=ORIENTED_EDGE('',*,*,#6286,.T.);
#8926=ORIENTED_EDGE('',*,*,#6549,.T.);
#8927=ORIENTED_EDGE('',*,*,#6557,.F.);
#8928=ORIENTED_EDGE('',*,*,#6558,.F.);
#8929=ORIENTED_EDGE('',*,*,#5957,.F.);
#8930=ORIENTED_EDGE('',*,*,#6551,.T.);
#8931=ORIENTED_EDGE('',*,*,#6559,.F.);
#8932=ORIENTED_EDGE('',*,*,#6553,.T.);
#8933=ORIENTED_EDGE('',*,*,#6552,.T.);
#8934=ORIENTED_EDGE('',*,*,#5985,.F.);
#8935=ORIENTED_EDGE('',*,*,#6560,.F.);
#8936=ORIENTED_EDGE('',*,*,#5948,.F.);
#8937=ORIENTED_EDGE('',*,*,#6554,.T.);
#8938=ORIENTED_EDGE('',*,*,#5950,.F.);
#8939=ORIENTED_EDGE('',*,*,#6561,.F.);
#8940=ORIENTED_EDGE('',*,*,#5810,.F.);
#8941=ORIENTED_EDGE('',*,*,#6555,.T.);
#8942=ORIENTED_EDGE('',*,*,#5567,.F.);
#8943=ORIENTED_EDGE('',*,*,#6562,.F.);
#8944=ORIENTED_EDGE('',*,*,#5790,.F.);
#8945=ORIENTED_EDGE('',*,*,#6563,.F.);
#8946=ORIENTED_EDGE('',*,*,#5800,.F.);
#8947=ORIENTED_EDGE('',*,*,#6564,.F.);
#8948=ORIENTED_EDGE('',*,*,#6160,.F.);
#8949=ORIENTED_EDGE('',*,*,#6556,.T.);
#8950=ORIENTED_EDGE('',*,*,#6161,.F.);
#8951=ORIENTED_EDGE('',*,*,#6565,.F.);
#8952=ORIENTED_EDGE('',*,*,#5593,.F.);
#8953=ORIENTED_EDGE('',*,*,#6557,.T.);
#8954=ORIENTED_EDGE('',*,*,#6330,.F.);
#8955=ORIENTED_EDGE('',*,*,#6566,.F.);
#8956=ORIENTED_EDGE('',*,*,#6328,.F.);
#8957=ORIENTED_EDGE('',*,*,#6558,.T.);
#8958=ORIENTED_EDGE('',*,*,#6327,.F.);
#8959=ORIENTED_EDGE('',*,*,#6567,.F.);
#8960=ORIENTED_EDGE('',*,*,#6287,.F.);
#8961=ORIENTED_EDGE('',*,*,#6559,.T.);
#8962=ORIENTED_EDGE('',*,*,#6288,.F.);
#8963=ORIENTED_EDGE('',*,*,#6568,.F.);
#8964=ORIENTED_EDGE('',*,*,#6281,.F.);
#8965=ORIENTED_EDGE('',*,*,#5949,.F.);
#8966=ORIENTED_EDGE('',*,*,#6560,.T.);
#8967=ORIENTED_EDGE('',*,*,#6569,.F.);
#8968=ORIENTED_EDGE('',*,*,#6561,.T.);
#8969=ORIENTED_EDGE('',*,*,#5566,.T.);
#8970=ORIENTED_EDGE('',*,*,#5462,.T.);
#8971=ORIENTED_EDGE('',*,*,#6570,.F.);
#8972=ORIENTED_EDGE('',*,*,#6562,.T.);
#8973=ORIENTED_EDGE('',*,*,#6565,.T.);
#8974=ORIENTED_EDGE('',*,*,#6564,.T.);
#8975=ORIENTED_EDGE('',*,*,#6571,.F.);
#8976=ORIENTED_EDGE('',*,*,#5594,.T.);
#8977=ORIENTED_EDGE('',*,*,#6566,.T.);
#8978=ORIENTED_EDGE('',*,*,#5460,.T.);
#8979=ORIENTED_EDGE('',*,*,#6572,.F.);
#8980=ORIENTED_EDGE('',*,*,#6568,.T.);
#8981=ORIENTED_EDGE('',*,*,#6567,.T.);
#8982=ORIENTED_EDGE('',*,*,#6573,.F.);
#8983=ORIENTED_EDGE('',*,*,#6569,.T.);
#8984=ORIENTED_EDGE('',*,*,#5984,.F.);
#8985=ORIENTED_EDGE('',*,*,#6574,.F.);
#8986=ORIENTED_EDGE('',*,*,#5805,.F.);
#8987=ORIENTED_EDGE('',*,*,#6570,.T.);
#8988=ORIENTED_EDGE('',*,*,#5806,.F.);
#8989=ORIENTED_EDGE('',*,*,#6575,.F.);
#8990=ORIENTED_EDGE('',*,*,#5791,.F.);
#8991=ORIENTED_EDGE('',*,*,#6571,.T.);
#8992=ORIENTED_EDGE('',*,*,#5799,.F.);
#8993=ORIENTED_EDGE('',*,*,#6576,.F.);
#8994=ORIENTED_EDGE('',*,*,#5595,.F.);
#8995=ORIENTED_EDGE('',*,*,#6577,.F.);
#8996=ORIENTED_EDGE('',*,*,#6165,.F.);
#8997=ORIENTED_EDGE('',*,*,#6578,.F.);
#8998=ORIENTED_EDGE('',*,*,#5597,.F.);
#8999=ORIENTED_EDGE('',*,*,#6579,.F.);
#9000=ORIENTED_EDGE('',*,*,#6170,.F.);
#9001=ORIENTED_EDGE('',*,*,#6580,.F.);
#9002=ORIENTED_EDGE('',*,*,#6228,.F.);
#9003=ORIENTED_EDGE('',*,*,#6171,.T.);
#9004=ORIENTED_EDGE('',*,*,#6579,.T.);
#9005=ORIENTED_EDGE('',*,*,#6581,.F.);
#9006=ORIENTED_EDGE('',*,*,#6578,.T.);
#9007=ORIENTED_EDGE('',*,*,#6572,.T.);
#9008=ORIENTED_EDGE('',*,*,#5557,.F.);
#9009=ORIENTED_EDGE('',*,*,#6582,.F.);
#9010=ORIENTED_EDGE('',*,*,#6329,.F.);
#9011=ORIENTED_EDGE('',*,*,#6573,.T.);
#9012=ORIENTED_EDGE('',*,*,#6326,.F.);
#9013=ORIENTED_EDGE('',*,*,#6583,.F.);
#9014=ORIENTED_EDGE('',*,*,#6282,.F.);
#9015=ORIENTED_EDGE('',*,*,#6575,.T.);
#9016=ORIENTED_EDGE('',*,*,#6574,.T.);
#9017=ORIENTED_EDGE('',*,*,#6584,.F.);
#9018=ORIENTED_EDGE('',*,*,#5792,.F.);
#9019=ORIENTED_EDGE('',*,*,#5596,.T.);
#9020=ORIENTED_EDGE('',*,*,#6576,.T.);
#9021=ORIENTED_EDGE('',*,*,#6585,.F.);
#9022=ORIENTED_EDGE('',*,*,#6577,.T.);
#9023=ORIENTED_EDGE('',*,*,#6586,.F.);
#9024=ORIENTED_EDGE('',*,*,#6587,.F.);
#9025=ORIENTED_EDGE('',*,*,#6580,.T.);
#9026=ORIENTED_EDGE('',*,*,#6587,.T.);
#9027=ORIENTED_EDGE('',*,*,#6175,.F.);
#9028=ORIENTED_EDGE('',*,*,#6588,.F.);
#9029=ORIENTED_EDGE('',*,*,#6229,.F.);
#9030=ORIENTED_EDGE('',*,*,#6589,.F.);
#9031=ORIENTED_EDGE('',*,*,#6230,.F.);
#9032=ORIENTED_EDGE('',*,*,#6590,.F.);
#9033=ORIENTED_EDGE('',*,*,#6232,.F.);
#9034=ORIENTED_EDGE('',*,*,#6581,.T.);
#9035=ORIENTED_EDGE('',*,*,#6231,.F.);
#9036=ORIENTED_EDGE('',*,*,#6591,.F.);
#9037=ORIENTED_EDGE('',*,*,#5598,.F.);
#9038=ORIENTED_EDGE('',*,*,#6583,.T.);
#9039=ORIENTED_EDGE('',*,*,#6582,.T.);
#9040=ORIENTED_EDGE('',*,*,#6592,.F.);
#9041=ORIENTED_EDGE('',*,*,#6283,.T.);
#9042=ORIENTED_EDGE('',*,*,#6584,.T.);
#9043=ORIENTED_EDGE('',*,*,#5987,.F.);
#9044=ORIENTED_EDGE('',*,*,#6593,.F.);
#9045=ORIENTED_EDGE('',*,*,#5793,.F.);
#9046=ORIENTED_EDGE('',*,*,#6585,.T.);
#9047=ORIENTED_EDGE('',*,*,#5798,.F.);
#9048=ORIENTED_EDGE('',*,*,#6594,.F.);
#9049=ORIENTED_EDGE('',*,*,#6166,.F.);
#9050=ORIENTED_EDGE('',*,*,#6586,.T.);
#9051=ORIENTED_EDGE('',*,*,#6169,.F.);
#9052=ORIENTED_EDGE('',*,*,#6595,.F.);
#9053=ORIENTED_EDGE('',*,*,#6176,.F.);
#9054=ORIENTED_EDGE('',*,*,#6588,.T.);
#9055=ORIENTED_EDGE('',*,*,#6174,.T.);
#9056=ORIENTED_EDGE('',*,*,#6596,.F.);
#9057=ORIENTED_EDGE('',*,*,#6590,.T.);
#9058=ORIENTED_EDGE('',*,*,#6591,.T.);
#9059=ORIENTED_EDGE('',*,*,#6589,.T.);
#9060=ORIENTED_EDGE('',*,*,#6597,.F.);
#9061=ORIENTED_EDGE('',*,*,#6592,.T.);
#9062=ORIENTED_EDGE('',*,*,#5556,.F.);
#9063=ORIENTED_EDGE('',*,*,#6598,.F.);
#9064=ORIENTED_EDGE('',*,*,#6278,.F.);
#9065=ORIENTED_EDGE('',*,*,#6593,.T.);
#9066=ORIENTED_EDGE('',*,*,#6279,.F.);
#9067=ORIENTED_EDGE('',*,*,#6599,.F.);
#9068=ORIENTED_EDGE('',*,*,#5794,.F.);
#9069=ORIENTED_EDGE('',*,*,#6594,.T.);
#9070=ORIENTED_EDGE('',*,*,#5797,.F.);
#9071=ORIENTED_EDGE('',*,*,#5455,.F.);
#9072=ORIENTED_EDGE('',*,*,#6325,.F.);
#9073=ORIENTED_EDGE('',*,*,#6600,.F.);
#9074=ORIENTED_EDGE('',*,*,#5928,.F.);
#9075=ORIENTED_EDGE('',*,*,#6601,.F.);
#9076=ORIENTED_EDGE('',*,*,#6595,.T.);
#9077=ORIENTED_EDGE('',*,*,#6601,.T.);
#9078=ORIENTED_EDGE('',*,*,#5927,.F.);
#9079=ORIENTED_EDGE('',*,*,#6602,.F.);
#9080=ORIENTED_EDGE('',*,*,#6177,.F.);
#9081=ORIENTED_EDGE('',*,*,#6596,.T.);
#9082=ORIENTED_EDGE('',*,*,#6173,.F.);
#9083=ORIENTED_EDGE('',*,*,#6603,.F.);
#9084=ORIENTED_EDGE('',*,*,#6233,.F.);
#9085=ORIENTED_EDGE('',*,*,#6597,.T.);
#9086=ORIENTED_EDGE('',*,*,#6234,.F.);
#9087=ORIENTED_EDGE('',*,*,#6604,.F.);
#9088=ORIENTED_EDGE('',*,*,#5599,.F.);
#9089=ORIENTED_EDGE('',*,*,#6598,.T.);
#9090=ORIENTED_EDGE('',*,*,#5555,.T.);
#9091=ORIENTED_EDGE('',*,*,#6605,.F.);
#9092=ORIENTED_EDGE('',*,*,#6599,.T.);
#9093=ORIENTED_EDGE('',*,*,#6600,.T.);
#9094=ORIENTED_EDGE('',*,*,#6168,.F.);
#9095=ORIENTED_EDGE('',*,*,#6606,.F.);
#9096=ORIENTED_EDGE('',*,*,#5929,.F.);
#9097=ORIENTED_EDGE('',*,*,#6602,.T.);
#9098=ORIENTED_EDGE('',*,*,#5937,.T.);
#9099=ORIENTED_EDGE('',*,*,#6607,.F.);
#9100=ORIENTED_EDGE('',*,*,#6608,.F.);
#9101=ORIENTED_EDGE('',*,*,#6604,.T.);
#9102=ORIENTED_EDGE('',*,*,#6603,.T.);
#9103=ORIENTED_EDGE('',*,*,#6609,.F.);
#9104=ORIENTED_EDGE('',*,*,#5600,.F.);
#9105=ORIENTED_EDGE('',*,*,#6605,.T.);
#9106=ORIENTED_EDGE('',*,*,#5554,.F.);
#9107=ORIENTED_EDGE('',*,*,#6610,.F.);
#9108=ORIENTED_EDGE('',*,*,#5795,.F.);
#9109=ORIENTED_EDGE('',*,*,#5457,.T.);
#9110=ORIENTED_EDGE('',*,*,#5796,.F.);
#9111=ORIENTED_EDGE('',*,*,#6611,.F.);
#9112=ORIENTED_EDGE('',*,*,#6272,.F.);
#9113=ORIENTED_EDGE('',*,*,#6606,.T.);
#9114=ORIENTED_EDGE('',*,*,#6324,.F.);
#9115=ORIENTED_EDGE('',*,*,#6612,.F.);
#9116=ORIENTED_EDGE('',*,*,#5930,.F.);
#9117=ORIENTED_EDGE('',*,*,#6607,.T.);
#9118=ORIENTED_EDGE('',*,*,#5936,.F.);
#9119=ORIENTED_EDGE('',*,*,#6613,.F.);
#9120=ORIENTED_EDGE('',*,*,#5771,.F.);
#9121=ORIENTED_EDGE('',*,*,#6380,.F.);
#9122=ORIENTED_EDGE('',*,*,#5772,.F.);
#9123=ORIENTED_EDGE('',*,*,#6614,.F.);
#9124=ORIENTED_EDGE('',*,*,#6269,.F.);
#9125=ORIENTED_EDGE('',*,*,#6382,.F.);
#9126=ORIENTED_EDGE('',*,*,#6608,.T.);
#9127=ORIENTED_EDGE('',*,*,#5770,.F.);
#9128=ORIENTED_EDGE('',*,*,#6378,.F.);
#9129=ORIENTED_EDGE('',*,*,#6376,.F.);
#9130=ORIENTED_EDGE('',*,*,#6178,.F.);
#9131=ORIENTED_EDGE('',*,*,#6609,.T.);
#9132=ORIENTED_EDGE('',*,*,#6172,.F.);
#9133=ORIENTED_EDGE('',*,*,#6375,.F.);
#9134=ORIENTED_EDGE('',*,*,#6373,.F.);
#9135=ORIENTED_EDGE('',*,*,#5601,.F.);
#9136=ORIENTED_EDGE('',*,*,#6610,.T.);
#9137=ORIENTED_EDGE('',*,*,#5553,.T.);
#9138=ORIENTED_EDGE('',*,*,#6615,.F.);
#9139=ORIENTED_EDGE('',*,*,#6611,.T.);
#9140=ORIENTED_EDGE('',*,*,#6612,.T.);
#9141=ORIENTED_EDGE('',*,*,#5453,.T.);
#9142=ORIENTED_EDGE('',*,*,#6616,.F.);
#9143=ORIENTED_EDGE('',*,*,#5931,.F.);
#9144=ORIENTED_EDGE('',*,*,#6613,.T.);
#9145=ORIENTED_EDGE('',*,*,#5935,.T.);
#9146=ORIENTED_EDGE('',*,*,#6617,.F.);
#9147=ORIENTED_EDGE('',*,*,#6614,.T.);
#9148=ORIENTED_EDGE('',*,*,#5547,.T.);
#9149=ORIENTED_EDGE('',*,*,#6372,.T.);
#9150=ORIENTED_EDGE('',*,*,#6384,.F.);
#9151=ORIENTED_EDGE('',*,*,#6618,.F.);
#9152=ORIENTED_EDGE('',*,*,#6615,.T.);
#9153=ORIENTED_EDGE('',*,*,#5552,.F.);
#9154=ORIENTED_EDGE('',*,*,#6619,.F.);
#9155=ORIENTED_EDGE('',*,*,#6273,.F.);
#9156=ORIENTED_EDGE('',*,*,#6616,.T.);
#9157=ORIENTED_EDGE('',*,*,#6277,.F.);
#9158=ORIENTED_EDGE('',*,*,#6620,.F.);
#9159=ORIENTED_EDGE('',*,*,#5932,.F.);
#9160=ORIENTED_EDGE('',*,*,#6617,.T.);
#9161=ORIENTED_EDGE('',*,*,#5934,.F.);
#9162=ORIENTED_EDGE('',*,*,#6621,.F.);
#9163=ORIENTED_EDGE('',*,*,#6270,.F.);
#9164=ORIENTED_EDGE('',*,*,#6383,.T.);
#9165=ORIENTED_EDGE('',*,*,#6268,.F.);
#9166=ORIENTED_EDGE('',*,*,#6622,.F.);
#9167=ORIENTED_EDGE('',*,*,#5548,.F.);
#9168=ORIENTED_EDGE('',*,*,#6618,.T.);
#9169=ORIENTED_EDGE('',*,*,#6623,.F.);
#9170=ORIENTED_EDGE('',*,*,#5550,.F.);
#9171=ORIENTED_EDGE('',*,*,#6624,.F.);
#9172=ORIENTED_EDGE('',*,*,#6336,.F.);
#9173=ORIENTED_EDGE('',*,*,#6625,.F.);
#9174=ORIENTED_EDGE('',*,*,#5551,.F.);
#9175=ORIENTED_EDGE('',*,*,#6626,.F.);
#9176=ORIENTED_EDGE('',*,*,#6335,.F.);
#9177=ORIENTED_EDGE('',*,*,#6619,.T.);
#9178=ORIENTED_EDGE('',*,*,#6625,.T.);
#9179=ORIENTED_EDGE('',*,*,#6627,.F.);
#9180=ORIENTED_EDGE('',*,*,#6274,.T.);
#9181=ORIENTED_EDGE('',*,*,#5933,.T.);
#9182=ORIENTED_EDGE('',*,*,#6620,.T.);
#9183=ORIENTED_EDGE('',*,*,#6628,.F.);
#9184=ORIENTED_EDGE('',*,*,#6621,.T.);
#9185=ORIENTED_EDGE('',*,*,#5549,.T.);
#9186=ORIENTED_EDGE('',*,*,#6622,.T.);
#9187=ORIENTED_EDGE('',*,*,#6629,.F.);
#9188=ORIENTED_EDGE('',*,*,#6624,.T.);
#9189=ORIENTED_EDGE('',*,*,#6626,.T.);
#9190=ORIENTED_EDGE('',*,*,#6623,.T.);
#9191=ORIENTED_EDGE('',*,*,#6630,.F.);
#9192=ORIENTED_EDGE('',*,*,#6627,.T.);
#9193=ORIENTED_EDGE('',*,*,#6334,.F.);
#9194=ORIENTED_EDGE('',*,*,#6631,.F.);
#9195=ORIENTED_EDGE('',*,*,#6275,.F.);
#9196=ORIENTED_EDGE('',*,*,#6628,.T.);
#9197=ORIENTED_EDGE('',*,*,#6276,.F.);
#9198=ORIENTED_EDGE('',*,*,#6632,.F.);
#9199=ORIENTED_EDGE('',*,*,#6271,.F.);
#9200=ORIENTED_EDGE('',*,*,#6629,.T.);
#9201=ORIENTED_EDGE('',*,*,#6267,.F.);
#9202=ORIENTED_EDGE('',*,*,#6633,.F.);
#9203=ORIENTED_EDGE('',*,*,#6337,.F.);
#9204=ORIENTED_EDGE('',*,*,#6630,.T.);
#9205=ORIENTED_EDGE('',*,*,#6338,.F.);
#9206=ORIENTED_EDGE('',*,*,#6634,.F.);
#9207=ORIENTED_EDGE('',*,*,#6332,.F.);
#9208=ORIENTED_EDGE('',*,*,#6632,.T.);
#9209=ORIENTED_EDGE('',*,*,#6631,.T.);
#9210=ORIENTED_EDGE('',*,*,#6635,.F.);
#9211=ORIENTED_EDGE('',*,*,#6633,.T.);
#9212=ORIENTED_EDGE('',*,*,#6266,.F.);
#9213=ORIENTED_EDGE('',*,*,#6636,.F.);
#9214=ORIENTED_EDGE('',*,*,#6634,.T.);
#9215=ORIENTED_EDGE('',*,*,#6635,.T.);
#9216=ORIENTED_EDGE('',*,*,#6333,.F.);
#9217=ORIENTED_EDGE('',*,*,#6636,.T.);
#9218=ORIENTED_EDGE('',*,*,#6265,.F.);
#9219=ORIENTED_EDGE('',*,*,#6637,.F.);
#9220=ORIENTED_EDGE('',*,*,#5843,.F.);
#9221=ORIENTED_EDGE('',*,*,#6638,.F.);
#9222=ORIENTED_EDGE('',*,*,#6112,.F.);
#9223=ORIENTED_EDGE('',*,*,#6639,.F.);
#9224=ORIENTED_EDGE('',*,*,#6637,.T.);
#9225=ORIENTED_EDGE('',*,*,#5449,.F.);
#9226=ORIENTED_EDGE('',*,*,#6640,.F.);
#9227=ORIENTED_EDGE('',*,*,#6638,.T.);
#9228=ORIENTED_EDGE('',*,*,#6641,.F.);
#9229=ORIENTED_EDGE('',*,*,#6639,.T.);
#9230=ORIENTED_EDGE('',*,*,#5835,.F.);
#9231=ORIENTED_EDGE('',*,*,#6642,.F.);
#9232=ORIENTED_EDGE('',*,*,#5844,.F.);
#9233=ORIENTED_EDGE('',*,*,#6641,.T.);
#9234=ORIENTED_EDGE('',*,*,#5848,.F.);
#9235=ORIENTED_EDGE('',*,*,#6643,.F.);
#9236=ORIENTED_EDGE('',*,*,#6075,.F.);
#9237=ORIENTED_EDGE('',*,*,#6640,.T.);
#9238=ORIENTED_EDGE('',*,*,#6074,.F.);
#9239=ORIENTED_EDGE('',*,*,#6644,.F.);
#9240=ORIENTED_EDGE('',*,*,#6113,.F.);
#9241=ORIENTED_EDGE('',*,*,#6645,.F.);
#9242=ORIENTED_EDGE('',*,*,#5447,.T.);
#9243=ORIENTED_EDGE('',*,*,#6646,.F.);
#9244=ORIENTED_EDGE('',*,*,#6647,.F.);
#9245=ORIENTED_EDGE('',*,*,#6642,.T.);
#9246=ORIENTED_EDGE('',*,*,#5445,.F.);
#9247=ORIENTED_EDGE('',*,*,#6648,.F.);
#9248=ORIENTED_EDGE('',*,*,#6643,.T.);
#9249=ORIENTED_EDGE('',*,*,#6649,.F.);
#9250=ORIENTED_EDGE('',*,*,#5884,.T.);
#9251=ORIENTED_EDGE('',*,*,#6644,.T.);
#9252=ORIENTED_EDGE('',*,*,#6073,.F.);
#9253=ORIENTED_EDGE('',*,*,#6650,.F.);
#9254=ORIENTED_EDGE('',*,*,#5533,.F.);
#9255=ORIENTED_EDGE('',*,*,#6646,.T.);
#9256=ORIENTED_EDGE('',*,*,#6111,.F.);
#9257=ORIENTED_EDGE('',*,*,#6651,.F.);
#9258=ORIENTED_EDGE('',*,*,#5612,.F.);
#9259=ORIENTED_EDGE('',*,*,#6645,.T.);
#9260=ORIENTED_EDGE('',*,*,#5611,.F.);
#9261=ORIENTED_EDGE('',*,*,#6652,.F.);
#9262=ORIENTED_EDGE('',*,*,#5836,.F.);
#9263=ORIENTED_EDGE('',*,*,#6647,.T.);
#9264=ORIENTED_EDGE('',*,*,#5978,.F.);
#9265=ORIENTED_EDGE('',*,*,#6653,.F.);
#9266=ORIENTED_EDGE('',*,*,#5845,.F.);
#9267=ORIENTED_EDGE('',*,*,#6654,.F.);
#9268=ORIENTED_EDGE('',*,*,#5846,.F.);
#9269=ORIENTED_EDGE('',*,*,#6655,.F.);
#9270=ORIENTED_EDGE('',*,*,#5859,.F.);
#9271=ORIENTED_EDGE('',*,*,#6649,.T.);
#9272=ORIENTED_EDGE('',*,*,#5847,.F.);
#9273=ORIENTED_EDGE('',*,*,#6656,.F.);
#9274=ORIENTED_EDGE('',*,*,#5885,.F.);
#9275=ORIENTED_EDGE('',*,*,#6648,.T.);
#9276=ORIENTED_EDGE('',*,*,#5883,.F.);
#9277=ORIENTED_EDGE('',*,*,#6657,.F.);
#9278=ORIENTED_EDGE('',*,*,#6068,.F.);
#9279=ORIENTED_EDGE('',*,*,#6650,.T.);
#9280=ORIENTED_EDGE('',*,*,#6072,.F.);
#9281=ORIENTED_EDGE('',*,*,#6658,.F.);
#9282=ORIENTED_EDGE('',*,*,#6107,.F.);
#9283=ORIENTED_EDGE('',*,*,#6659,.F.);
#9284=ORIENTED_EDGE('',*,*,#6651,.T.);
#9285=ORIENTED_EDGE('',*,*,#6660,.F.);
#9286=ORIENTED_EDGE('',*,*,#5443,.T.);
#9287=ORIENTED_EDGE('',*,*,#6652,.T.);
#9288=ORIENTED_EDGE('',*,*,#6661,.F.);
#9289=ORIENTED_EDGE('',*,*,#6655,.T.);
#9290=ORIENTED_EDGE('',*,*,#6653,.T.);
#9291=ORIENTED_EDGE('',*,*,#6662,.F.);
#9292=ORIENTED_EDGE('',*,*,#6656,.T.);
#9293=ORIENTED_EDGE('',*,*,#6654,.T.);
#9294=ORIENTED_EDGE('',*,*,#6663,.F.);
#9295=ORIENTED_EDGE('',*,*,#5886,.T.);
#9296=ORIENTED_EDGE('',*,*,#6657,.T.);
#9297=ORIENTED_EDGE('',*,*,#6094,.F.);
#9298=ORIENTED_EDGE('',*,*,#6664,.F.);
#9299=ORIENTED_EDGE('',*,*,#6069,.F.);
#9300=ORIENTED_EDGE('',*,*,#6665,.F.);
#9301=ORIENTED_EDGE('',*,*,#6658,.T.);
#9302=ORIENTED_EDGE('',*,*,#6666,.F.);
#9303=ORIENTED_EDGE('',*,*,#6660,.T.);
#9304=ORIENTED_EDGE('',*,*,#6110,.F.);
#9305=ORIENTED_EDGE('',*,*,#5440,.F.);
#9306=ORIENTED_EDGE('',*,*,#6065,.F.);
#9307=ORIENTED_EDGE('',*,*,#6659,.T.);
#9308=ORIENTED_EDGE('',*,*,#6064,.F.);
#9309=ORIENTED_EDGE('',*,*,#6667,.F.);
#9310=ORIENTED_EDGE('',*,*,#5613,.F.);
#9311=ORIENTED_EDGE('',*,*,#6661,.T.);
#9312=ORIENTED_EDGE('',*,*,#5617,.F.);
#9313=ORIENTED_EDGE('',*,*,#6668,.F.);
#9314=ORIENTED_EDGE('',*,*,#5975,.F.);
#9315=ORIENTED_EDGE('',*,*,#6662,.T.);
#9316=ORIENTED_EDGE('',*,*,#5977,.F.);
#9317=ORIENTED_EDGE('',*,*,#6669,.F.);
#9318=ORIENTED_EDGE('',*,*,#5860,.F.);
#9319=ORIENTED_EDGE('',*,*,#6663,.T.);
#9320=ORIENTED_EDGE('',*,*,#5858,.F.);
#9321=ORIENTED_EDGE('',*,*,#6670,.F.);
#9322=ORIENTED_EDGE('',*,*,#5887,.F.);
#9323=ORIENTED_EDGE('',*,*,#6664,.T.);
#9324=ORIENTED_EDGE('',*,*,#6092,.F.);
#9325=ORIENTED_EDGE('',*,*,#6671,.F.);
#9326=ORIENTED_EDGE('',*,*,#6070,.F.);
#9327=ORIENTED_EDGE('',*,*,#6666,.T.);
#9328=ORIENTED_EDGE('',*,*,#6071,.F.);
#9329=ORIENTED_EDGE('',*,*,#6672,.F.);
#9330=ORIENTED_EDGE('',*,*,#6058,.F.);
#9331=ORIENTED_EDGE('',*,*,#6665,.T.);
#9332=ORIENTED_EDGE('',*,*,#6057,.F.);
#9333=ORIENTED_EDGE('',*,*,#6673,.F.);
#9334=ORIENTED_EDGE('',*,*,#6108,.F.);
#9335=ORIENTED_EDGE('',*,*,#6674,.F.);
#9336=ORIENTED_EDGE('',*,*,#6667,.T.);
#9337=ORIENTED_EDGE('',*,*,#6675,.F.);
#9338=ORIENTED_EDGE('',*,*,#5864,.T.);
#9339=ORIENTED_EDGE('',*,*,#6676,.F.);
#9340=ORIENTED_EDGE('',*,*,#6668,.T.);
#9341=ORIENTED_EDGE('',*,*,#6677,.F.);
#9342=ORIENTED_EDGE('',*,*,#6669,.T.);
#9343=ORIENTED_EDGE('',*,*,#5618,.F.);
#9344=ORIENTED_EDGE('',*,*,#6678,.F.);
#9345=ORIENTED_EDGE('',*,*,#5861,.F.);
#9346=ORIENTED_EDGE('',*,*,#6670,.T.);
#9347=ORIENTED_EDGE('',*,*,#5857,.F.);
#9348=ORIENTED_EDGE('',*,*,#6679,.F.);
#9349=ORIENTED_EDGE('',*,*,#5959,.F.);
#9350=ORIENTED_EDGE('',*,*,#6671,.T.);
#9351=ORIENTED_EDGE('',*,*,#6091,.T.);
#9352=ORIENTED_EDGE('',*,*,#6680,.F.);
#9353=ORIENTED_EDGE('',*,*,#6672,.T.);
#9354=ORIENTED_EDGE('',*,*,#6681,.F.);
#9355=ORIENTED_EDGE('',*,*,#6673,.T.);
#9356=ORIENTED_EDGE('',*,*,#6682,.F.);
#9357=ORIENTED_EDGE('',*,*,#5442,.T.);
#9358=ORIENTED_EDGE('',*,*,#6106,.F.);
#9359=ORIENTED_EDGE('',*,*,#6683,.F.);
#9360=ORIENTED_EDGE('',*,*,#6066,.F.);
#9361=ORIENTED_EDGE('',*,*,#6675,.T.);
#9362=ORIENTED_EDGE('',*,*,#6063,.F.);
#9363=ORIENTED_EDGE('',*,*,#6684,.F.);
#9364=ORIENTED_EDGE('',*,*,#5865,.F.);
#9365=ORIENTED_EDGE('',*,*,#6674,.T.);
#9366=ORIENTED_EDGE('',*,*,#5871,.F.);
#9367=ORIENTED_EDGE('',*,*,#6685,.F.);
#9368=ORIENTED_EDGE('',*,*,#5615,.F.);
#9369=ORIENTED_EDGE('',*,*,#5614,.F.);
#9370=ORIENTED_EDGE('',*,*,#6677,.T.);
#9371=ORIENTED_EDGE('',*,*,#5616,.F.);
#9372=ORIENTED_EDGE('',*,*,#6686,.F.);
#9373=ORIENTED_EDGE('',*,*,#5855,.F.);
#9374=ORIENTED_EDGE('',*,*,#6676,.T.);
#9375=ORIENTED_EDGE('',*,*,#5854,.F.);
#9376=ORIENTED_EDGE('',*,*,#5438,.F.);
#9377=ORIENTED_EDGE('',*,*,#5976,.F.);
#9378=ORIENTED_EDGE('',*,*,#6678,.T.);
#9379=ORIENTED_EDGE('',*,*,#5983,.F.);
#9380=ORIENTED_EDGE('',*,*,#6687,.F.);
#9381=ORIENTED_EDGE('',*,*,#5862,.F.);
#9382=ORIENTED_EDGE('',*,*,#6688,.F.);
#9383=ORIENTED_EDGE('',*,*,#5863,.F.);
#9384=ORIENTED_EDGE('',*,*,#6689,.F.);
#9385=ORIENTED_EDGE('',*,*,#5842,.F.);
#9386=ORIENTED_EDGE('',*,*,#6679,.T.);
#9387=ORIENTED_EDGE('',*,*,#5856,.F.);
#9388=ORIENTED_EDGE('',*,*,#6690,.F.);
#9389=ORIENTED_EDGE('',*,*,#5895,.F.);
#9390=ORIENTED_EDGE('',*,*,#6680,.T.);
#9391=ORIENTED_EDGE('',*,*,#6090,.F.);
#9392=ORIENTED_EDGE('',*,*,#6691,.F.);
#9393=ORIENTED_EDGE('',*,*,#6059,.F.);
#9394=ORIENTED_EDGE('',*,*,#6682,.T.);
#9395=ORIENTED_EDGE('',*,*,#6056,.F.);
#9396=ORIENTED_EDGE('',*,*,#6692,.F.);
#9397=ORIENTED_EDGE('',*,*,#6052,.F.);
#9398=ORIENTED_EDGE('',*,*,#6681,.T.);
#9399=ORIENTED_EDGE('',*,*,#6051,.F.);
#9400=ORIENTED_EDGE('',*,*,#6693,.F.);
#9401=ORIENTED_EDGE('',*,*,#6109,.F.);
#9402=ORIENTED_EDGE('',*,*,#6694,.F.);
#9403=ORIENTED_EDGE('',*,*,#6105,.F.);
#9404=ORIENTED_EDGE('',*,*,#6695,.F.);
#9405=ORIENTED_EDGE('',*,*,#5532,.F.);
#9406=ORIENTED_EDGE('',*,*,#6683,.T.);
#9407=ORIENTED_EDGE('',*,*,#6694,.T.);
#9408=ORIENTED_EDGE('',*,*,#6696,.F.);
#9409=ORIENTED_EDGE('',*,*,#6684,.T.);
#9410=ORIENTED_EDGE('',*,*,#6062,.F.);
#9411=ORIENTED_EDGE('',*,*,#6697,.F.);
#9412=ORIENTED_EDGE('',*,*,#6084,.F.);
#9413=ORIENTED_EDGE('',*,*,#6685,.T.);
#9414=ORIENTED_EDGE('',*,*,#5870,.T.);
#9415=ORIENTED_EDGE('',*,*,#6698,.F.);
#9416=ORIENTED_EDGE('',*,*,#6686,.T.);
#9417=ORIENTED_EDGE('',*,*,#6689,.T.);
#9418=ORIENTED_EDGE('',*,*,#6687,.T.);
#9419=ORIENTED_EDGE('',*,*,#6699,.F.);
#9420=ORIENTED_EDGE('',*,*,#6690,.T.);
#9421=ORIENTED_EDGE('',*,*,#6688,.T.);
#9422=ORIENTED_EDGE('',*,*,#6700,.F.);
#9423=ORIENTED_EDGE('',*,*,#5896,.T.);
#9424=ORIENTED_EDGE('',*,*,#6691,.T.);
#9425=ORIENTED_EDGE('',*,*,#6089,.T.);
#9426=ORIENTED_EDGE('',*,*,#6701,.F.);
#9427=ORIENTED_EDGE('',*,*,#6702,.F.);
#9428=ORIENTED_EDGE('',*,*,#6703,.F.);
#9429=ORIENTED_EDGE('',*,*,#6692,.T.);
#9430=ORIENTED_EDGE('',*,*,#6704,.F.);
#9431=ORIENTED_EDGE('',*,*,#6695,.T.);
#9432=ORIENTED_EDGE('',*,*,#6693,.T.);
#9433=ORIENTED_EDGE('',*,*,#6705,.F.);
#9434=ORIENTED_EDGE('',*,*,#6696,.T.);
#9435=ORIENTED_EDGE('',*,*,#5531,.F.);
#9436=ORIENTED_EDGE('',*,*,#6706,.F.);
#9437=ORIENTED_EDGE('',*,*,#6067,.F.);
#9438=ORIENTED_EDGE('',*,*,#6697,.T.);
#9439=ORIENTED_EDGE('',*,*,#6061,.F.);
#9440=ORIENTED_EDGE('',*,*,#6707,.F.);
#9441=ORIENTED_EDGE('',*,*,#6080,.F.);
#9442=ORIENTED_EDGE('',*,*,#6698,.T.);
#9443=ORIENTED_EDGE('',*,*,#5869,.F.);
#9444=ORIENTED_EDGE('',*,*,#6708,.F.);
#9445=ORIENTED_EDGE('',*,*,#5849,.F.);
#9446=ORIENTED_EDGE('',*,*,#5436,.T.);
#9447=ORIENTED_EDGE('',*,*,#5853,.F.);
#9448=ORIENTED_EDGE('',*,*,#6709,.F.);
#9449=ORIENTED_EDGE('',*,*,#5979,.F.);
#9450=ORIENTED_EDGE('',*,*,#6699,.T.);
#9451=ORIENTED_EDGE('',*,*,#5982,.F.);
#9452=ORIENTED_EDGE('',*,*,#6710,.F.);
#9453=ORIENTED_EDGE('',*,*,#5837,.F.);
#9454=ORIENTED_EDGE('',*,*,#6700,.T.);
#9455=ORIENTED_EDGE('',*,*,#5841,.F.);
#9456=ORIENTED_EDGE('',*,*,#6711,.F.);
#9457=ORIENTED_EDGE('',*,*,#5897,.F.);
#9458=ORIENTED_EDGE('',*,*,#6712,.F.);
#9459=ORIENTED_EDGE('',*,*,#5715,.F.);
#9460=ORIENTED_EDGE('',*,*,#6701,.T.);
#9461=ORIENTED_EDGE('',*,*,#6088,.F.);
#9462=ORIENTED_EDGE('',*,*,#6702,.T.);
#9463=ORIENTED_EDGE('',*,*,#5714,.F.);
#9464=ORIENTED_EDGE('',*,*,#6713,.F.);
#9465=ORIENTED_EDGE('',*,*,#6060,.F.);
#9466=ORIENTED_EDGE('',*,*,#6704,.T.);
#9467=ORIENTED_EDGE('',*,*,#6055,.F.);
#9468=ORIENTED_EDGE('',*,*,#6714,.F.);
#9469=ORIENTED_EDGE('',*,*,#6223,.F.);
#9470=ORIENTED_EDGE('',*,*,#6703,.T.);
#9471=ORIENTED_EDGE('',*,*,#6222,.F.);
#9472=ORIENTED_EDGE('',*,*,#6715,.F.);
#9473=ORIENTED_EDGE('',*,*,#6053,.F.);
#9474=ORIENTED_EDGE('',*,*,#6705,.T.);
#9475=ORIENTED_EDGE('',*,*,#6054,.F.);
#9476=ORIENTED_EDGE('',*,*,#6716,.F.);
#9477=ORIENTED_EDGE('',*,*,#5526,.F.);
#9478=ORIENTED_EDGE('',*,*,#6707,.T.);
#9479=ORIENTED_EDGE('',*,*,#6706,.T.);
#9480=ORIENTED_EDGE('',*,*,#6717,.F.);
#9481=ORIENTED_EDGE('',*,*,#6081,.T.);
#9482=ORIENTED_EDGE('',*,*,#6708,.T.);
#9483=ORIENTED_EDGE('',*,*,#5880,.F.);
#9484=ORIENTED_EDGE('',*,*,#6718,.F.);
#9485=ORIENTED_EDGE('',*,*,#5850,.F.);
#9486=ORIENTED_EDGE('',*,*,#6719,.F.);
#9487=ORIENTED_EDGE('',*,*,#6709,.T.);
#9488=ORIENTED_EDGE('',*,*,#6720,.F.);
#9489=ORIENTED_EDGE('',*,*,#6721,.F.);
#9490=ORIENTED_EDGE('',*,*,#6710,.T.);
#9491=ORIENTED_EDGE('',*,*,#6722,.F.);
#9492=ORIENTED_EDGE('',*,*,#5890,.T.);
#9493=ORIENTED_EDGE('',*,*,#6711,.T.);
#9494=ORIENTED_EDGE('',*,*,#6723,.F.);
#9495=ORIENTED_EDGE('',*,*,#6724,.F.);
#9496=ORIENTED_EDGE('',*,*,#5727,.T.);
#9497=ORIENTED_EDGE('',*,*,#6204,.F.);
#9498=ORIENTED_EDGE('',*,*,#6725,.F.);
#9499=ORIENTED_EDGE('',*,*,#5709,.F.);
#9500=ORIENTED_EDGE('',*,*,#6714,.T.);
#9501=ORIENTED_EDGE('',*,*,#6713,.T.);
#9502=ORIENTED_EDGE('',*,*,#6726,.F.);
#9503=ORIENTED_EDGE('',*,*,#6716,.T.);
#9504=ORIENTED_EDGE('',*,*,#6715,.T.);
#9505=ORIENTED_EDGE('',*,*,#6727,.F.);
#9506=ORIENTED_EDGE('',*,*,#6717,.T.);
#9507=ORIENTED_EDGE('',*,*,#5530,.F.);
#9508=ORIENTED_EDGE('',*,*,#5529,.F.);
#9509=ORIENTED_EDGE('',*,*,#6728,.F.);
#9510=ORIENTED_EDGE('',*,*,#6082,.F.);
#9511=ORIENTED_EDGE('',*,*,#6718,.T.);
#9512=ORIENTED_EDGE('',*,*,#5877,.F.);
#9513=ORIENTED_EDGE('',*,*,#6729,.F.);
#9514=ORIENTED_EDGE('',*,*,#5851,.F.);
#9515=ORIENTED_EDGE('',*,*,#6720,.T.);
#9516=ORIENTED_EDGE('',*,*,#5852,.F.);
#9517=ORIENTED_EDGE('',*,*,#6730,.F.);
#9518=ORIENTED_EDGE('',*,*,#5828,.F.);
#9519=ORIENTED_EDGE('',*,*,#6719,.T.);
#9520=ORIENTED_EDGE('',*,*,#5827,.F.);
#9521=ORIENTED_EDGE('',*,*,#6731,.F.);
#9522=ORIENTED_EDGE('',*,*,#5980,.F.);
#9523=ORIENTED_EDGE('',*,*,#6722,.T.);
#9524=ORIENTED_EDGE('',*,*,#5981,.F.);
#9525=ORIENTED_EDGE('',*,*,#6732,.F.);
#9526=ORIENTED_EDGE('',*,*,#5833,.F.);
#9527=ORIENTED_EDGE('',*,*,#6721,.T.);
#9528=ORIENTED_EDGE('',*,*,#5832,.F.);
#9529=ORIENTED_EDGE('',*,*,#6733,.F.);
#9530=ORIENTED_EDGE('',*,*,#5838,.F.);
#9531=ORIENTED_EDGE('',*,*,#6734,.F.);
#9532=ORIENTED_EDGE('',*,*,#5839,.F.);
#9533=ORIENTED_EDGE('',*,*,#6735,.F.);
#9534=ORIENTED_EDGE('',*,*,#6317,.F.);
#9535=ORIENTED_EDGE('',*,*,#6723,.T.);
#9536=ORIENTED_EDGE('',*,*,#5840,.F.);
#9537=ORIENTED_EDGE('',*,*,#6736,.F.);
#9538=ORIENTED_EDGE('',*,*,#6302,.F.);
#9539=ORIENTED_EDGE('',*,*,#6724,.T.);
#9540=ORIENTED_EDGE('',*,*,#6301,.F.);
#9541=ORIENTED_EDGE('',*,*,#6737,.F.);
#9542=ORIENTED_EDGE('',*,*,#5891,.F.);
#9543=ORIENTED_EDGE('',*,*,#6725,.T.);
#9544=ORIENTED_EDGE('',*,*,#6201,.F.);
#9545=ORIENTED_EDGE('',*,*,#6738,.F.);
#9546=ORIENTED_EDGE('',*,*,#5710,.F.);
#9547=ORIENTED_EDGE('',*,*,#6726,.T.);
#9548=ORIENTED_EDGE('',*,*,#5713,.F.);
#9549=ORIENTED_EDGE('',*,*,#5434,.F.);
#9550=ORIENTED_EDGE('',*,*,#6224,.F.);
#9551=ORIENTED_EDGE('',*,*,#6727,.T.);
#9552=ORIENTED_EDGE('',*,*,#6221,.F.);
#9553=ORIENTED_EDGE('',*,*,#6739,.F.);
#9554=ORIENTED_EDGE('',*,*,#5527,.F.);
#9555=ORIENTED_EDGE('',*,*,#6740,.F.);
#9556=ORIENTED_EDGE('',*,*,#5528,.F.);
#9557=ORIENTED_EDGE('',*,*,#6741,.F.);
#9558=ORIENTED_EDGE('',*,*,#5696,.F.);
#9559=ORIENTED_EDGE('',*,*,#6728,.T.);
#9560=ORIENTED_EDGE('',*,*,#6740,.T.);
#9561=ORIENTED_EDGE('',*,*,#6742,.F.);
#9562=ORIENTED_EDGE('',*,*,#6083,.T.);
#9563=ORIENTED_EDGE('',*,*,#6729,.T.);
#9564=ORIENTED_EDGE('',*,*,#5876,.T.);
#9565=ORIENTED_EDGE('',*,*,#6743,.F.);
#9566=ORIENTED_EDGE('',*,*,#6730,.T.);
#9567=ORIENTED_EDGE('',*,*,#6732,.T.);
#9568=ORIENTED_EDGE('',*,*,#6731,.T.);
#9569=ORIENTED_EDGE('',*,*,#6744,.F.);
#9570=ORIENTED_EDGE('',*,*,#6735,.T.);
#9571=ORIENTED_EDGE('',*,*,#6733,.T.);
#9572=ORIENTED_EDGE('',*,*,#6745,.F.);
#9573=ORIENTED_EDGE('',*,*,#6736,.T.);
#9574=ORIENTED_EDGE('',*,*,#6734,.T.);
#9575=ORIENTED_EDGE('',*,*,#6746,.F.);
#9576=ORIENTED_EDGE('',*,*,#6737,.T.);
#9577=ORIENTED_EDGE('',*,*,#6300,.F.);
#9578=ORIENTED_EDGE('',*,*,#6747,.F.);
#9579=ORIENTED_EDGE('',*,*,#6308,.F.);
#9580=ORIENTED_EDGE('',*,*,#6738,.T.);
#9581=ORIENTED_EDGE('',*,*,#6200,.T.);
#9582=ORIENTED_EDGE('',*,*,#6748,.F.);
#9583=ORIENTED_EDGE('',*,*,#6749,.F.);
#9584=ORIENTED_EDGE('',*,*,#6741,.T.);
#9585=ORIENTED_EDGE('',*,*,#6739,.T.);
#9586=ORIENTED_EDGE('',*,*,#6750,.F.);
#9587=ORIENTED_EDGE('',*,*,#6751,.F.);
#9588=ORIENTED_EDGE('',*,*,#6076,.F.);
#9589=ORIENTED_EDGE('',*,*,#6742,.T.);
#9590=ORIENTED_EDGE('',*,*,#5695,.F.);
#9591=ORIENTED_EDGE('',*,*,#6743,.T.);
#9592=ORIENTED_EDGE('',*,*,#5875,.F.);
#9593=ORIENTED_EDGE('',*,*,#6752,.F.);
#9594=ORIENTED_EDGE('',*,*,#5829,.F.);
#9595=ORIENTED_EDGE('',*,*,#6744,.T.);
#9596=ORIENTED_EDGE('',*,*,#5826,.F.);
#9597=ORIENTED_EDGE('',*,*,#6753,.F.);
#9598=ORIENTED_EDGE('',*,*,#5834,.F.);
#9599=ORIENTED_EDGE('',*,*,#6745,.T.);
#9600=ORIENTED_EDGE('',*,*,#5831,.F.);
#9601=ORIENTED_EDGE('',*,*,#6754,.F.);
#9602=ORIENTED_EDGE('',*,*,#6318,.F.);
#9603=ORIENTED_EDGE('',*,*,#6746,.T.);
#9604=ORIENTED_EDGE('',*,*,#6316,.F.);
#9605=ORIENTED_EDGE('',*,*,#5428,.F.);
#9606=ORIENTED_EDGE('',*,*,#6303,.F.);
#9607=ORIENTED_EDGE('',*,*,#6747,.T.);
#9608=ORIENTED_EDGE('',*,*,#6299,.F.);
#9609=ORIENTED_EDGE('',*,*,#6755,.F.);
#9610=ORIENTED_EDGE('',*,*,#6197,.F.);
#9611=ORIENTED_EDGE('',*,*,#6748,.T.);
#9612=ORIENTED_EDGE('',*,*,#6199,.F.);
#9613=ORIENTED_EDGE('',*,*,#6756,.F.);
#9614=ORIENTED_EDGE('',*,*,#6184,.F.);
#9615=ORIENTED_EDGE('',*,*,#6749,.T.);
#9616=ORIENTED_EDGE('',*,*,#6183,.F.);
#9617=ORIENTED_EDGE('',*,*,#6757,.F.);
#9618=ORIENTED_EDGE('',*,*,#5711,.F.);
#9619=ORIENTED_EDGE('',*,*,#5432,.T.);
#9620=ORIENTED_EDGE('',*,*,#5712,.F.);
#9621=ORIENTED_EDGE('',*,*,#6758,.F.);
#9622=ORIENTED_EDGE('',*,*,#6217,.F.);
#9623=ORIENTED_EDGE('',*,*,#6750,.T.);
#9624=ORIENTED_EDGE('',*,*,#6220,.F.);
#9625=ORIENTED_EDGE('',*,*,#6759,.F.);
#9626=ORIENTED_EDGE('',*,*,#5697,.F.);
#9627=ORIENTED_EDGE('',*,*,#5729,.T.);
#9628=ORIENTED_EDGE('',*,*,#5702,.F.);
#9629=ORIENTED_EDGE('',*,*,#6760,.F.);
#9630=ORIENTED_EDGE('',*,*,#6194,.F.);
#9631=ORIENTED_EDGE('',*,*,#6752,.T.);
#9632=ORIENTED_EDGE('',*,*,#5874,.T.);
#9633=ORIENTED_EDGE('',*,*,#6761,.F.);
#9634=ORIENTED_EDGE('',*,*,#6762,.F.);
#9635=ORIENTED_EDGE('',*,*,#6754,.T.);
#9636=ORIENTED_EDGE('',*,*,#6753,.T.);
#9637=ORIENTED_EDGE('',*,*,#6763,.F.);
#9638=ORIENTED_EDGE('',*,*,#6198,.T.);
#9639=ORIENTED_EDGE('',*,*,#6755,.T.);
#9640=ORIENTED_EDGE('',*,*,#6764,.F.);
#9641=ORIENTED_EDGE('',*,*,#6756,.T.);
#9642=ORIENTED_EDGE('',*,*,#6758,.T.);
#9643=ORIENTED_EDGE('',*,*,#6757,.T.);
#9644=ORIENTED_EDGE('',*,*,#6765,.F.);
#9645=ORIENTED_EDGE('',*,*,#6759,.T.);
#9646=ORIENTED_EDGE('',*,*,#5516,.F.);
#9647=ORIENTED_EDGE('',*,*,#6766,.F.);
#9648=ORIENTED_EDGE('',*,*,#5698,.F.);
#9649=ORIENTED_EDGE('',*,*,#6760,.T.);
#9650=ORIENTED_EDGE('',*,*,#5701,.F.);
#9651=ORIENTED_EDGE('',*,*,#6767,.F.);
#9652=ORIENTED_EDGE('',*,*,#6191,.F.);
#9653=ORIENTED_EDGE('',*,*,#6761,.T.);
#9654=ORIENTED_EDGE('',*,*,#5873,.F.);
#9655=ORIENTED_EDGE('',*,*,#6768,.F.);
#9656=ORIENTED_EDGE('',*,*,#6291,.F.);
#9657=ORIENTED_EDGE('',*,*,#6762,.T.);
#9658=ORIENTED_EDGE('',*,*,#6298,.F.);
#9659=ORIENTED_EDGE('',*,*,#6769,.F.);
#9660=ORIENTED_EDGE('',*,*,#5830,.F.);
#9661=ORIENTED_EDGE('',*,*,#6763,.T.);
#9662=ORIENTED_EDGE('',*,*,#5825,.F.);
#9663=ORIENTED_EDGE('',*,*,#6770,.F.);
#9664=ORIENTED_EDGE('',*,*,#6314,.F.);
#9665=ORIENTED_EDGE('',*,*,#5430,.T.);
#9666=ORIENTED_EDGE('',*,*,#6323,.F.);
#9667=ORIENTED_EDGE('',*,*,#6771,.F.);
#9668=ORIENTED_EDGE('',*,*,#6304,.F.);
#9669=ORIENTED_EDGE('',*,*,#6764,.T.);
#9670=ORIENTED_EDGE('',*,*,#6305,.F.);
#9671=ORIENTED_EDGE('',*,*,#6772,.F.);
#9672=ORIENTED_EDGE('',*,*,#6185,.F.);
#9673=ORIENTED_EDGE('',*,*,#6765,.T.);
#9674=ORIENTED_EDGE('',*,*,#6182,.F.);
#9675=ORIENTED_EDGE('',*,*,#6773,.F.);
#9676=ORIENTED_EDGE('',*,*,#6218,.F.);
#9677=ORIENTED_EDGE('',*,*,#6766,.T.);
#9678=ORIENTED_EDGE('',*,*,#6216,.F.);
#9679=ORIENTED_EDGE('',*,*,#6774,.F.);
#9680=ORIENTED_EDGE('',*,*,#5699,.F.);
#9681=ORIENTED_EDGE('',*,*,#6775,.F.);
#9682=ORIENTED_EDGE('',*,*,#5700,.F.);
#9683=ORIENTED_EDGE('',*,*,#6776,.F.);
#9684=ORIENTED_EDGE('',*,*,#5513,.F.);
#9685=ORIENTED_EDGE('',*,*,#6767,.T.);
#9686=ORIENTED_EDGE('',*,*,#6775,.T.);
#9687=ORIENTED_EDGE('',*,*,#6777,.F.);
#9688=ORIENTED_EDGE('',*,*,#6192,.T.);
#9689=ORIENTED_EDGE('',*,*,#6768,.T.);
#9690=ORIENTED_EDGE('',*,*,#6306,.F.);
#9691=ORIENTED_EDGE('',*,*,#6778,.F.);
#9692=ORIENTED_EDGE('',*,*,#6292,.F.);
#9693=ORIENTED_EDGE('',*,*,#6770,.T.);
#9694=ORIENTED_EDGE('',*,*,#6769,.T.);
#9695=ORIENTED_EDGE('',*,*,#6779,.F.);
#9696=ORIENTED_EDGE('',*,*,#6772,.T.);
#9697=ORIENTED_EDGE('',*,*,#6771,.T.);
#9698=ORIENTED_EDGE('',*,*,#6780,.F.);
#9699=ORIENTED_EDGE('',*,*,#6781,.F.);
#9700=ORIENTED_EDGE('',*,*,#6773,.T.);
#9701=ORIENTED_EDGE('',*,*,#5426,.F.);
#9702=ORIENTED_EDGE('',*,*,#6776,.T.);
#9703=ORIENTED_EDGE('',*,*,#6774,.T.);
#9704=ORIENTED_EDGE('',*,*,#6782,.F.);
#9705=ORIENTED_EDGE('',*,*,#6777,.T.);
#9706=ORIENTED_EDGE('',*,*,#5512,.F.);
#9707=ORIENTED_EDGE('',*,*,#5511,.F.);
#9708=ORIENTED_EDGE('',*,*,#6783,.F.);
#9709=ORIENTED_EDGE('',*,*,#6193,.F.);
#9710=ORIENTED_EDGE('',*,*,#6778,.T.);
#9711=ORIENTED_EDGE('',*,*,#6187,.F.);
#9712=ORIENTED_EDGE('',*,*,#6784,.F.);
#9713=ORIENTED_EDGE('',*,*,#6293,.F.);
#9714=ORIENTED_EDGE('',*,*,#6779,.T.);
#9715=ORIENTED_EDGE('',*,*,#6297,.F.);
#9716=ORIENTED_EDGE('',*,*,#6785,.F.);
#9717=ORIENTED_EDGE('',*,*,#6315,.F.);
#9718=ORIENTED_EDGE('',*,*,#6780,.T.);
#9719=ORIENTED_EDGE('',*,*,#6322,.F.);
#9720=ORIENTED_EDGE('',*,*,#6786,.F.);
#9721=ORIENTED_EDGE('',*,*,#6181,.F.);
#9722=ORIENTED_EDGE('',*,*,#6781,.T.);
#9723=ORIENTED_EDGE('',*,*,#6179,.F.);
#9724=ORIENTED_EDGE('',*,*,#6787,.F.);
#9725=ORIENTED_EDGE('',*,*,#6219,.F.);
#9726=ORIENTED_EDGE('',*,*,#6782,.T.);
#9727=ORIENTED_EDGE('',*,*,#6215,.F.);
#9728=ORIENTED_EDGE('',*,*,#6788,.F.);
#9729=ORIENTED_EDGE('',*,*,#5514,.F.);
#9730=ORIENTED_EDGE('',*,*,#6186,.T.);
#9731=ORIENTED_EDGE('',*,*,#6783,.T.);
#9732=ORIENTED_EDGE('',*,*,#6789,.F.);
#9733=ORIENTED_EDGE('',*,*,#6784,.T.);
#9734=ORIENTED_EDGE('',*,*,#6785,.T.);
#9735=ORIENTED_EDGE('',*,*,#6296,.F.);
#9736=ORIENTED_EDGE('',*,*,#6790,.F.);
#9737=ORIENTED_EDGE('',*,*,#5497,.F.);
#9738=ORIENTED_EDGE('',*,*,#5424,.T.);
#9739=ORIENTED_EDGE('',*,*,#6786,.T.);
#9740=ORIENTED_EDGE('',*,*,#6791,.F.);
#9741=ORIENTED_EDGE('',*,*,#6788,.T.);
#9742=ORIENTED_EDGE('',*,*,#6787,.T.);
#9743=ORIENTED_EDGE('',*,*,#5422,.F.);
#9744=ORIENTED_EDGE('',*,*,#6789,.T.);
#9745=ORIENTED_EDGE('',*,*,#5510,.F.);
#9746=ORIENTED_EDGE('',*,*,#6792,.F.);
#9747=ORIENTED_EDGE('',*,*,#6294,.F.);
#9748=ORIENTED_EDGE('',*,*,#6790,.T.);
#9749=ORIENTED_EDGE('',*,*,#6295,.F.);
#9750=ORIENTED_EDGE('',*,*,#6793,.F.);
#9751=ORIENTED_EDGE('',*,*,#6319,.F.);
#9752=ORIENTED_EDGE('',*,*,#6791,.T.);
#9753=ORIENTED_EDGE('',*,*,#6321,.F.);
#9754=ORIENTED_EDGE('',*,*,#6794,.F.);
#9755=ORIENTED_EDGE('',*,*,#6180,.F.);
#9756=ORIENTED_EDGE('',*,*,#6793,.T.);
#9757=ORIENTED_EDGE('',*,*,#6792,.T.);
#9758=ORIENTED_EDGE('',*,*,#6795,.F.);
#9759=ORIENTED_EDGE('',*,*,#5420,.T.);
#9760=ORIENTED_EDGE('',*,*,#6794,.T.);
#9761=ORIENTED_EDGE('',*,*,#6796,.F.);
#9762=ORIENTED_EDGE('',*,*,#6795,.T.);
#9763=ORIENTED_EDGE('',*,*,#5509,.F.);
#9764=ORIENTED_EDGE('',*,*,#6796,.T.);
#9765=ORIENTED_EDGE('',*,*,#6320,.F.);
#9766=ORIENTED_EDGE('',*,*,#6797,.F.);
#9767=ORIENTED_EDGE('',*,*,#6214,.T.);
#9768=ORIENTED_EDGE('',*,*,#6798,.T.);
#9769=ORIENTED_EDGE('',*,*,#6799,.T.);
#9770=ORIENTED_EDGE('',*,*,#6799,.F.);
#9771=ORIENTED_EDGE('',*,*,#6800,.T.);
#9772=ORIENTED_EDGE('',*,*,#6801,.T.);
#9773=ORIENTED_EDGE('',*,*,#6802,.T.);
#9774=ORIENTED_EDGE('',*,*,#6802,.F.);
#9775=ORIENTED_EDGE('',*,*,#6803,.T.);
#9776=ORIENTED_EDGE('',*,*,#5603,.T.);
#9777=ORIENTED_EDGE('',*,*,#6804,.T.);
#9778=ORIENTED_EDGE('',*,*,#6804,.F.);
#9779=ORIENTED_EDGE('',*,*,#5545,.T.);
#9780=ORIENTED_EDGE('',*,*,#6805,.T.);
#9781=ORIENTED_EDGE('',*,*,#6806,.T.);
#9782=ORIENTED_EDGE('',*,*,#6806,.F.);
#9783=ORIENTED_EDGE('',*,*,#6807,.T.);
#9784=ORIENTED_EDGE('',*,*,#6808,.F.);
#9785=ORIENTED_EDGE('',*,*,#6809,.T.);
#9786=ORIENTED_EDGE('',*,*,#6810,.F.);
#9787=ORIENTED_EDGE('',*,*,#6811,.T.);
#9788=ORIENTED_EDGE('',*,*,#6100,.T.);
#9789=ORIENTED_EDGE('',*,*,#6812,.T.);
#9790=ORIENTED_EDGE('',*,*,#6812,.F.);
#9791=ORIENTED_EDGE('',*,*,#6104,.T.);
#9792=ORIENTED_EDGE('',*,*,#6813,.T.);
#9793=ORIENTED_EDGE('',*,*,#6814,.T.);
#9794=ORIENTED_EDGE('',*,*,#6814,.F.);
#9795=ORIENTED_EDGE('',*,*,#6815,.T.);
#9796=ORIENTED_EDGE('',*,*,#6816,.T.);
#9797=ORIENTED_EDGE('',*,*,#6817,.T.);
#9798=ORIENTED_EDGE('',*,*,#6817,.F.);
#9799=ORIENTED_EDGE('',*,*,#6818,.T.);
#9800=ORIENTED_EDGE('',*,*,#5606,.T.);
#9801=ORIENTED_EDGE('',*,*,#6819,.T.);
#9802=ORIENTED_EDGE('',*,*,#6819,.F.);
#9803=ORIENTED_EDGE('',*,*,#5605,.T.);
#9804=ORIENTED_EDGE('',*,*,#6820,.F.);
#9805=ORIENTED_EDGE('',*,*,#6821,.T.);
#9806=ORIENTED_EDGE('',*,*,#6822,.F.);
#9807=ORIENTED_EDGE('',*,*,#5542,.T.);
#9808=ORIENTED_EDGE('',*,*,#6823,.T.);
#9809=ORIENTED_EDGE('',*,*,#6824,.T.);
#9810=ORIENTED_EDGE('',*,*,#6824,.F.);
#9811=ORIENTED_EDGE('',*,*,#6825,.T.);
#9812=ORIENTED_EDGE('',*,*,#6826,.T.);
#9813=ORIENTED_EDGE('',*,*,#6827,.T.);
#9814=ORIENTED_EDGE('',*,*,#6827,.F.);
#9815=ORIENTED_EDGE('',*,*,#6828,.T.);
#9816=ORIENTED_EDGE('',*,*,#5764,.T.);
#9817=ORIENTED_EDGE('',*,*,#6829,.T.);
#9818=ORIENTED_EDGE('',*,*,#6829,.F.);
#9819=ORIENTED_EDGE('',*,*,#5763,.T.);
#9820=ORIENTED_EDGE('',*,*,#6830,.T.);
#9821=ORIENTED_EDGE('',*,*,#6831,.T.);
#9822=ORIENTED_EDGE('',*,*,#6831,.F.);
#9823=ORIENTED_EDGE('',*,*,#6832,.T.);
#9824=ORIENTED_EDGE('',*,*,#6833,.F.);
#9825=ORIENTED_EDGE('',*,*,#6834,.T.);
#9826=ORIENTED_EDGE('',*,*,#6835,.F.);
#9827=ORIENTED_EDGE('',*,*,#6836,.T.);
#9828=ORIENTED_EDGE('',*,*,#5965,.T.);
#9829=ORIENTED_EDGE('',*,*,#6837,.T.);
#9830=ORIENTED_EDGE('',*,*,#6837,.F.);
#9831=ORIENTED_EDGE('',*,*,#5969,.T.);
#9832=ORIENTED_EDGE('',*,*,#6838,.T.);
#9833=ORIENTED_EDGE('',*,*,#6839,.T.);
#9834=ORIENTED_EDGE('',*,*,#6839,.F.);
#9835=ORIENTED_EDGE('',*,*,#6840,.T.);
#9836=ORIENTED_EDGE('',*,*,#6841,.F.);
#9837=ORIENTED_EDGE('',*,*,#6842,.T.);
#9838=ORIENTED_EDGE('',*,*,#6842,.F.);
#9839=ORIENTED_EDGE('',*,*,#6843,.F.);
#9840=ORIENTED_EDGE('',*,*,#5540,.T.);
#9841=ORIENTED_EDGE('',*,*,#6844,.T.);
#9842=ORIENTED_EDGE('',*,*,#6844,.F.);
#9843=ORIENTED_EDGE('',*,*,#5608,.T.);
#9844=ORIENTED_EDGE('',*,*,#6845,.F.);
#9845=ORIENTED_EDGE('',*,*,#6846,.T.);
#9846=ORIENTED_EDGE('',*,*,#6847,.F.);
#9847=ORIENTED_EDGE('',*,*,#5676,.F.);
#9848=ORIENTED_EDGE('',*,*,#6848,.F.);
#9849=ORIENTED_EDGE('',*,*,#5967,.F.);
#9850=ORIENTED_EDGE('',*,*,#5677,.T.);
#9851=ORIENTED_EDGE('',*,*,#6847,.T.);
#9852=ORIENTED_EDGE('',*,*,#6849,.F.);
#9853=ORIENTED_EDGE('',*,*,#6850,.F.);
#9854=ORIENTED_EDGE('',*,*,#6851,.F.);
#9855=ORIENTED_EDGE('',*,*,#6852,.F.);
#9856=ORIENTED_EDGE('',*,*,#6848,.T.);
#9857=ORIENTED_EDGE('',*,*,#5675,.T.);
#9858=ORIENTED_EDGE('',*,*,#6852,.T.);
#9859=ORIENTED_EDGE('',*,*,#5963,.F.);
#9860=ORIENTED_EDGE('',*,*,#6840,.F.);
#9861=ORIENTED_EDGE('',*,*,#6838,.F.);
#9862=ORIENTED_EDGE('',*,*,#5968,.F.);
#9863=ORIENTED_EDGE('',*,*,#6849,.T.);
#9864=ORIENTED_EDGE('',*,*,#5966,.F.);
#9865=ORIENTED_EDGE('',*,*,#6836,.F.);
#9866=ORIENTED_EDGE('',*,*,#6853,.F.);
#9867=ORIENTED_EDGE('',*,*,#6096,.F.);
#9868=ORIENTED_EDGE('',*,*,#6850,.T.);
#9869=ORIENTED_EDGE('',*,*,#6099,.F.);
#9870=ORIENTED_EDGE('',*,*,#6854,.F.);
#9871=ORIENTED_EDGE('',*,*,#5678,.F.);
#9872=ORIENTED_EDGE('',*,*,#6855,.F.);
#9873=ORIENTED_EDGE('',*,*,#5680,.F.);
#9874=ORIENTED_EDGE('',*,*,#6856,.F.);
#9875=ORIENTED_EDGE('',*,*,#6102,.F.);
#9876=ORIENTED_EDGE('',*,*,#6851,.T.);
#9877=ORIENTED_EDGE('',*,*,#5674,.F.);
#9878=ORIENTED_EDGE('',*,*,#6857,.F.);
#9879=ORIENTED_EDGE('',*,*,#5964,.F.);
#9880=ORIENTED_EDGE('',*,*,#6853,.T.);
#9881=ORIENTED_EDGE('',*,*,#6835,.T.);
#9882=ORIENTED_EDGE('',*,*,#6846,.F.);
#9883=ORIENTED_EDGE('',*,*,#6858,.F.);
#9884=ORIENTED_EDGE('',*,*,#5679,.T.);
#9885=ORIENTED_EDGE('',*,*,#6854,.T.);
#9886=ORIENTED_EDGE('',*,*,#6859,.F.);
#9887=ORIENTED_EDGE('',*,*,#6856,.T.);
#9888=ORIENTED_EDGE('',*,*,#5665,.T.);
#9889=ORIENTED_EDGE('',*,*,#6855,.T.);
#9890=ORIENTED_EDGE('',*,*,#6860,.F.);
#9891=ORIENTED_EDGE('',*,*,#6861,.F.);
#9892=ORIENTED_EDGE('',*,*,#6862,.F.);
#9893=ORIENTED_EDGE('',*,*,#6863,.F.);
#9894=ORIENTED_EDGE('',*,*,#6857,.T.);
#9895=ORIENTED_EDGE('',*,*,#5673,.T.);
#9896=ORIENTED_EDGE('',*,*,#6863,.T.);
#9897=ORIENTED_EDGE('',*,*,#5765,.F.);
#9898=ORIENTED_EDGE('',*,*,#6828,.F.);
#9899=ORIENTED_EDGE('',*,*,#6826,.F.);
#9900=ORIENTED_EDGE('',*,*,#5961,.F.);
#9901=ORIENTED_EDGE('',*,*,#6841,.T.);
#9902=ORIENTED_EDGE('',*,*,#5962,.F.);
#9903=ORIENTED_EDGE('',*,*,#6825,.F.);
#9904=ORIENTED_EDGE('',*,*,#6823,.F.);
#9905=ORIENTED_EDGE('',*,*,#5541,.F.);
#9906=ORIENTED_EDGE('',*,*,#6843,.T.);
#9907=ORIENTED_EDGE('',*,*,#6845,.T.);
#9908=ORIENTED_EDGE('',*,*,#5607,.F.);
#9909=ORIENTED_EDGE('',*,*,#6818,.F.);
#9910=ORIENTED_EDGE('',*,*,#6816,.F.);
#9911=ORIENTED_EDGE('',*,*,#6097,.F.);
#9912=ORIENTED_EDGE('',*,*,#6858,.T.);
#9913=ORIENTED_EDGE('',*,*,#6859,.T.);
#9914=ORIENTED_EDGE('',*,*,#6098,.F.);
#9915=ORIENTED_EDGE('',*,*,#6815,.F.);
#9916=ORIENTED_EDGE('',*,*,#6813,.F.);
#9917=ORIENTED_EDGE('',*,*,#6103,.F.);
#9918=ORIENTED_EDGE('',*,*,#6860,.T.);
#9919=ORIENTED_EDGE('',*,*,#6101,.F.);
#9920=ORIENTED_EDGE('',*,*,#6811,.F.);
#9921=ORIENTED_EDGE('',*,*,#6864,.F.);
#9922=ORIENTED_EDGE('',*,*,#6206,.F.);
#9923=ORIENTED_EDGE('',*,*,#6861,.T.);
#9924=ORIENTED_EDGE('',*,*,#6209,.F.);
#9925=ORIENTED_EDGE('',*,*,#6865,.F.);
#9926=ORIENTED_EDGE('',*,*,#5666,.F.);
#9927=ORIENTED_EDGE('',*,*,#6862,.T.);
#9928=ORIENTED_EDGE('',*,*,#5672,.F.);
#9929=ORIENTED_EDGE('',*,*,#6866,.F.);
#9930=ORIENTED_EDGE('',*,*,#5766,.F.);
#9931=ORIENTED_EDGE('',*,*,#6832,.F.);
#9932=ORIENTED_EDGE('',*,*,#6830,.F.);
#9933=ORIENTED_EDGE('',*,*,#5767,.F.);
#9934=ORIENTED_EDGE('',*,*,#6867,.F.);
#9935=ORIENTED_EDGE('',*,*,#6312,.F.);
#9936=ORIENTED_EDGE('',*,*,#5543,.T.);
#9937=ORIENTED_EDGE('',*,*,#6822,.T.);
#9938=ORIENTED_EDGE('',*,*,#6834,.F.);
#9939=ORIENTED_EDGE('',*,*,#6868,.F.);
#9940=ORIENTED_EDGE('',*,*,#6864,.T.);
#9941=ORIENTED_EDGE('',*,*,#6810,.T.);
#9942=ORIENTED_EDGE('',*,*,#6821,.F.);
#9943=ORIENTED_EDGE('',*,*,#6869,.F.);
#9944=ORIENTED_EDGE('',*,*,#5667,.T.);
#9945=ORIENTED_EDGE('',*,*,#6865,.T.);
#9946=ORIENTED_EDGE('',*,*,#6870,.F.);
#9947=ORIENTED_EDGE('',*,*,#6871,.F.);
#9948=ORIENTED_EDGE('',*,*,#6866,.T.);
#9949=ORIENTED_EDGE('',*,*,#5671,.T.);
#9950=ORIENTED_EDGE('',*,*,#6872,.F.);
#9951=ORIENTED_EDGE('',*,*,#6867,.T.);
#9952=ORIENTED_EDGE('',*,*,#6833,.T.);
#9953=ORIENTED_EDGE('',*,*,#6311,.F.);
#9954=ORIENTED_EDGE('',*,*,#6807,.F.);
#9955=ORIENTED_EDGE('',*,*,#6805,.F.);
#9956=ORIENTED_EDGE('',*,*,#5544,.F.);
#9957=ORIENTED_EDGE('',*,*,#6868,.T.);
#9958=ORIENTED_EDGE('',*,*,#6820,.T.);
#9959=ORIENTED_EDGE('',*,*,#5604,.F.);
#9960=ORIENTED_EDGE('',*,*,#6803,.F.);
#9961=ORIENTED_EDGE('',*,*,#6801,.F.);
#9962=ORIENTED_EDGE('',*,*,#6207,.F.);
#9963=ORIENTED_EDGE('',*,*,#6869,.T.);
#9964=ORIENTED_EDGE('',*,*,#6870,.T.);
#9965=ORIENTED_EDGE('',*,*,#6208,.F.);
#9966=ORIENTED_EDGE('',*,*,#6800,.F.);
#9967=ORIENTED_EDGE('',*,*,#6798,.F.);
#9968=ORIENTED_EDGE('',*,*,#6213,.F.);
#9969=ORIENTED_EDGE('',*,*,#6871,.T.);
#9970=ORIENTED_EDGE('',*,*,#6212,.F.);
#9971=ORIENTED_EDGE('',*,*,#6873,.F.);
#9972=ORIENTED_EDGE('',*,*,#5668,.F.);
#9973=ORIENTED_EDGE('',*,*,#6872,.T.);
#9974=ORIENTED_EDGE('',*,*,#5670,.F.);
#9975=ORIENTED_EDGE('',*,*,#6874,.F.);
#9976=ORIENTED_EDGE('',*,*,#6313,.F.);
#9977=ORIENTED_EDGE('',*,*,#6210,.T.);
#9978=ORIENTED_EDGE('',*,*,#6797,.T.);
#9979=ORIENTED_EDGE('',*,*,#6809,.F.);
#9980=ORIENTED_EDGE('',*,*,#6875,.F.);
#9981=ORIENTED_EDGE('',*,*,#5669,.T.);
#9982=ORIENTED_EDGE('',*,*,#6873,.T.);
#9983=ORIENTED_EDGE('',*,*,#6876,.F.);
#9984=ORIENTED_EDGE('',*,*,#6874,.T.);
#9985=ORIENTED_EDGE('',*,*,#6808,.T.);
#9986=ORIENTED_EDGE('',*,*,#6310,.F.);
#9987=ORIENTED_EDGE('',*,*,#6876,.T.);
#9988=ORIENTED_EDGE('',*,*,#6211,.F.);
#9989=ORIENTED_EDGE('',*,*,#6875,.T.);
#9990=ORIENTED_EDGE('',*,*,#6877,.F.);
#9991=ORIENTED_EDGE('',*,*,#5926,.F.);
#9992=ORIENTED_EDGE('',*,*,#6878,.F.);
#9993=ORIENTED_EDGE('',*,*,#6085,.F.);
#9994=ORIENTED_EDGE('',*,*,#6878,.T.);
#9995=ORIENTED_EDGE('',*,*,#5925,.F.);
#9996=ORIENTED_EDGE('',*,*,#6879,.F.);
#9997=ORIENTED_EDGE('',*,*,#5867,.F.);
#9998=ORIENTED_EDGE('',*,*,#6880,.F.);
#9999=ORIENTED_EDGE('',*,*,#5898,.F.);
#10000=ORIENTED_EDGE('',*,*,#6877,.T.);
#10001=ORIENTED_EDGE('',*,*,#6078,.F.);
#10002=ORIENTED_EDGE('',*,*,#6879,.T.);
#10003=ORIENTED_EDGE('',*,*,#5924,.F.);
#10004=ORIENTED_EDGE('',*,*,#6881,.F.);
#10005=ORIENTED_EDGE('',*,*,#5881,.F.);
#10006=ORIENTED_EDGE('',*,*,#5732,.T.);
#10007=ORIENTED_EDGE('',*,*,#6195,.F.);
#10008=ORIENTED_EDGE('',*,*,#6882,.F.);
#10009=ORIENTED_EDGE('',*,*,#5920,.F.);
#10010=ORIENTED_EDGE('',*,*,#6881,.T.);
#10011=ORIENTED_EDGE('',*,*,#5923,.F.);
#10012=ORIENTED_EDGE('',*,*,#6883,.F.);
#10013=ORIENTED_EDGE('',*,*,#5879,.F.);
#10014=ORIENTED_EDGE('',*,*,#6882,.T.);
#10015=ORIENTED_EDGE('',*,*,#6189,.F.);
#10016=ORIENTED_EDGE('',*,*,#6884,.F.);
#10017=ORIENTED_EDGE('',*,*,#5921,.F.);
#10018=ORIENTED_EDGE('',*,*,#6883,.T.);
#10019=ORIENTED_EDGE('',*,*,#5922,.F.);
#10020=ORIENTED_EDGE('',*,*,#6884,.T.);
#10021=ORIENTED_EDGE('',*,*,#6307,.F.);
#10022=ORIENTED_EDGE('',*,*,#6885,.F.);
#10023=ORIENTED_EDGE('',*,*,#6095,.F.);
#10024=ORIENTED_EDGE('',*,*,#6886,.F.);
#10025=ORIENTED_EDGE('',*,*,#5639,.F.);
#10026=ORIENTED_EDGE('',*,*,#6886,.T.);
#10027=ORIENTED_EDGE('',*,*,#5889,.F.);
#10028=ORIENTED_EDGE('',*,*,#6887,.F.);
#10029=ORIENTED_EDGE('',*,*,#5640,.F.);
#10030=ORIENTED_EDGE('',*,*,#6888,.F.);
#10031=ORIENTED_EDGE('',*,*,#6086,.F.);
#10032=ORIENTED_EDGE('',*,*,#6885,.T.);
#10033=ORIENTED_EDGE('',*,*,#5638,.F.);
#10034=ORIENTED_EDGE('',*,*,#6887,.T.);
#10035=ORIENTED_EDGE('',*,*,#5960,.F.);
#10036=ORIENTED_EDGE('',*,*,#6889,.F.);
#10037=ORIENTED_EDGE('',*,*,#5641,.F.);
#10038=ORIENTED_EDGE('',*,*,#5734,.T.);
#10039=ORIENTED_EDGE('',*,*,#5645,.F.);
#10040=ORIENTED_EDGE('',*,*,#6890,.F.);
#10041=ORIENTED_EDGE('',*,*,#6205,.F.);
#10042=ORIENTED_EDGE('',*,*,#6889,.T.);
#10043=ORIENTED_EDGE('',*,*,#5893,.F.);
#10044=ORIENTED_EDGE('',*,*,#6891,.F.);
#10045=ORIENTED_EDGE('',*,*,#5642,.F.);
#10046=ORIENTED_EDGE('',*,*,#6890,.T.);
#10047=ORIENTED_EDGE('',*,*,#5644,.F.);
#10048=ORIENTED_EDGE('',*,*,#6892,.F.);
#10049=ORIENTED_EDGE('',*,*,#6203,.F.);
#10050=ORIENTED_EDGE('',*,*,#6891,.T.);
#10051=ORIENTED_EDGE('',*,*,#6309,.F.);
#10052=ORIENTED_EDGE('',*,*,#6892,.T.);
#10053=ORIENTED_EDGE('',*,*,#5643,.F.);
#10054=ORIENTED_EDGE('',*,*,#6893,.F.);
#10055=ORIENTED_EDGE('',*,*,#5629,.F.);
#10056=ORIENTED_EDGE('',*,*,#5402,.F.);
#10057=ORIENTED_EDGE('',*,*,#5505,.F.);
#10058=ORIENTED_EDGE('',*,*,#6893,.T.);
#10059=ORIENTED_EDGE('',*,*,#6264,.F.);
#10060=ORIENTED_EDGE('',*,*,#6894,.F.);
#10061=ORIENTED_EDGE('',*,*,#5630,.F.);
#10062=ORIENTED_EDGE('',*,*,#6895,.F.);
#10063=ORIENTED_EDGE('',*,*,#5635,.F.);
#10064=ORIENTED_EDGE('',*,*,#6896,.F.);
#10065=ORIENTED_EDGE('',*,*,#6246,.F.);
#10066=ORIENTED_EDGE('',*,*,#6894,.T.);
#10067=ORIENTED_EDGE('',*,*,#6248,.F.);
#10068=ORIENTED_EDGE('',*,*,#6897,.F.);
#10069=ORIENTED_EDGE('',*,*,#5631,.F.);
#10070=ORIENTED_EDGE('',*,*,#6896,.T.);
#10071=ORIENTED_EDGE('',*,*,#5634,.F.);
#10072=ORIENTED_EDGE('',*,*,#6898,.F.);
#10073=ORIENTED_EDGE('',*,*,#5501,.F.);
#10074=ORIENTED_EDGE('',*,*,#6897,.T.);
#10075=ORIENTED_EDGE('',*,*,#6262,.F.);
#10076=ORIENTED_EDGE('',*,*,#6899,.F.);
#10077=ORIENTED_EDGE('',*,*,#5632,.F.);
#10078=ORIENTED_EDGE('',*,*,#6898,.T.);
#10079=ORIENTED_EDGE('',*,*,#5633,.F.);
#10080=ORIENTED_EDGE('',*,*,#6899,.T.);
#10081=ORIENTED_EDGE('',*,*,#6241,.F.);
#10082=ORIENTED_EDGE('',*,*,#6900,.F.);
#10083=ORIENTED_EDGE('',*,*,#5503,.F.);
#10084=ORIENTED_EDGE('',*,*,#5396,.F.);
#10085=ORIENTED_EDGE('',*,*,#6258,.F.);
#10086=ORIENTED_EDGE('',*,*,#6900,.T.);
#10087=ORIENTED_EDGE('',*,*,#6257,.F.);
#10088=ORIENTED_EDGE('',*,*,#6901,.F.);
#10089=ORIENTED_EDGE('',*,*,#6263,.F.);
#10090=ORIENTED_EDGE('',*,*,#6252,.F.);
#10091=ORIENTED_EDGE('',*,*,#6902,.T.);
#10092=ORIENTED_EDGE('',*,*,#6244,.F.);
#10093=ORIENTED_EDGE('',*,*,#6903,.F.);
#10094=ORIENTED_EDGE('',*,*,#6901,.T.);
#10095=ORIENTED_EDGE('',*,*,#6256,.F.);
#10096=ORIENTED_EDGE('',*,*,#6904,.F.);
#10097=ORIENTED_EDGE('',*,*,#6250,.F.);
#10098=ORIENTED_EDGE('',*,*,#6903,.T.);
#10099=ORIENTED_EDGE('',*,*,#5499,.F.);
#10100=ORIENTED_EDGE('',*,*,#6905,.F.);
#10101=ORIENTED_EDGE('',*,*,#6253,.F.);
#10102=ORIENTED_EDGE('',*,*,#6904,.T.);
#10103=ORIENTED_EDGE('',*,*,#6255,.F.);
#10104=ORIENTED_EDGE('',*,*,#6906,.F.);
#10105=ORIENTED_EDGE('',*,*,#6261,.F.);
#10106=ORIENTED_EDGE('',*,*,#6905,.T.);
#10107=ORIENTED_EDGE('',*,*,#6243,.F.);
#10108=ORIENTED_EDGE('',*,*,#6906,.T.);
#10109=ORIENTED_EDGE('',*,*,#6254,.F.);
#10110=ORIENTED_EDGE('',*,*,#5381,.T.);
#10111=ORIENTED_EDGE('',*,*,#5656,.F.);
#10112=ORIENTED_EDGE('',*,*,#6907,.F.);
#10113=ORIENTED_EDGE('',*,*,#6148,.F.);
#10114=ORIENTED_EDGE('',*,*,#5379,.T.);
#10115=ORIENTED_EDGE('',*,*,#6150,.F.);
#10116=ORIENTED_EDGE('',*,*,#6908,.F.);
#10117=ORIENTED_EDGE('',*,*,#5657,.F.);
#10118=ORIENTED_EDGE('',*,*,#6907,.T.);
#10119=ORIENTED_EDGE('',*,*,#5655,.F.);
#10120=ORIENTED_EDGE('',*,*,#6909,.F.);
#10121=ORIENTED_EDGE('',*,*,#6135,.F.);
#10122=ORIENTED_EDGE('',*,*,#6908,.T.);
#10123=ORIENTED_EDGE('',*,*,#6138,.F.);
#10124=ORIENTED_EDGE('',*,*,#5375,.F.);
#10125=ORIENTED_EDGE('',*,*,#5658,.F.);
#10126=ORIENTED_EDGE('',*,*,#6909,.T.);
#10127=ORIENTED_EDGE('',*,*,#5654,.F.);
#10128=ORIENTED_EDGE('',*,*,#6910,.F.);
#10129=ORIENTED_EDGE('',*,*,#5520,.F.);
#10130=ORIENTED_EDGE('',*,*,#6910,.T.);
#10131=ORIENTED_EDGE('',*,*,#5653,.F.);
#10132=ORIENTED_EDGE('',*,*,#5377,.T.);
#10133=ORIENTED_EDGE('',*,*,#6131,.F.);
#10134=ORIENTED_EDGE('',*,*,#5371,.T.);
#10135=ORIENTED_EDGE('',*,*,#6147,.F.);
#10136=ORIENTED_EDGE('',*,*,#6911,.F.);
#10137=ORIENTED_EDGE('',*,*,#6141,.F.);
#10138=ORIENTED_EDGE('',*,*,#5373,.T.);
#10139=ORIENTED_EDGE('',*,*,#6146,.F.);
#10140=ORIENTED_EDGE('',*,*,#6912,.F.);
#10141=ORIENTED_EDGE('',*,*,#6149,.F.);
#10142=ORIENTED_EDGE('',*,*,#6911,.T.);
#10143=ORIENTED_EDGE('',*,*,#6136,.F.);
#10144=ORIENTED_EDGE('',*,*,#6913,.F.);
#10145=ORIENTED_EDGE('',*,*,#6142,.F.);
#10146=ORIENTED_EDGE('',*,*,#6912,.T.);
#10147=ORIENTED_EDGE('',*,*,#6145,.F.);
#10148=ORIENTED_EDGE('',*,*,#5369,.F.);
#10149=ORIENTED_EDGE('',*,*,#6140,.F.);
#10150=ORIENTED_EDGE('',*,*,#6913,.T.);
#10151=ORIENTED_EDGE('',*,*,#5518,.F.);
#10152=ORIENTED_EDGE('',*,*,#6914,.F.);
#10153=ORIENTED_EDGE('',*,*,#6143,.F.);
#10154=ORIENTED_EDGE('',*,*,#6914,.T.);
#10155=ORIENTED_EDGE('',*,*,#6133,.F.);
#10156=ORIENTED_EDGE('',*,*,#5367,.T.);
#10157=ORIENTED_EDGE('',*,*,#6144,.F.);
#10158=ORIENTED_EDGE('',*,*,#5349,.T.);
#10159=ORIENTED_EDGE('',*,*,#5661,.F.);
#10160=ORIENTED_EDGE('',*,*,#6915,.F.);
#10161=ORIENTED_EDGE('',*,*,#6021,.F.);
#10162=ORIENTED_EDGE('',*,*,#5347,.T.);
#10163=ORIENTED_EDGE('',*,*,#6023,.F.);
#10164=ORIENTED_EDGE('',*,*,#6916,.F.);
#10165=ORIENTED_EDGE('',*,*,#5662,.F.);
#10166=ORIENTED_EDGE('',*,*,#6915,.T.);
#10167=ORIENTED_EDGE('',*,*,#5660,.F.);
#10168=ORIENTED_EDGE('',*,*,#5345,.F.);
#10169=ORIENTED_EDGE('',*,*,#6006,.F.);
#10170=ORIENTED_EDGE('',*,*,#6916,.T.);
#10171=ORIENTED_EDGE('',*,*,#6009,.F.);
#10172=ORIENTED_EDGE('',*,*,#6917,.F.);
#10173=ORIENTED_EDGE('',*,*,#5663,.F.);
#10174=ORIENTED_EDGE('',*,*,#6917,.T.);
#10175=ORIENTED_EDGE('',*,*,#6019,.F.);
#10176=ORIENTED_EDGE('',*,*,#6918,.F.);
#10177=ORIENTED_EDGE('',*,*,#5664,.F.);
#10178=ORIENTED_EDGE('',*,*,#5343,.T.);
#10179=ORIENTED_EDGE('',*,*,#5659,.F.);
#10180=ORIENTED_EDGE('',*,*,#6918,.T.);
#10181=ORIENTED_EDGE('',*,*,#6002,.F.);
#10182=ORIENTED_EDGE('',*,*,#5339,.T.);
#10183=ORIENTED_EDGE('',*,*,#6020,.F.);
#10184=ORIENTED_EDGE('',*,*,#6919,.F.);
#10185=ORIENTED_EDGE('',*,*,#6012,.F.);
#10186=ORIENTED_EDGE('',*,*,#5341,.T.);
#10187=ORIENTED_EDGE('',*,*,#6017,.F.);
#10188=ORIENTED_EDGE('',*,*,#6920,.F.);
#10189=ORIENTED_EDGE('',*,*,#6022,.F.);
#10190=ORIENTED_EDGE('',*,*,#6919,.T.);
#10191=ORIENTED_EDGE('',*,*,#6007,.F.);
#10192=ORIENTED_EDGE('',*,*,#5335,.F.);
#10193=ORIENTED_EDGE('',*,*,#6013,.F.);
#10194=ORIENTED_EDGE('',*,*,#6920,.T.);
#10195=ORIENTED_EDGE('',*,*,#6016,.F.);
#10196=ORIENTED_EDGE('',*,*,#6921,.F.);
#10197=ORIENTED_EDGE('',*,*,#6011,.F.);
#10198=ORIENTED_EDGE('',*,*,#6921,.T.);
#10199=ORIENTED_EDGE('',*,*,#6015,.F.);
#10200=ORIENTED_EDGE('',*,*,#6922,.F.);
#10201=ORIENTED_EDGE('',*,*,#6018,.F.);
#10202=ORIENTED_EDGE('',*,*,#5337,.T.);
#10203=ORIENTED_EDGE('',*,*,#6004,.F.);
#10204=ORIENTED_EDGE('',*,*,#6922,.T.);
#10205=ORIENTED_EDGE('',*,*,#6014,.F.);
#10206=ORIENTED_EDGE('',*,*,#5750,.F.);
#10207=ORIENTED_EDGE('',*,*,#6923,.T.);
#10208=ORIENTED_EDGE('',*,*,#5803,.T.);
#10209=ORIENTED_EDGE('',*,*,#6924,.F.);
#10210=ORIENTED_EDGE('',*,*,#5780,.T.);
#10211=ORIENTED_EDGE('',*,*,#6925,.T.);
#10212=ORIENTED_EDGE('',*,*,#5748,.F.);
#10213=ORIENTED_EDGE('',*,*,#6926,.T.);
#10214=ORIENTED_EDGE('',*,*,#6927,.F.);
#10215=ORIENTED_EDGE('',*,*,#5915,.F.);
#10216=ORIENTED_EDGE('',*,*,#6928,.T.);
#10217=ORIENTED_EDGE('',*,*,#5751,.T.);
#10218=ORIENTED_EDGE('',*,*,#6924,.T.);
#10219=ORIENTED_EDGE('',*,*,#5802,.F.);
#10220=ORIENTED_EDGE('',*,*,#5622,.F.);
#10221=ORIENTED_EDGE('',*,*,#6929,.F.);
#10222=ORIENTED_EDGE('',*,*,#6930,.F.);
#10223=ORIENTED_EDGE('',*,*,#5690,.T.);
#10224=ORIENTED_EDGE('',*,*,#5749,.F.);
#10225=ORIENTED_EDGE('',*,*,#6925,.F.);
#10226=ORIENTED_EDGE('',*,*,#5804,.F.);
#10227=ORIENTED_EDGE('',*,*,#6923,.F.);
#10228=ORIENTED_EDGE('',*,*,#5310,.T.);
#10229=ORIENTED_EDGE('',*,*,#5318,.F.);
#10230=ORIENTED_EDGE('',*,*,#5313,.T.);
#10231=ORIENTED_EDGE('',*,*,#5312,.F.);
#10232=ORIENTED_EDGE('',*,*,#5309,.F.);
#10233=ORIENTED_EDGE('',*,*,#5316,.T.);
#10234=ORIENTED_EDGE('',*,*,#5902,.F.);
#10235=ORIENTED_EDGE('',*,*,#6931,.F.);
#10236=ORIENTED_EDGE('',*,*,#6932,.F.);
#10237=ORIENTED_EDGE('',*,*,#5624,.T.);
#10238=ORIENTED_EDGE('',*,*,#5801,.T.);
#10239=ORIENTED_EDGE('',*,*,#6563,.T.);
#10240=ORIENTED_EDGE('',*,*,#6159,.F.);
#10241=ORIENTED_EDGE('',*,*,#6517,.T.);
#10242=ORIENTED_EDGE('',*,*,#5742,.T.);
#10243=ORIENTED_EDGE('',*,*,#5739,.F.);
#10244=ORIENTED_EDGE('',*,*,#5745,.T.);
#10245=ORIENTED_EDGE('',*,*,#5781,.T.);
#10246=ORIENTED_EDGE('',*,*,#6926,.F.);
#10247=ORIENTED_EDGE('',*,*,#5752,.T.);
#10248=ORIENTED_EDGE('',*,*,#6928,.F.);
#10249=ORIENTED_EDGE('',*,*,#5914,.F.);
#10250=ORIENTED_EDGE('',*,*,#5900,.T.);
#10251=ORIENTED_EDGE('',*,*,#6933,.F.);
#10252=ORIENTED_EDGE('',*,*,#5693,.T.);
#10253=ORIENTED_EDGE('',*,*,#6934,.T.);
#10254=ORIENTED_EDGE('',*,*,#5901,.T.);
#10255=ORIENTED_EDGE('',*,*,#6934,.F.);
#10256=ORIENTED_EDGE('',*,*,#5692,.T.);
#10257=ORIENTED_EDGE('',*,*,#6935,.T.);
#10258=ORIENTED_EDGE('',*,*,#6936,.F.);
#10259=ORIENTED_EDGE('',*,*,#6931,.T.);
#10260=ORIENTED_EDGE('',*,*,#6937,.F.);
#10261=ORIENTED_EDGE('',*,*,#6929,.T.);
#10262=ORIENTED_EDGE('',*,*,#5621,.T.);
#10263=ORIENTED_EDGE('',*,*,#6932,.T.);
#10264=ORIENTED_EDGE('',*,*,#6936,.T.);
#10265=ORIENTED_EDGE('',*,*,#5704,.T.);
#10266=ORIENTED_EDGE('',*,*,#5728,.F.);
#10267=ORIENTED_EDGE('',*,*,#5681,.T.);
#10268=ORIENTED_EDGE('',*,*,#5731,.F.);
#10269=ORIENTED_EDGE('',*,*,#5919,.F.);
#10270=ORIENTED_EDGE('',*,*,#6938,.F.);
#10271=ORIENTED_EDGE('',*,*,#5705,.T.);
#10272=ORIENTED_EDGE('',*,*,#6938,.T.);
#10273=ORIENTED_EDGE('',*,*,#5918,.F.);
#10274=ORIENTED_EDGE('',*,*,#6939,.F.);
#10275=ORIENTED_EDGE('',*,*,#6927,.T.);
#10276=ORIENTED_EDGE('',*,*,#5689,.F.);
#10277=ORIENTED_EDGE('',*,*,#6940,.T.);
#10278=ORIENTED_EDGE('',*,*,#5916,.T.);
#10279=ORIENTED_EDGE('',*,*,#6933,.T.);
#10280=ORIENTED_EDGE('',*,*,#5899,.T.);
#10281=ORIENTED_EDGE('',*,*,#6880,.T.);
#10282=ORIENTED_EDGE('',*,*,#6077,.F.);
#10283=ORIENTED_EDGE('',*,*,#6751,.T.);
#10284=ORIENTED_EDGE('',*,*,#5694,.F.);
#10285=ORIENTED_EDGE('',*,*,#5706,.T.);
#10286=ORIENTED_EDGE('',*,*,#6939,.T.);
#10287=ORIENTED_EDGE('',*,*,#5917,.F.);
#10288=ORIENTED_EDGE('',*,*,#6940,.F.);
#10289=ORIENTED_EDGE('',*,*,#5707,.T.);
#10290=ORIENTED_EDGE('',*,*,#6941,.F.);
#10291=ORIENTED_EDGE('',*,*,#5626,.T.);
#10292=ORIENTED_EDGE('',*,*,#5733,.F.);
#10293=ORIENTED_EDGE('',*,*,#5685,.T.);
#10294=ORIENTED_EDGE('',*,*,#5726,.F.);
#10295=ORIENTED_EDGE('',*,*,#5721,.T.);
#10296=ORIENTED_EDGE('',*,*,#6942,.F.);
#10297=ORIENTED_EDGE('',*,*,#5627,.T.);
#10298=ORIENTED_EDGE('',*,*,#6941,.T.);
#10299=ORIENTED_EDGE('',*,*,#5720,.T.);
#10300=ORIENTED_EDGE('',*,*,#6943,.F.);
#10301=ORIENTED_EDGE('',*,*,#6259,.F.);
#10302=ORIENTED_EDGE('',*,*,#5736,.T.);
#10303=ORIENTED_EDGE('',*,*,#5722,.T.);
#10304=ORIENTED_EDGE('',*,*,#5735,.F.);
#10305=ORIENTED_EDGE('',*,*,#6942,.T.);
#10306=ORIENTED_EDGE('',*,*,#6712,.T.);
#10307=ORIENTED_EDGE('',*,*,#6087,.F.);
#10308=ORIENTED_EDGE('',*,*,#6888,.T.);
#10309=ORIENTED_EDGE('',*,*,#5637,.F.);
#10310=ORIENTED_EDGE('',*,*,#6944,.T.);
#10311=ORIENTED_EDGE('',*,*,#5716,.F.);
#10312=ORIENTED_EDGE('',*,*,#5717,.T.);
#10313=ORIENTED_EDGE('',*,*,#6944,.F.);
#10314=ORIENTED_EDGE('',*,*,#5636,.T.);
#10315=ORIENTED_EDGE('',*,*,#6945,.T.);
#10316=ORIENTED_EDGE('',*,*,#6945,.F.);
#10317=ORIENTED_EDGE('',*,*,#6895,.T.);
#10318=ORIENTED_EDGE('',*,*,#6245,.F.);
#10319=ORIENTED_EDGE('',*,*,#6902,.F.);
#10320=ORIENTED_EDGE('',*,*,#6251,.T.);
#10321=ORIENTED_EDGE('',*,*,#6946,.T.);
#10322=ORIENTED_EDGE('',*,*,#5718,.F.);
#10323=ORIENTED_EDGE('',*,*,#6946,.F.);
#10324=ORIENTED_EDGE('',*,*,#6260,.T.);
#10325=ORIENTED_EDGE('',*,*,#6943,.T.);
#10326=ORIENTED_EDGE('',*,*,#5719,.F.);
#10327=ORIENTED_EDGE('',*,*,#5691,.T.);
#10328=ORIENTED_EDGE('',*,*,#6930,.T.);
#10329=ORIENTED_EDGE('',*,*,#6937,.T.);
#10330=ORIENTED_EDGE('',*,*,#6935,.F.);
#10331=ORIENTED_EDGE('',*,*,#6947,.T.);
#10332=ORIENTED_EDGE('',*,*,#6948,.T.);
#10333=ORIENTED_EDGE('',*,*,#6949,.T.);
#10334=ORIENTED_EDGE('',*,*,#6950,.T.);
#10335=ORIENTED_EDGE('',*,*,#6951,.T.);
#10336=ORIENTED_EDGE('',*,*,#6952,.T.);
#10337=ORIENTED_EDGE('',*,*,#6953,.T.);
#10338=ORIENTED_EDGE('',*,*,#6954,.T.);
#10339=ORIENTED_EDGE('',*,*,#6955,.T.);
#10340=ORIENTED_EDGE('',*,*,#6956,.T.);
#10341=ORIENTED_EDGE('',*,*,#6957,.T.);
#10342=ORIENTED_EDGE('',*,*,#6958,.T.);
#10343=ORIENTED_EDGE('',*,*,#6959,.T.);
#10344=ORIENTED_EDGE('',*,*,#6960,.T.);
#10345=ORIENTED_EDGE('',*,*,#6961,.T.);
#10346=ORIENTED_EDGE('',*,*,#6962,.T.);
#10347=ORIENTED_EDGE('',*,*,#6963,.T.);
#10348=ORIENTED_EDGE('',*,*,#6964,.T.);
#10349=ORIENTED_EDGE('',*,*,#6965,.T.);
#10350=ORIENTED_EDGE('',*,*,#6966,.T.);
#10351=ORIENTED_EDGE('',*,*,#6967,.T.);
#10352=ORIENTED_EDGE('',*,*,#6968,.T.);
#10353=ORIENTED_EDGE('',*,*,#6969,.T.);
#10354=ORIENTED_EDGE('',*,*,#6970,.F.);
#10355=ORIENTED_EDGE('',*,*,#6971,.T.);
#10356=ORIENTED_EDGE('',*,*,#6972,.T.);
#10357=ORIENTED_EDGE('',*,*,#6948,.F.);
#10358=ORIENTED_EDGE('',*,*,#6973,.F.);
#10359=ORIENTED_EDGE('',*,*,#6974,.T.);
#10360=ORIENTED_EDGE('',*,*,#6975,.F.);
#10361=ORIENTED_EDGE('',*,*,#6974,.F.);
#10362=ORIENTED_EDGE('',*,*,#6976,.T.);
#10363=ORIENTED_EDGE('',*,*,#6977,.T.);
#10364=ORIENTED_EDGE('',*,*,#6978,.T.);
#10365=ORIENTED_EDGE('',*,*,#6977,.F.);
#10366=ORIENTED_EDGE('',*,*,#6979,.F.);
#10367=ORIENTED_EDGE('',*,*,#6980,.T.);
#10368=ORIENTED_EDGE('',*,*,#6981,.F.);
#10369=ORIENTED_EDGE('',*,*,#6980,.F.);
#10370=ORIENTED_EDGE('',*,*,#6981,.T.);
#10371=ORIENTED_EDGE('',*,*,#6982,.T.);
#10372=ORIENTED_EDGE('',*,*,#6983,.T.);
#10373=ORIENTED_EDGE('',*,*,#6982,.F.);
#10374=ORIENTED_EDGE('',*,*,#6984,.F.);
#10375=ORIENTED_EDGE('',*,*,#6985,.F.);
#10376=ORIENTED_EDGE('',*,*,#6986,.F.);
#10377=ORIENTED_EDGE('',*,*,#6987,.F.);
#10378=ORIENTED_EDGE('',*,*,#6988,.T.);
#10379=ORIENTED_EDGE('',*,*,#6956,.F.);
#10380=ORIENTED_EDGE('',*,*,#6989,.F.);
#10381=ORIENTED_EDGE('',*,*,#6990,.F.);
#10382=ORIENTED_EDGE('',*,*,#6991,.F.);
#10383=ORIENTED_EDGE('',*,*,#6953,.F.);
#10384=ORIENTED_EDGE('',*,*,#6992,.F.);
#10385=ORIENTED_EDGE('',*,*,#6993,.F.);
#10386=ORIENTED_EDGE('',*,*,#6994,.F.);
#10387=ORIENTED_EDGE('',*,*,#6950,.F.);
#10388=ORIENTED_EDGE('',*,*,#6995,.F.);
#10389=ORIENTED_EDGE('',*,*,#6996,.F.);
#10390=ORIENTED_EDGE('',*,*,#6997,.F.);
#10391=ORIENTED_EDGE('',*,*,#6998,.F.);
#10392=ORIENTED_EDGE('',*,*,#6969,.F.);
#10393=ORIENTED_EDGE('',*,*,#6999,.F.);
#10394=ORIENTED_EDGE('',*,*,#7000,.F.);
#10395=ORIENTED_EDGE('',*,*,#7001,.F.);
#10396=ORIENTED_EDGE('',*,*,#6966,.F.);
#10397=ORIENTED_EDGE('',*,*,#7002,.F.);
#10398=ORIENTED_EDGE('',*,*,#7003,.F.);
#10399=ORIENTED_EDGE('',*,*,#7004,.F.);
#10400=ORIENTED_EDGE('',*,*,#6963,.F.);
#10401=ORIENTED_EDGE('',*,*,#7005,.F.);
#10402=ORIENTED_EDGE('',*,*,#7006,.F.);
#10403=ORIENTED_EDGE('',*,*,#7007,.F.);
#10404=ORIENTED_EDGE('',*,*,#6960,.F.);
#10405=ORIENTED_EDGE('',*,*,#7008,.F.);
#10406=ORIENTED_EDGE('',*,*,#7009,.F.);
#10407=ORIENTED_EDGE('',*,*,#7010,.F.);
#10408=ORIENTED_EDGE('',*,*,#6957,.F.);
#10409=ORIENTED_EDGE('',*,*,#6988,.F.);
#10410=ORIENTED_EDGE('',*,*,#6970,.T.);
#10411=ORIENTED_EDGE('',*,*,#6998,.T.);
#10412=ORIENTED_EDGE('',*,*,#7011,.T.);
#10413=ORIENTED_EDGE('',*,*,#7012,.T.);
#10414=ORIENTED_EDGE('',*,*,#7013,.T.);
#10415=ORIENTED_EDGE('',*,*,#7014,.T.);
#10416=ORIENTED_EDGE('',*,*,#7000,.T.);
#10417=ORIENTED_EDGE('',*,*,#7015,.F.);
#10418=ORIENTED_EDGE('',*,*,#7016,.T.);
#10419=ORIENTED_EDGE('',*,*,#7012,.F.);
#10420=ORIENTED_EDGE('',*,*,#6999,.T.);
#10421=ORIENTED_EDGE('',*,*,#6968,.F.);
#10422=ORIENTED_EDGE('',*,*,#7014,.F.);
#10423=ORIENTED_EDGE('',*,*,#7017,.T.);
#10424=ORIENTED_EDGE('',*,*,#7015,.T.);
#10425=ORIENTED_EDGE('',*,*,#6967,.F.);
#10426=ORIENTED_EDGE('',*,*,#7001,.T.);
#10427=ORIENTED_EDGE('',*,*,#7018,.F.);
#10428=ORIENTED_EDGE('',*,*,#7019,.T.);
#10429=ORIENTED_EDGE('',*,*,#7020,.T.);
#10430=ORIENTED_EDGE('',*,*,#6971,.F.);
#10431=ORIENTED_EDGE('',*,*,#7011,.F.);
#10432=ORIENTED_EDGE('',*,*,#6997,.T.);
#10433=ORIENTED_EDGE('',*,*,#7020,.F.);
#10434=ORIENTED_EDGE('',*,*,#7021,.T.);
#10435=ORIENTED_EDGE('',*,*,#7022,.F.);
#10436=ORIENTED_EDGE('',*,*,#6995,.T.);
#10437=ORIENTED_EDGE('',*,*,#6949,.F.);
#10438=ORIENTED_EDGE('',*,*,#6972,.F.);
#10439=ORIENTED_EDGE('',*,*,#7022,.T.);
#10440=ORIENTED_EDGE('',*,*,#7023,.T.);
#10441=ORIENTED_EDGE('',*,*,#7018,.T.);
#10442=ORIENTED_EDGE('',*,*,#6996,.T.);
#10443=ORIENTED_EDGE('',*,*,#7024,.F.);
#10444=ORIENTED_EDGE('',*,*,#7025,.T.);
#10445=ORIENTED_EDGE('',*,*,#7026,.T.);
#10446=ORIENTED_EDGE('',*,*,#6951,.F.);
#10447=ORIENTED_EDGE('',*,*,#6994,.T.);
#10448=ORIENTED_EDGE('',*,*,#7026,.F.);
#10449=ORIENTED_EDGE('',*,*,#7027,.T.);
#10450=ORIENTED_EDGE('',*,*,#7028,.F.);
#10451=ORIENTED_EDGE('',*,*,#6992,.T.);
#10452=ORIENTED_EDGE('',*,*,#6952,.F.);
#10453=ORIENTED_EDGE('',*,*,#7028,.T.);
#10454=ORIENTED_EDGE('',*,*,#7029,.T.);
#10455=ORIENTED_EDGE('',*,*,#7024,.T.);
#10456=ORIENTED_EDGE('',*,*,#6993,.T.);
#10457=ORIENTED_EDGE('',*,*,#7030,.F.);
#10458=ORIENTED_EDGE('',*,*,#7031,.T.);
#10459=ORIENTED_EDGE('',*,*,#7032,.T.);
#10460=ORIENTED_EDGE('',*,*,#6954,.F.);
#10461=ORIENTED_EDGE('',*,*,#6991,.T.);
#10462=ORIENTED_EDGE('',*,*,#7032,.F.);
#10463=ORIENTED_EDGE('',*,*,#7033,.T.);
#10464=ORIENTED_EDGE('',*,*,#7034,.F.);
#10465=ORIENTED_EDGE('',*,*,#6989,.T.);
#10466=ORIENTED_EDGE('',*,*,#6955,.F.);
#10467=ORIENTED_EDGE('',*,*,#7034,.T.);
#10468=ORIENTED_EDGE('',*,*,#7035,.T.);
#10469=ORIENTED_EDGE('',*,*,#7030,.T.);
#10470=ORIENTED_EDGE('',*,*,#6990,.T.);
#10471=ORIENTED_EDGE('',*,*,#7036,.F.);
#10472=ORIENTED_EDGE('',*,*,#6984,.T.);
#10473=ORIENTED_EDGE('',*,*,#7037,.T.);
#10474=ORIENTED_EDGE('',*,*,#6958,.F.);
#10475=ORIENTED_EDGE('',*,*,#7010,.T.);
#10476=ORIENTED_EDGE('',*,*,#7037,.F.);
#10477=ORIENTED_EDGE('',*,*,#6986,.T.);
#10478=ORIENTED_EDGE('',*,*,#7038,.F.);
#10479=ORIENTED_EDGE('',*,*,#7008,.T.);
#10480=ORIENTED_EDGE('',*,*,#6959,.F.);
#10481=ORIENTED_EDGE('',*,*,#7038,.T.);
#10482=ORIENTED_EDGE('',*,*,#6985,.T.);
#10483=ORIENTED_EDGE('',*,*,#7036,.T.);
#10484=ORIENTED_EDGE('',*,*,#7009,.T.);
#10485=ORIENTED_EDGE('',*,*,#7039,.F.);
#10486=ORIENTED_EDGE('',*,*,#7040,.T.);
#10487=ORIENTED_EDGE('',*,*,#7041,.T.);
#10488=ORIENTED_EDGE('',*,*,#6961,.F.);
#10489=ORIENTED_EDGE('',*,*,#7007,.T.);
#10490=ORIENTED_EDGE('',*,*,#7041,.F.);
#10491=ORIENTED_EDGE('',*,*,#7042,.T.);
#10492=ORIENTED_EDGE('',*,*,#7043,.F.);
#10493=ORIENTED_EDGE('',*,*,#7005,.T.);
#10494=ORIENTED_EDGE('',*,*,#6962,.F.);
#10495=ORIENTED_EDGE('',*,*,#7043,.T.);
#10496=ORIENTED_EDGE('',*,*,#7044,.T.);
#10497=ORIENTED_EDGE('',*,*,#7039,.T.);
#10498=ORIENTED_EDGE('',*,*,#7006,.T.);
#10499=ORIENTED_EDGE('',*,*,#7045,.F.);
#10500=ORIENTED_EDGE('',*,*,#7046,.T.);
#10501=ORIENTED_EDGE('',*,*,#7047,.T.);
#10502=ORIENTED_EDGE('',*,*,#6964,.F.);
#10503=ORIENTED_EDGE('',*,*,#7004,.T.);
#10504=ORIENTED_EDGE('',*,*,#7047,.F.);
#10505=ORIENTED_EDGE('',*,*,#7048,.T.);
#10506=ORIENTED_EDGE('',*,*,#7049,.F.);
#10507=ORIENTED_EDGE('',*,*,#7002,.T.);
#10508=ORIENTED_EDGE('',*,*,#6965,.F.);
#10509=ORIENTED_EDGE('',*,*,#7049,.T.);
#10510=ORIENTED_EDGE('',*,*,#7050,.T.);
#10511=ORIENTED_EDGE('',*,*,#7045,.T.);
#10512=ORIENTED_EDGE('',*,*,#7003,.T.);
#10513=ORIENTED_EDGE('',*,*,#6987,.T.);
#10514=ORIENTED_EDGE('',*,*,#6947,.F.);
#10515=ORIENTED_EDGE('',*,*,#6983,.F.);
#10516=ORIENTED_EDGE('',*,*,#7050,.F.);
#10517=ORIENTED_EDGE('',*,*,#7048,.F.);
#10518=ORIENTED_EDGE('',*,*,#7046,.F.);
#10519=ORIENTED_EDGE('',*,*,#7044,.F.);
#10520=ORIENTED_EDGE('',*,*,#7042,.F.);
#10521=ORIENTED_EDGE('',*,*,#7040,.F.);
#10522=ORIENTED_EDGE('',*,*,#7035,.F.);
#10523=ORIENTED_EDGE('',*,*,#7033,.F.);
#10524=ORIENTED_EDGE('',*,*,#7031,.F.);
#10525=ORIENTED_EDGE('',*,*,#7029,.F.);
#10526=ORIENTED_EDGE('',*,*,#7027,.F.);
#10527=ORIENTED_EDGE('',*,*,#7025,.F.);
#10528=ORIENTED_EDGE('',*,*,#7023,.F.);
#10529=ORIENTED_EDGE('',*,*,#7021,.F.);
#10530=ORIENTED_EDGE('',*,*,#7019,.F.);
#10531=ORIENTED_EDGE('',*,*,#7016,.F.);
#10532=ORIENTED_EDGE('',*,*,#7017,.F.);
#10533=ORIENTED_EDGE('',*,*,#7013,.F.);
#10534=ORIENTED_EDGE('',*,*,#6979,.T.);
#10535=ORIENTED_EDGE('',*,*,#6975,.T.);
#10536=ORIENTED_EDGE('',*,*,#6973,.T.);
#10537=ORIENTED_EDGE('',*,*,#6976,.F.);
#10538=ORIENTED_EDGE('',*,*,#6978,.F.);
#10539=CYLINDRICAL_SURFACE('',#11524,2.1875);
#10540=CYLINDRICAL_SURFACE('',#11527,2.5625);
#10541=CYLINDRICAL_SURFACE('',#11530,3.4375);
#10542=CYLINDRICAL_SURFACE('',#11533,1.3125);
#10543=CYLINDRICAL_SURFACE('',#11692,0.3125);
#10544=CYLINDRICAL_SURFACE('',#11695,0.3125);
#10545=CYLINDRICAL_SURFACE('',#11698,0.3125);
#10546=CYLINDRICAL_SURFACE('',#11705,0.3125);
#10547=CYLINDRICAL_SURFACE('',#11708,0.3125);
#10548=CYLINDRICAL_SURFACE('',#11711,0.3125);
#10549=CYLINDRICAL_SURFACE('',#11714,0.3125);
#10550=CYLINDRICAL_SURFACE('',#11732,0.937500000000001);
#10551=CYLINDRICAL_SURFACE('',#11735,4.375);
#10552=CYLINDRICAL_SURFACE('',#11738,2.8125);
#10553=CYLINDRICAL_SURFACE('',#11739,2.8125);
#10554=CYLINDRICAL_SURFACE('',#11740,0.937500000000001);
#10555=CYLINDRICAL_SURFACE('',#11742,0.937500000000001);
#10556=CYLINDRICAL_SURFACE('',#11745,4.375);
#10557=CYLINDRICAL_SURFACE('',#11748,2.8125);
#10558=CYLINDRICAL_SURFACE('',#11749,2.8125);
#10559=CYLINDRICAL_SURFACE('',#11753,0.937500000000001);
#10560=CYLINDRICAL_SURFACE('',#11755,0.937500000000001);
#10561=CYLINDRICAL_SURFACE('',#11758,4.375);
#10562=CYLINDRICAL_SURFACE('',#11759,2.8125);
#10563=CYLINDRICAL_SURFACE('',#11760,2.8125);
#10564=CYLINDRICAL_SURFACE('',#11765,0.937500000000001);
#10565=CYLINDRICAL_SURFACE('',#11767,0.937500000000001);
#10566=CYLINDRICAL_SURFACE('',#11768,4.375);
#10567=CYLINDRICAL_SURFACE('',#11769,48.4375);
#10568=CYLINDRICAL_SURFACE('',#11810,2.8125);
#10569=CYLINDRICAL_SURFACE('',#11811,2.8125);
#10570=CYLINDRICAL_SURFACE('',#11816,0.937500000000001);
#10571=CYLINDRICAL_SURFACE('',#11818,1.25);
#10572=CYLINDRICAL_SURFACE('',#11860,0.3125);
#10573=CYLINDRICAL_SURFACE('',#11863,0.3125);
#10574=CYLINDRICAL_SURFACE('',#11866,0.3125);
#10575=CYLINDRICAL_SURFACE('',#11869,0.3125);
#10576=CYLINDRICAL_SURFACE('',#11872,0.3125);
#10577=CYLINDRICAL_SURFACE('',#11874,0.3125);
#10578=CYLINDRICAL_SURFACE('',#11877,0.3125);
#10579=CYLINDRICAL_SURFACE('',#11880,0.312499999999999);
#10580=CYLINDRICAL_SURFACE('',#11931,49.6875);
#10581=CYLINDRICAL_SURFACE('',#11934,49.6875);
#10582=CYLINDRICAL_SURFACE('',#11956,5.625);
#10583=CYLINDRICAL_SURFACE('',#11981,5.625);
#10584=CYLINDRICAL_SURFACE('',#11995,21.875);
#10585=CYLINDRICAL_SURFACE('',#12006,55.);
#10586=CYLINDRICAL_SURFACE('',#12016,0.937500000000001);
#10587=CYLINDRICAL_SURFACE('',#12019,0.937500000000001);
#10588=CYLINDRICAL_SURFACE('',#12022,0.937500000000001);
#10589=CYLINDRICAL_SURFACE('',#12040,49.6875);
#10590=CYLINDRICAL_SURFACE('',#12057,5.625);
#10591=CYLINDRICAL_SURFACE('',#12061,5.625);
#10592=CYLINDRICAL_SURFACE('',#12072,21.875);
#10593=CYLINDRICAL_SURFACE('',#12083,55.);
#10594=CYLINDRICAL_SURFACE('',#12093,0.937500000000001);
#10595=CYLINDRICAL_SURFACE('',#12094,0.937500000000001);
#10596=CYLINDRICAL_SURFACE('',#12097,0.937500000000001);
#10597=CYLINDRICAL_SURFACE('',#12115,49.6875);
#10598=CYLINDRICAL_SURFACE('',#12120,5.625);
#10599=CYLINDRICAL_SURFACE('',#12124,5.625);
#10600=CYLINDRICAL_SURFACE('',#12135,21.875);
#10601=CYLINDRICAL_SURFACE('',#12146,55.);
#10602=CYLINDRICAL_SURFACE('',#12157,0.937500000000001);
#10603=CYLINDRICAL_SURFACE('',#12160,0.937500000000001);
#10604=CYLINDRICAL_SURFACE('',#12161,0.937500000000001);
#10605=CYLINDRICAL_SURFACE('',#12188,5.625);
#10606=CYLINDRICAL_SURFACE('',#12191,5.625);
#10607=CYLINDRICAL_SURFACE('',#12199,21.875);
#10608=CYLINDRICAL_SURFACE('',#12210,55.);
#10609=CYLINDRICAL_SURFACE('',#12221,0.937500000000001);
#10610=CYLINDRICAL_SURFACE('',#12224,0.937500000000001);
#10611=CYLINDRICAL_SURFACE('',#12227,0.937500000000001);
#10612=CYLINDRICAL_SURFACE('',#12232,0.3125);
#10613=CYLINDRICAL_SURFACE('',#12234,0.3125);
#10614=CYLINDRICAL_SURFACE('',#12245,0.3125);
#10615=CYLINDRICAL_SURFACE('',#12247,0.3125);
#10616=CYLINDRICAL_SURFACE('',#12262,0.312500000000001);
#10617=CYLINDRICAL_SURFACE('',#12264,0.3125);
#10618=CYLINDRICAL_SURFACE('',#12267,0.3125);
#10619=CYLINDRICAL_SURFACE('',#12281,0.312500000000001);
#10620=CYLINDRICAL_SURFACE('',#12284,0.3125);
#10621=CYLINDRICAL_SURFACE('',#12287,0.312499999999999);
#10622=CYLINDRICAL_SURFACE('',#12297,0.312500000000002);
#10623=CYLINDRICAL_SURFACE('',#12309,0.3125);
#10624=CYLINDRICAL_SURFACE('',#12315,0.312500000000001);
#10625=CYLINDRICAL_SURFACE('',#12316,0.3125);
#10626=CYLINDRICAL_SURFACE('',#12319,0.312499999999999);
#10627=CYLINDRICAL_SURFACE('',#12325,0.3125);
#10628=CYLINDRICAL_SURFACE('',#12327,0.312499999999999);
#10629=CYLINDRICAL_SURFACE('',#12344,0.3125);
#10630=CYLINDRICAL_SURFACE('',#12346,0.312500000000001);
#10631=CYLINDRICAL_SURFACE('',#12350,0.3125);
#10632=CYLINDRICAL_SURFACE('',#12359,0.3125);
#10633=CYLINDRICAL_SURFACE('',#12361,0.3125);
#10634=CYLINDRICAL_SURFACE('',#12364,0.312499999999999);
#10635=CYLINDRICAL_SURFACE('',#12370,0.3125);
#10636=CYLINDRICAL_SURFACE('',#12375,0.3125);
#10637=CYLINDRICAL_SURFACE('',#12378,0.3125);
#10638=CYLINDRICAL_SURFACE('',#12390,0.312499999999999);
#10639=CYLINDRICAL_SURFACE('',#12401,0.3125);
#10640=CYLINDRICAL_SURFACE('',#12404,0.3125);
#10641=CYLINDRICAL_SURFACE('',#12406,0.312499999999999);
#10642=CYLINDRICAL_SURFACE('',#12409,0.3125);
#10643=CYLINDRICAL_SURFACE('',#12411,0.3125);
#10644=CYLINDRICAL_SURFACE('',#12419,0.312500000000001);
#10645=CYLINDRICAL_SURFACE('',#12429,0.3125);
#10646=CYLINDRICAL_SURFACE('',#12433,0.312499999999999);
#10647=CYLINDRICAL_SURFACE('',#12435,0.3125);
#10648=CYLINDRICAL_SURFACE('',#12437,0.3125);
#10649=CYLINDRICAL_SURFACE('',#12449,0.3125);
#10650=CYLINDRICAL_SURFACE('',#12451,0.3125);
#10651=CYLINDRICAL_SURFACE('',#12455,0.3125);
#10652=CYLINDRICAL_SURFACE('',#12458,0.312499999999999);
#10653=CYLINDRICAL_SURFACE('',#12462,0.3125);
#10654=CYLINDRICAL_SURFACE('',#12471,0.312499999999999);
#10655=CYLINDRICAL_SURFACE('',#12478,0.312499999999999);
#10656=CYLINDRICAL_SURFACE('',#12483,0.3125);
#10657=CYLINDRICAL_SURFACE('',#12485,0.3125);
#10658=CYLINDRICAL_SURFACE('',#12491,0.3125);
#10659=CYLINDRICAL_SURFACE('',#12494,0.3125);
#10660=CYLINDRICAL_SURFACE('',#12500,0.3125);
#10661=CYLINDRICAL_SURFACE('',#12503,0.3125);
#10662=CYLINDRICAL_SURFACE('',#12511,0.3125);
#10663=CYLINDRICAL_SURFACE('',#12513,0.3125);
#10664=CYLINDRICAL_SURFACE('',#12519,0.3125);
#10665=CYLINDRICAL_SURFACE('',#12527,0.3125);
#10666=CYLINDRICAL_SURFACE('',#12531,0.3125);
#10667=CYLINDRICAL_SURFACE('',#12536,0.312499169784042);
#10668=CYLINDRICAL_SURFACE('',#12547,0.312499999999999);
#10669=CYLINDRICAL_SURFACE('',#12561,0.312499805812968);
#10670=CYLINDRICAL_SURFACE('',#12566,0.3125);
#10671=CYLINDRICAL_SURFACE('',#12568,0.312500000000001);
#10672=CYLINDRICAL_SURFACE('',#12583,0.312500000000001);
#10673=CYLINDRICAL_SURFACE('',#12586,0.312500000000001);
#10674=CYLINDRICAL_SURFACE('',#12588,0.3125);
#10675=CYLINDRICAL_SURFACE('',#12590,0.3125);
#10676=CYLINDRICAL_SURFACE('',#12593,0.312499805814757);
#10677=CYLINDRICAL_SURFACE('',#12608,0.312500000000001);
#10678=CYLINDRICAL_SURFACE('',#12610,0.3125);
#10679=CYLINDRICAL_SURFACE('',#12614,0.312500000000001);
#10680=CYLINDRICAL_SURFACE('',#12615,0.312500000000001);
#10681=CYLINDRICAL_SURFACE('',#12619,0.3125);
#10682=CYLINDRICAL_SURFACE('',#12624,0.3125);
#10683=CYLINDRICAL_SURFACE('',#12643,0.3125);
#10684=CYLINDRICAL_SURFACE('',#12645,0.3125);
#10685=CYLINDRICAL_SURFACE('',#12647,0.312500000000001);
#10686=CYLINDRICAL_SURFACE('',#12649,0.31249916978701);
#10687=CYLINDRICAL_SURFACE('',#12652,0.3125);
#10688=CYLINDRICAL_SURFACE('',#12656,0.312499169785485);
#10689=CYLINDRICAL_SURFACE('',#12658,0.3125);
#10690=CYLINDRICAL_SURFACE('',#12679,0.3125);
#10691=CYLINDRICAL_SURFACE('',#12683,0.3125);
#10692=CYLINDRICAL_SURFACE('',#12687,0.312499805816233);
#10693=CYLINDRICAL_SURFACE('',#12692,0.3125);
#10694=CYLINDRICAL_SURFACE('',#12694,0.3125);
#10695=CYLINDRICAL_SURFACE('',#12696,0.312500000000001);
#10696=CYLINDRICAL_SURFACE('',#12713,0.3125);
#10697=CYLINDRICAL_SURFACE('',#12718,0.3125);
#10698=CYLINDRICAL_SURFACE('',#12720,0.312499999999999);
#10699=CYLINDRICAL_SURFACE('',#12721,0.3125);
#10700=CYLINDRICAL_SURFACE('',#12726,0.312500000000001);
#10701=CYLINDRICAL_SURFACE('',#12728,0.312500000000001);
#10702=CYLINDRICAL_SURFACE('',#12739,0.3125);
#10703=CYLINDRICAL_SURFACE('',#12741,0.3125);
#10704=CYLINDRICAL_SURFACE('',#12746,0.312499999999999);
#10705=CYLINDRICAL_SURFACE('',#12750,0.312499805811005);
#10706=CYLINDRICAL_SURFACE('',#12752,0.312500000000001);
#10707=CYLINDRICAL_SURFACE('',#12768,0.3125);
#10708=CYLINDRICAL_SURFACE('',#12770,0.312500000000001);
#10709=CYLINDRICAL_SURFACE('',#12772,0.312499169782492);
#10710=CYLINDRICAL_SURFACE('',#12774,0.3125);
#10711=CYLINDRICAL_SURFACE('',#12784,0.312499999999996);
#10712=CYLINDRICAL_SURFACE('',#12786,0.3125);
#10713=CYLINDRICAL_SURFACE('',#12795,0.3125);
#10714=CYLINDRICAL_SURFACE('',#12802,0.3125);
#10715=CYLINDRICAL_SURFACE('',#12813,0.3125);
#10716=CYLINDRICAL_SURFACE('',#12820,0.3125);
#10717=CYLINDRICAL_SURFACE('',#12828,0.3125);
#10718=CYLINDRICAL_SURFACE('',#12830,0.3125);
#10719=CYLINDRICAL_SURFACE('',#12836,0.3125);
#10720=CYLINDRICAL_SURFACE('',#12838,0.3125);
#10721=CYLINDRICAL_SURFACE('',#12844,0.3125);
#10722=CYLINDRICAL_SURFACE('',#12846,0.3125);
#10723=CYLINDRICAL_SURFACE('',#12852,0.3125);
#10724=CYLINDRICAL_SURFACE('',#12854,0.3125);
#10725=CYLINDRICAL_SURFACE('',#12861,0.3125);
#10726=CYLINDRICAL_SURFACE('',#12864,0.3125);
#10727=CYLINDRICAL_SURFACE('',#12875,0.3125);
#10728=CYLINDRICAL_SURFACE('',#12878,0.3125);
#10729=CYLINDRICAL_SURFACE('',#12889,0.3125);
#10730=CYLINDRICAL_SURFACE('',#12891,0.3125);
#10731=CYLINDRICAL_SURFACE('',#12899,0.3125);
#10732=CYLINDRICAL_SURFACE('',#12901,0.3125);
#10733=CYLINDRICAL_SURFACE('',#12909,0.3125);
#10734=CYLINDRICAL_SURFACE('',#12910,0.3125);
#10735=CYLINDRICAL_SURFACE('',#12919,0.3125);
#10736=CYLINDRICAL_SURFACE('',#12920,0.3125);
#10737=CYLINDRICAL_SURFACE('',#12925,20.);
#10738=CYLINDRICAL_SURFACE('',#12928,1.25);
#10739=CYLINDRICAL_SURFACE('',#12951,21.875);
#10740=CYLINDRICAL_SURFACE('',#12965,1.875);
#10741=CYLINDRICAL_SURFACE('',#12972,20.);
#10742=CYLINDRICAL_SURFACE('',#12974,46.875);
#10743=CYLINDRICAL_SURFACE('',#12979,21.875);
#10744=CYLINDRICAL_SURFACE('',#12982,46.875);
#10745=CYLINDRICAL_SURFACE('',#12983,46.875);
#10746=CYLINDRICAL_SURFACE('',#12984,46.875);
#10747=CYLINDRICAL_SURFACE('',#12985,46.875);
#10748=CYLINDRICAL_SURFACE('',#12986,46.875);
#10749=CYLINDRICAL_SURFACE('',#12987,46.875);
#10750=ADVANCED_FACE('',(#1012),#10539,.F.);
#10751=ADVANCED_FACE('',(#1013),#10540,.F.);
#10752=ADVANCED_FACE('',(#1014),#10541,.T.);
#10753=ADVANCED_FACE('',(#1015),#10542,.F.);
#10754=ADVANCED_FACE('',(#1016),#837,.T.);
#10755=ADVANCED_FACE('',(#1017),#838,.T.);
#10756=ADVANCED_FACE('',(#1018),#839,.T.);
#10757=ADVANCED_FACE('',(#1019),#840,.T.);
#10758=ADVANCED_FACE('',(#1020),#841,.F.);
#10759=ADVANCED_FACE('',(#1021),#842,.F.);
#10760=ADVANCED_FACE('',(#1022),#843,.T.);
#10761=ADVANCED_FACE('',(#1023),#844,.T.);
#10762=ADVANCED_FACE('',(#1024),#845,.T.);
#10763=ADVANCED_FACE('',(#1025),#846,.T.);
#10764=ADVANCED_FACE('',(#1026),#847,.T.);
#10765=ADVANCED_FACE('',(#1027),#848,.T.);
#10766=ADVANCED_FACE('',(#1028),#849,.F.);
#10767=ADVANCED_FACE('',(#1029),#850,.F.);
#10768=ADVANCED_FACE('',(#1030),#851,.T.);
#10769=ADVANCED_FACE('',(#1031),#852,.T.);
#10770=ADVANCED_FACE('',(#1032),#853,.T.);
#10771=ADVANCED_FACE('',(#1033),#854,.T.);
#10772=ADVANCED_FACE('',(#1034),#855,.T.);
#10773=ADVANCED_FACE('',(#1035),#856,.T.);
#10774=ADVANCED_FACE('',(#1036),#857,.F.);
#10775=ADVANCED_FACE('',(#1037),#858,.T.);
#10776=ADVANCED_FACE('',(#1038),#859,.T.);
#10777=ADVANCED_FACE('',(#1039),#860,.T.);
#10778=ADVANCED_FACE('',(#1040),#861,.T.);
#10779=ADVANCED_FACE('',(#1041),#862,.T.);
#10780=ADVANCED_FACE('',(#1042),#863,.F.);
#10781=ADVANCED_FACE('',(#1043),#864,.F.);
#10782=ADVANCED_FACE('',(#1044),#865,.F.);
#10783=ADVANCED_FACE('',(#1045),#866,.F.);
#10784=ADVANCED_FACE('',(#1046),#867,.F.);
#10785=ADVANCED_FACE('',(#1047),#868,.F.);
#10786=ADVANCED_FACE('',(#1048),#10543,.F.);
#10787=ADVANCED_FACE('',(#1049),#10544,.F.);
#10788=ADVANCED_FACE('',(#1050),#10545,.F.);
#10789=ADVANCED_FACE('',(#1051),#869,.T.);
#10790=ADVANCED_FACE('',(#1052),#10546,.T.);
#10791=ADVANCED_FACE('',(#1053),#10547,.F.);
#10792=ADVANCED_FACE('',(#1054),#10548,.T.);
#10793=ADVANCED_FACE('',(#1055),#10549,.F.);
#10794=ADVANCED_FACE('',(#1056),#870,.T.);
#10795=ADVANCED_FACE('',(#1057),#871,.F.);
#10796=ADVANCED_FACE('',(#1058),#872,.T.);
#10797=ADVANCED_FACE('',(#1059),#10550,.F.);
#10798=ADVANCED_FACE('',(#1060),#10551,.T.);
#10799=ADVANCED_FACE('',(#1061),#10552,.F.);
#10800=ADVANCED_FACE('',(#1062),#10553,.F.);
#10801=ADVANCED_FACE('',(#1063),#10554,.T.);
#10802=ADVANCED_FACE('',(#1064),#10555,.F.);
#10803=ADVANCED_FACE('',(#1065),#10556,.T.);
#10804=ADVANCED_FACE('',(#1066),#10557,.F.);
#10805=ADVANCED_FACE('',(#1067),#10558,.F.);
#10806=ADVANCED_FACE('',(#1068),#817,.T.);
#10807=ADVANCED_FACE('',(#1069),#10559,.T.);
#10808=ADVANCED_FACE('',(#1070),#10560,.F.);
#10809=ADVANCED_FACE('',(#1071),#10561,.T.);
#10810=ADVANCED_FACE('',(#1072),#10562,.F.);
#10811=ADVANCED_FACE('',(#1073),#10563,.F.);
#10812=ADVANCED_FACE('',(#1074),#818,.T.);
#10813=ADVANCED_FACE('',(#1075),#10564,.T.);
#10814=ADVANCED_FACE('',(#1076),#10565,.F.);
#10815=ADVANCED_FACE('',(#1077),#10566,.T.);
#10816=ADVANCED_FACE('',(#1078),#10567,.F.);
#10817=ADVANCED_FACE('',(#1079),#10568,.F.);
#10818=ADVANCED_FACE('',(#1080),#10569,.F.);
#10819=ADVANCED_FACE('',(#1081),#819,.T.);
#10820=ADVANCED_FACE('',(#1082),#10570,.T.);
#10821=ADVANCED_FACE('',(#1083),#10571,.F.);
#10822=ADVANCED_FACE('',(#1084,#284,#285,#286,#287,#288,#289,#290,#291),
#315,.T.);
#10823=ADVANCED_FACE('',(#1085),#316,.F.);
#10824=ADVANCED_FACE('',(#1086),#317,.F.);
#10825=ADVANCED_FACE('',(#1087,#292),#318,.F.);
#10826=ADVANCED_FACE('',(#1088,#293),#319,.F.);
#10827=ADVANCED_FACE('',(#1089),#320,.F.);
#10828=ADVANCED_FACE('',(#1090),#10572,.T.);
#10829=ADVANCED_FACE('',(#1091),#10573,.T.);
#10830=ADVANCED_FACE('',(#1092),#10574,.T.);
#10831=ADVANCED_FACE('',(#1093),#10575,.T.);
#10832=ADVANCED_FACE('',(#1094),#10576,.T.);
#10833=ADVANCED_FACE('',(#1095),#10577,.F.);
#10834=ADVANCED_FACE('',(#1096),#321,.F.);
#10835=ADVANCED_FACE('',(#1097),#10578,.T.);
#10836=ADVANCED_FACE('',(#1098),#10579,.T.);
#10837=ADVANCED_FACE('',(#1099,#294),#322,.T.);
#10838=ADVANCED_FACE('',(#1100),#323,.T.);
#10839=ADVANCED_FACE('',(#1101),#324,.T.);
#10840=ADVANCED_FACE('',(#1102),#325,.T.);
#10841=ADVANCED_FACE('',(#1103),#326,.T.);
#10842=ADVANCED_FACE('',(#1104),#820,.F.);
#10843=ADVANCED_FACE('',(#1105),#327,.F.);
#10844=ADVANCED_FACE('',(#1106),#328,.F.);
#10845=ADVANCED_FACE('',(#1107),#329,.T.);
#10846=ADVANCED_FACE('',(#1108),#821,.F.);
#10847=ADVANCED_FACE('',(#1109),#822,.T.);
#10848=ADVANCED_FACE('',(#1110),#10580,.T.);
#10849=ADVANCED_FACE('',(#1111),#10581,.T.);
#10850=ADVANCED_FACE('',(#1112),#823,.T.);
#10851=ADVANCED_FACE('',(#1113),#824,.T.);
#10852=ADVANCED_FACE('',(#1114,#295),#330,.F.);
#10853=ADVANCED_FACE('',(#1115,#296),#331,.F.);
#10854=ADVANCED_FACE('',(#1116),#332,.F.);
#10855=ADVANCED_FACE('',(#1117),#333,.F.);
#10856=ADVANCED_FACE('',(#1118),#10582,.T.);
#10857=ADVANCED_FACE('',(#1119),#334,.F.);
#10858=ADVANCED_FACE('',(#1120),#335,.F.);
#10859=ADVANCED_FACE('',(#1121,#297,#298,#299,#300,#301,#302,#303,#304),
#336,.F.);
#10860=ADVANCED_FACE('',(#1122),#10583,.T.);
#10861=ADVANCED_FACE('',(#1123),#825,.F.);
#10862=ADVANCED_FACE('',(#1124),#337,.T.);
#10863=ADVANCED_FACE('',(#1125),#338,.T.);
#10864=ADVANCED_FACE('',(#1126),#339,.F.);
#10865=ADVANCED_FACE('',(#1127),#340,.F.);
#10866=ADVANCED_FACE('',(#1128),#10584,.T.);
#10867=ADVANCED_FACE('',(#1129),#341,.T.);
#10868=ADVANCED_FACE('',(#1130),#342,.T.);
#10869=ADVANCED_FACE('',(#1131),#343,.T.);
#10870=ADVANCED_FACE('',(#1132),#344,.F.);
#10871=ADVANCED_FACE('',(#1133),#10585,.T.);
#10872=ADVANCED_FACE('',(#1134),#345,.F.);
#10873=ADVANCED_FACE('',(#1135),#346,.F.);
#10874=ADVANCED_FACE('',(#1136),#347,.T.);
#10875=ADVANCED_FACE('',(#1137),#10586,.F.);
#10876=ADVANCED_FACE('',(#1138),#10587,.F.);
#10877=ADVANCED_FACE('',(#1139),#10588,.F.);
#10878=ADVANCED_FACE('',(#1140),#826,.F.);
#10879=ADVANCED_FACE('',(#1141),#348,.F.);
#10880=ADVANCED_FACE('',(#1142),#349,.T.);
#10881=ADVANCED_FACE('',(#1143),#827,.F.);
#10882=ADVANCED_FACE('',(#1144),#10589,.T.);
#10883=ADVANCED_FACE('',(#1145),#828,.T.);
#10884=ADVANCED_FACE('',(#1146,#305),#350,.F.);
#10885=ADVANCED_FACE('',(#1147,#306),#351,.F.);
#10886=ADVANCED_FACE('',(#1148),#352,.F.);
#10887=ADVANCED_FACE('',(#1149),#10590,.T.);
#10888=ADVANCED_FACE('',(#1150),#353,.F.);
#10889=ADVANCED_FACE('',(#1151),#10591,.T.);
#10890=ADVANCED_FACE('',(#1152),#829,.F.);
#10891=ADVANCED_FACE('',(#1153),#354,.T.);
#10892=ADVANCED_FACE('',(#1154),#355,.F.);
#10893=ADVANCED_FACE('',(#1155),#356,.F.);
#10894=ADVANCED_FACE('',(#1156),#10592,.T.);
#10895=ADVANCED_FACE('',(#1157),#357,.T.);
#10896=ADVANCED_FACE('',(#1158),#358,.T.);
#10897=ADVANCED_FACE('',(#1159),#359,.T.);
#10898=ADVANCED_FACE('',(#1160),#360,.F.);
#10899=ADVANCED_FACE('',(#1161),#10593,.T.);
#10900=ADVANCED_FACE('',(#1162),#361,.F.);
#10901=ADVANCED_FACE('',(#1163),#362,.F.);
#10902=ADVANCED_FACE('',(#1164),#363,.T.);
#10903=ADVANCED_FACE('',(#1165),#10594,.F.);
#10904=ADVANCED_FACE('',(#1166),#10595,.F.);
#10905=ADVANCED_FACE('',(#1167),#10596,.F.);
#10906=ADVANCED_FACE('',(#1168),#830,.F.);
#10907=ADVANCED_FACE('',(#1169),#364,.F.);
#10908=ADVANCED_FACE('',(#1170),#365,.T.);
#10909=ADVANCED_FACE('',(#1171),#831,.F.);
#10910=ADVANCED_FACE('',(#1172),#10597,.T.);
#10911=ADVANCED_FACE('',(#1173),#832,.T.);
#10912=ADVANCED_FACE('',(#1174),#366,.F.);
#10913=ADVANCED_FACE('',(#1175),#10598,.T.);
#10914=ADVANCED_FACE('',(#1176),#367,.F.);
#10915=ADVANCED_FACE('',(#1177),#10599,.T.);
#10916=ADVANCED_FACE('',(#1178),#833,.F.);
#10917=ADVANCED_FACE('',(#1179),#368,.T.);
#10918=ADVANCED_FACE('',(#1180),#369,.F.);
#10919=ADVANCED_FACE('',(#1181),#370,.F.);
#10920=ADVANCED_FACE('',(#1182),#10600,.T.);
#10921=ADVANCED_FACE('',(#1183),#371,.T.);
#10922=ADVANCED_FACE('',(#1184),#372,.T.);
#10923=ADVANCED_FACE('',(#1185),#373,.T.);
#10924=ADVANCED_FACE('',(#1186),#374,.F.);
#10925=ADVANCED_FACE('',(#1187),#10601,.T.);
#10926=ADVANCED_FACE('',(#1188),#375,.F.);
#10927=ADVANCED_FACE('',(#1189),#376,.F.);
#10928=ADVANCED_FACE('',(#1190),#377,.T.);
#10929=ADVANCED_FACE('',(#1191),#10602,.F.);
#10930=ADVANCED_FACE('',(#1192),#10603,.F.);
#10931=ADVANCED_FACE('',(#1193),#10604,.F.);
#10932=ADVANCED_FACE('',(#1194),#834,.F.);
#10933=ADVANCED_FACE('',(#1195),#378,.F.);
#10934=ADVANCED_FACE('',(#1196),#379,.T.);
#10935=ADVANCED_FACE('',(#1197),#835,.F.);
#10936=ADVANCED_FACE('',(#1198,#307),#380,.F.);
#10937=ADVANCED_FACE('',(#1199,#308),#381,.F.);
#10938=ADVANCED_FACE('',(#1200),#10605,.T.);
#10939=ADVANCED_FACE('',(#1201),#10606,.T.);
#10940=ADVANCED_FACE('',(#1202),#836,.F.);
#10941=ADVANCED_FACE('',(#1203),#382,.F.);
#10942=ADVANCED_FACE('',(#1204),#383,.F.);
#10943=ADVANCED_FACE('',(#1205),#10607,.T.);
#10944=ADVANCED_FACE('',(#1206),#384,.T.);
#10945=ADVANCED_FACE('',(#1207),#385,.T.);
#10946=ADVANCED_FACE('',(#1208),#386,.T.);
#10947=ADVANCED_FACE('',(#1209),#387,.F.);
#10948=ADVANCED_FACE('',(#1210),#10608,.T.);
#10949=ADVANCED_FACE('',(#1211),#388,.F.);
#10950=ADVANCED_FACE('',(#1212),#389,.F.);
#10951=ADVANCED_FACE('',(#1213),#390,.T.);
#10952=ADVANCED_FACE('',(#1214),#10609,.F.);
#10953=ADVANCED_FACE('',(#1215),#10610,.F.);
#10954=ADVANCED_FACE('',(#1216),#10611,.F.);
#10955=ADVANCED_FACE('',(#1217),#873,.T.);
#10956=ADVANCED_FACE('',(#1218),#874,.T.);
#10957=ADVANCED_FACE('',(#1219),#10612,.T.);
#10958=ADVANCED_FACE('',(#1220),#10613,.T.);
#10959=ADVANCED_FACE('',(#1221),#875,.T.);
#10960=ADVANCED_FACE('',(#1222),#876,.T.);
#10961=ADVANCED_FACE('',(#1223),#877,.T.);
#10962=ADVANCED_FACE('',(#1224),#878,.F.);
#10963=ADVANCED_FACE('',(#1225),#879,.F.);
#10964=ADVANCED_FACE('',(#1226),#10614,.F.);
#10965=ADVANCED_FACE('',(#1227),#10615,.F.);
#10966=ADVANCED_FACE('',(#1228),#880,.F.);
#10967=ADVANCED_FACE('',(#1229),#881,.F.);
#10968=ADVANCED_FACE('',(#1230),#882,.F.);
#10969=ADVANCED_FACE('',(#1231),#195,.T.);
#10970=ADVANCED_FACE('',(#1232),#196,.T.);
#10971=ADVANCED_FACE('',(#1233),#197,.T.);
#10972=ADVANCED_FACE('',(#1234),#198,.T.);
#10973=ADVANCED_FACE('',(#1235),#199,.T.);
#10974=ADVANCED_FACE('',(#1236),#200,.T.);
#10975=ADVANCED_FACE('',(#1237),#201,.T.);
#10976=ADVANCED_FACE('',(#1238),#202,.T.);
#10977=ADVANCED_FACE('',(#1239),#203,.T.);
#10978=ADVANCED_FACE('',(#1240),#204,.T.);
#10979=ADVANCED_FACE('',(#1241),#205,.T.);
#10980=ADVANCED_FACE('',(#1242),#206,.T.);
#10981=ADVANCED_FACE('',(#1243),#207,.T.);
#10982=ADVANCED_FACE('',(#1244),#208,.T.);
#10983=ADVANCED_FACE('',(#1245),#209,.T.);
#10984=ADVANCED_FACE('',(#1246),#210,.T.);
#10985=ADVANCED_FACE('',(#1247),#211,.T.);
#10986=ADVANCED_FACE('',(#1248),#212,.T.);
#10987=ADVANCED_FACE('',(#1249),#213,.T.);
#10988=ADVANCED_FACE('',(#1250),#214,.T.);
#10989=ADVANCED_FACE('',(#1251),#75,.F.);
#10990=ADVANCED_FACE('',(#1252),#76,.F.);
#10991=ADVANCED_FACE('',(#1253),#77,.T.);
#10992=ADVANCED_FACE('',(#1254),#883,.F.);
#10993=ADVANCED_FACE('',(#1255),#10616,.T.);
#10994=ADVANCED_FACE('',(#1256),#10617,.T.);
#10995=ADVANCED_FACE('',(#1257),#884,.T.);
#10996=ADVANCED_FACE('',(#1258),#78,.F.);
#10997=ADVANCED_FACE('',(#1259),#79,.F.);
#10998=ADVANCED_FACE('',(#1260),#10618,.T.);
#10999=ADVANCED_FACE('',(#1261),#80,.T.);
#11000=ADVANCED_FACE('',(#1262),#27,.F.);
#11001=ADVANCED_FACE('',(#1263),#81,.F.);
#11002=ADVANCED_FACE('',(#1264),#28,.T.);
#11003=ADVANCED_FACE('',(#1265),#215,.T.);
#11004=ADVANCED_FACE('',(#1266),#82,.T.);
#11005=ADVANCED_FACE('',(#1267),#885,.T.);
#11006=ADVANCED_FACE('',(#1268),#83,.F.);
#11007=ADVANCED_FACE('',(#1269),#10619,.F.);
#11008=ADVANCED_FACE('',(#1270),#886,.T.);
#11009=ADVANCED_FACE('',(#1271),#84,.F.);
#11010=ADVANCED_FACE('',(#1272),#10620,.T.);
#11011=ADVANCED_FACE('',(#1273),#10621,.T.);
#11012=ADVANCED_FACE('',(#1274),#887,.F.);
#11013=ADVANCED_FACE('',(#1275),#85,.T.);
#11014=ADVANCED_FACE('',(#1276),#888,.T.);
#11015=ADVANCED_FACE('',(#1277),#86,.F.);
#11016=ADVANCED_FACE('',(#1278),#889,.T.);
#11017=ADVANCED_FACE('',(#1279),#10622,.T.);
#11018=ADVANCED_FACE('',(#1280),#87,.T.);
#11019=ADVANCED_FACE('',(#1281),#88,.F.);
#11020=ADVANCED_FACE('',(#1282),#29,.T.);
#11021=ADVANCED_FACE('',(#1283),#30,.F.);
#11022=ADVANCED_FACE('',(#1284),#89,.T.);
#11023=ADVANCED_FACE('',(#1285),#10623,.T.);
#11024=ADVANCED_FACE('',(#1286),#90,.F.);
#11025=ADVANCED_FACE('',(#1287),#91,.F.);
#11026=ADVANCED_FACE('',(#1288),#890,.T.);
#11027=ADVANCED_FACE('',(#1289),#92,.T.);
#11028=ADVANCED_FACE('',(#1290),#93,.F.);
#11029=ADVANCED_FACE('',(#1291),#94,.T.);
#11030=ADVANCED_FACE('',(#1292),#891,.T.);
#11031=ADVANCED_FACE('',(#1293),#10624,.T.);
#11032=ADVANCED_FACE('',(#1294),#10625,.F.);
#11033=ADVANCED_FACE('',(#1295),#892,.T.);
#11034=ADVANCED_FACE('',(#1296),#10626,.F.);
#11035=ADVANCED_FACE('',(#1297),#95,.F.);
#11036=ADVANCED_FACE('',(#1298),#893,.T.);
#11037=ADVANCED_FACE('',(#1299),#96,.T.);
#11038=ADVANCED_FACE('',(#1300),#216,.T.);
#11039=ADVANCED_FACE('',(#1301),#10627,.T.);
#11040=ADVANCED_FACE('',(#1302),#10628,.T.);
#11041=ADVANCED_FACE('',(#1303),#894,.F.);
#11042=ADVANCED_FACE('',(#1304),#97,.F.);
#11043=ADVANCED_FACE('',(#1305),#98,.F.);
#11044=ADVANCED_FACE('',(#1306),#99,.F.);
#11045=ADVANCED_FACE('',(#1307),#100,.T.);
#11046=ADVANCED_FACE('',(#1308),#895,.T.);
#11047=ADVANCED_FACE('',(#1309),#101,.F.);
#11048=ADVANCED_FACE('',(#1310),#102,.F.);
#11049=ADVANCED_FACE('',(#1311),#896,.T.);
#11050=ADVANCED_FACE('',(#1312),#31,.T.);
#11051=ADVANCED_FACE('',(#1313),#32,.F.);
#11052=ADVANCED_FACE('',(#1314),#10629,.F.);
#11053=ADVANCED_FACE('',(#1315),#10630,.T.);
#11054=ADVANCED_FACE('',(#1316),#897,.F.);
#11055=ADVANCED_FACE('',(#1317),#10631,.T.);
#11056=ADVANCED_FACE('',(#1318),#103,.T.);
#11057=ADVANCED_FACE('',(#1319),#104,.F.);
#11058=ADVANCED_FACE('',(#1320),#105,.T.);
#11059=ADVANCED_FACE('',(#1321),#106,.F.);
#11060=ADVANCED_FACE('',(#1322),#107,.T.);
#11061=ADVANCED_FACE('',(#1323),#898,.F.);
#11062=ADVANCED_FACE('',(#1324),#10632,.T.);
#11063=ADVANCED_FACE('',(#1325),#10633,.T.);
#11064=ADVANCED_FACE('',(#1326),#899,.T.);
#11065=ADVANCED_FACE('',(#1327),#10634,.F.);
#11066=ADVANCED_FACE('',(#1328),#900,.T.);
#11067=ADVANCED_FACE('',(#1329),#108,.F.);
#11068=ADVANCED_FACE('',(#1330),#901,.T.);
#11069=ADVANCED_FACE('',(#1331),#10635,.T.);
#11070=ADVANCED_FACE('',(#1332),#109,.F.);
#11071=ADVANCED_FACE('',(#1333),#902,.F.);
#11072=ADVANCED_FACE('',(#1334),#10636,.T.);
#11073=ADVANCED_FACE('',(#1335),#903,.T.);
#11074=ADVANCED_FACE('',(#1336),#110,.F.);
#11075=ADVANCED_FACE('',(#1337),#111,.F.);
#11076=ADVANCED_FACE('',(#1338),#10637,.T.);
#11077=ADVANCED_FACE('',(#1339),#112,.T.);
#11078=ADVANCED_FACE('',(#1340),#33,.F.);
#11079=ADVANCED_FACE('',(#1341),#34,.T.);
#11080=ADVANCED_FACE('',(#1342),#113,.F.);
#11081=ADVANCED_FACE('',(#1343),#904,.T.);
#11082=ADVANCED_FACE('',(#1344),#10638,.T.);
#11083=ADVANCED_FACE('',(#1345),#905,.T.);
#11084=ADVANCED_FACE('',(#1346),#35,.F.);
#11085=ADVANCED_FACE('',(#1347),#36,.T.);
#11086=ADVANCED_FACE('',(#1348),#217,.T.);
#11087=ADVANCED_FACE('',(#1349),#114,.T.);
#11088=ADVANCED_FACE('',(#1350),#906,.T.);
#11089=ADVANCED_FACE('',(#1351),#115,.F.);
#11090=ADVANCED_FACE('',(#1352),#10639,.F.);
#11091=ADVANCED_FACE('',(#1353),#907,.T.);
#11092=ADVANCED_FACE('',(#1354),#10640,.F.);
#11093=ADVANCED_FACE('',(#1355),#10641,.T.);
#11094=ADVANCED_FACE('',(#1356),#908,.T.);
#11095=ADVANCED_FACE('',(#1357),#10642,.F.);
#11096=ADVANCED_FACE('',(#1358),#10643,.F.);
#11097=ADVANCED_FACE('',(#1359),#909,.T.);
#11098=ADVANCED_FACE('',(#1360),#910,.T.);
#11099=ADVANCED_FACE('',(#1361),#116,.F.);
#11100=ADVANCED_FACE('',(#1362),#911,.T.);
#11101=ADVANCED_FACE('',(#1363),#10644,.T.);
#11102=ADVANCED_FACE('',(#1364),#117,.T.);
#11103=ADVANCED_FACE('',(#1365),#118,.F.);
#11104=ADVANCED_FACE('',(#1366),#119,.F.);
#11105=ADVANCED_FACE('',(#1367),#912,.T.);
#11106=ADVANCED_FACE('',(#1368),#120,.F.);
#11107=ADVANCED_FACE('',(#1369),#121,.T.);
#11108=ADVANCED_FACE('',(#1370),#122,.F.);
#11109=ADVANCED_FACE('',(#1371),#123,.T.);
#11110=ADVANCED_FACE('',(#1372),#913,.T.);
#11111=ADVANCED_FACE('',(#1373),#10645,.T.);
#11112=ADVANCED_FACE('',(#1374),#914,.F.);
#11113=ADVANCED_FACE('',(#1375),#10646,.T.);
#11114=ADVANCED_FACE('',(#1376),#10647,.F.);
#11115=ADVANCED_FACE('',(#1377),#10648,.T.);
#11116=ADVANCED_FACE('',(#1378),#915,.F.);
#11117=ADVANCED_FACE('',(#1379),#124,.F.);
#11118=ADVANCED_FACE('',(#1380),#916,.T.);
#11119=ADVANCED_FACE('',(#1381),#125,.F.);
#11120=ADVANCED_FACE('',(#1382),#126,.F.);
#11121=ADVANCED_FACE('',(#1383),#37,.T.);
#11122=ADVANCED_FACE('',(#1384),#38,.F.);
#11123=ADVANCED_FACE('',(#1385),#10649,.F.);
#11124=ADVANCED_FACE('',(#1386),#10650,.T.);
#11125=ADVANCED_FACE('',(#1387),#917,.F.);
#11126=ADVANCED_FACE('',(#1388),#10651,.F.);
#11127=ADVANCED_FACE('',(#1389),#10652,.F.);
#11128=ADVANCED_FACE('',(#1390),#127,.F.);
#11129=ADVANCED_FACE('',(#1391),#918,.T.);
#11130=ADVANCED_FACE('',(#1392),#10653,.F.);
#11131=ADVANCED_FACE('',(#1393),#919,.T.);
#11132=ADVANCED_FACE('',(#1394),#128,.F.);
#11133=ADVANCED_FACE('',(#1395),#39,.F.);
#11134=ADVANCED_FACE('',(#1396),#920,.F.);
#11135=ADVANCED_FACE('',(#1397),#10654,.T.);
#11136=ADVANCED_FACE('',(#1398),#921,.T.);
#11137=ADVANCED_FACE('',(#1399),#129,.F.);
#11138=ADVANCED_FACE('',(#1400),#922,.T.);
#11139=ADVANCED_FACE('',(#1401),#10655,.T.);
#11140=ADVANCED_FACE('',(#1402),#130,.F.);
#11141=ADVANCED_FACE('',(#1403),#131,.F.);
#11142=ADVANCED_FACE('',(#1404),#40,.T.);
#11143=ADVANCED_FACE('',(#1405),#10656,.F.);
#11144=ADVANCED_FACE('',(#1406),#10657,.T.);
#11145=ADVANCED_FACE('',(#1407),#923,.T.);
#11146=ADVANCED_FACE('',(#1408),#132,.T.);
#11147=ADVANCED_FACE('',(#1409),#924,.T.);
#11148=ADVANCED_FACE('',(#1410),#133,.F.);
#11149=ADVANCED_FACE('',(#1411),#10658,.T.);
#11150=ADVANCED_FACE('',(#1412),#134,.F.);
#11151=ADVANCED_FACE('',(#1413),#10659,.T.);
#11152=ADVANCED_FACE('',(#1414),#135,.T.);
#11153=ADVANCED_FACE('',(#1415),#136,.T.);
#11154=ADVANCED_FACE('',(#1416),#925,.F.);
#11155=ADVANCED_FACE('',(#1417),#10660,.T.);
#11156=ADVANCED_FACE('',(#1418),#926,.T.);
#11157=ADVANCED_FACE('',(#1419),#10661,.T.);
#11158=ADVANCED_FACE('',(#1420),#137,.F.);
#11159=ADVANCED_FACE('',(#1421),#138,.F.);
#11160=ADVANCED_FACE('',(#1422),#927,.T.);
#11161=ADVANCED_FACE('',(#1423),#139,.F.);
#11162=ADVANCED_FACE('',(#1424),#928,.T.);
#11163=ADVANCED_FACE('',(#1425),#140,.T.);
#11164=ADVANCED_FACE('',(#1426),#218,.T.);
#11165=ADVANCED_FACE('',(#1427),#10662,.F.);
#11166=ADVANCED_FACE('',(#1428),#10663,.T.);
#11167=ADVANCED_FACE('',(#1429),#929,.T.);
#11168=ADVANCED_FACE('',(#1430),#930,.T.);
#11169=ADVANCED_FACE('',(#1431),#10664,.T.);
#11170=ADVANCED_FACE('',(#1432),#931,.T.);
#11171=ADVANCED_FACE('',(#1433),#141,.F.);
#11172=ADVANCED_FACE('',(#1434),#142,.T.);
#11173=ADVANCED_FACE('',(#1435),#143,.T.);
#11174=ADVANCED_FACE('',(#1436),#41,.T.);
#11175=ADVANCED_FACE('',(#1437),#10665,.F.);
#11176=ADVANCED_FACE('',(#1438),#144,.F.);
#11177=ADVANCED_FACE('',(#1439),#145,.F.);
#11178=ADVANCED_FACE('',(#1440),#10666,.T.);
#11179=ADVANCED_FACE('',(#1441),#42,.F.);
#11180=ADVANCED_FACE('',(#1442),#146,.F.);
#11181=ADVANCED_FACE('',(#1443),#932,.F.);
#11182=ADVANCED_FACE('',(#1444),#10667,.F.);
#11183=ADVANCED_FACE('',(#1445),#43,.F.);
#11184=ADVANCED_FACE('',(#1446),#44,.F.);
#11185=ADVANCED_FACE('',(#1447),#933,.F.);
#11186=ADVANCED_FACE('',(#1448),#934,.F.);
#11187=ADVANCED_FACE('',(#1449),#10668,.F.);
#11188=ADVANCED_FACE('',(#1450),#45,.F.);
#11189=ADVANCED_FACE('',(#1451),#46,.F.);
#11190=ADVANCED_FACE('',(#1452),#147,.T.);
#11191=ADVANCED_FACE('',(#1453),#935,.F.);
#11192=ADVANCED_FACE('',(#1454),#148,.F.);
#11193=ADVANCED_FACE('',(#1455),#936,.F.);
#11194=ADVANCED_FACE('',(#1456),#10669,.F.);
#11195=ADVANCED_FACE('',(#1457),#937,.F.);
#11196=ADVANCED_FACE('',(#1458),#149,.T.);
#11197=ADVANCED_FACE('',(#1459),#10670,.T.);
#11198=ADVANCED_FACE('',(#1460),#10671,.F.);
#11199=ADVANCED_FACE('',(#1461),#47,.F.);
#11200=ADVANCED_FACE('',(#1462),#48,.F.);
#11201=ADVANCED_FACE('',(#1463),#49,.F.);
#11202=ADVANCED_FACE('',(#1464),#150,.T.);
#11203=ADVANCED_FACE('',(#1465),#938,.T.);
#11204=ADVANCED_FACE('',(#1466),#50,.F.);
#11205=ADVANCED_FACE('',(#1467),#10672,.F.);
#11206=ADVANCED_FACE('',(#1468),#939,.F.);
#11207=ADVANCED_FACE('',(#1469),#151,.F.);
#11208=ADVANCED_FACE('',(#1470),#10673,.F.);
#11209=ADVANCED_FACE('',(#1471),#10674,.T.);
#11210=ADVANCED_FACE('',(#1472),#10675,.T.);
#11211=ADVANCED_FACE('',(#1473),#940,.F.);
#11212=ADVANCED_FACE('',(#1474),#10676,.F.);
#11213=ADVANCED_FACE('',(#1475),#152,.T.);
#11214=ADVANCED_FACE('',(#1476),#51,.F.);
#11215=ADVANCED_FACE('',(#1477),#941,.F.);
#11216=ADVANCED_FACE('',(#1478),#942,.T.);
#11217=ADVANCED_FACE('',(#1479),#153,.T.);
#11218=ADVANCED_FACE('',(#1480),#52,.F.);
#11219=ADVANCED_FACE('',(#1481),#10677,.F.);
#11220=ADVANCED_FACE('',(#1482),#10678,.T.);
#11221=ADVANCED_FACE('',(#1483),#154,.T.);
#11222=ADVANCED_FACE('',(#1484),#943,.F.);
#11223=ADVANCED_FACE('',(#1485),#10679,.F.);
#11224=ADVANCED_FACE('',(#1486),#10680,.F.);
#11225=ADVANCED_FACE('',(#1487),#944,.F.);
#11226=ADVANCED_FACE('',(#1488),#10681,.T.);
#11227=ADVANCED_FACE('',(#1489),#155,.T.);
#11228=ADVANCED_FACE('',(#1490),#945,.F.);
#11229=ADVANCED_FACE('',(#1491),#10682,.F.);
#11230=ADVANCED_FACE('',(#1492),#156,.F.);
#11231=ADVANCED_FACE('',(#1493),#53,.F.);
#11232=ADVANCED_FACE('',(#1494),#946,.T.);
#11233=ADVANCED_FACE('',(#1495),#157,.T.);
#11234=ADVANCED_FACE('',(#1496),#54,.F.);
#11235=ADVANCED_FACE('',(#1497),#158,.T.);
#11236=ADVANCED_FACE('',(#1498),#159,.T.);
#11237=ADVANCED_FACE('',(#1499),#55,.F.);
#11238=ADVANCED_FACE('',(#1500),#56,.F.);
#11239=ADVANCED_FACE('',(#1501),#947,.F.);
#11240=ADVANCED_FACE('',(#1502),#10683,.T.);
#11241=ADVANCED_FACE('',(#1503),#10684,.T.);
#11242=ADVANCED_FACE('',(#1504),#10685,.F.);
#11243=ADVANCED_FACE('',(#1505),#10686,.F.);
#11244=ADVANCED_FACE('',(#1506),#160,.T.);
#11245=ADVANCED_FACE('',(#1507),#10687,.T.);
#11246=ADVANCED_FACE('',(#1508),#948,.F.);
#11247=ADVANCED_FACE('',(#1509),#10688,.F.);
#11248=ADVANCED_FACE('',(#1510),#10689,.F.);
#11249=ADVANCED_FACE('',(#1511),#949,.F.);
#11250=ADVANCED_FACE('',(#1512),#161,.T.);
#11251=ADVANCED_FACE('',(#1513),#950,.T.);
#11252=ADVANCED_FACE('',(#1514),#57,.F.);
#11253=ADVANCED_FACE('',(#1515),#58,.F.);
#11254=ADVANCED_FACE('',(#1516),#162,.T.);
#11255=ADVANCED_FACE('',(#1517),#951,.T.);
#11256=ADVANCED_FACE('',(#1518),#59,.F.);
#11257=ADVANCED_FACE('',(#1519),#60,.F.);
#11258=ADVANCED_FACE('',(#1520),#163,.T.);
#11259=ADVANCED_FACE('',(#1521),#10690,.T.);
#11260=ADVANCED_FACE('',(#1522),#952,.F.);
#11261=ADVANCED_FACE('',(#1523),#164,.F.);
#11262=ADVANCED_FACE('',(#1524),#10691,.F.);
#11263=ADVANCED_FACE('',(#1525),#953,.F.);
#11264=ADVANCED_FACE('',(#1526),#10692,.F.);
#11265=ADVANCED_FACE('',(#1527),#954,.F.);
#11266=ADVANCED_FACE('',(#1528),#10693,.T.);
#11267=ADVANCED_FACE('',(#1529),#10694,.T.);
#11268=ADVANCED_FACE('',(#1530),#10695,.F.);
#11269=ADVANCED_FACE('',(#1531),#165,.F.);
#11270=ADVANCED_FACE('',(#1532),#955,.F.);
#11271=ADVANCED_FACE('',(#1533),#166,.T.);
#11272=ADVANCED_FACE('',(#1534),#167,.T.);
#11273=ADVANCED_FACE('',(#1535),#61,.F.);
#11274=ADVANCED_FACE('',(#1536),#62,.F.);
#11275=ADVANCED_FACE('',(#1537),#63,.F.);
#11276=ADVANCED_FACE('',(#1538),#956,.T.);
#11277=ADVANCED_FACE('',(#1539),#168,.T.);
#11278=ADVANCED_FACE('',(#1540),#64,.F.);
#11279=ADVANCED_FACE('',(#1541),#10696,.T.);
#11280=ADVANCED_FACE('',(#1542),#169,.T.);
#11281=ADVANCED_FACE('',(#1543),#957,.F.);
#11282=ADVANCED_FACE('',(#1544),#10697,.F.);
#11283=ADVANCED_FACE('',(#1545),#10698,.F.);
#11284=ADVANCED_FACE('',(#1546),#10699,.T.);
#11285=ADVANCED_FACE('',(#1547),#170,.T.);
#11286=ADVANCED_FACE('',(#1548),#958,.F.);
#11287=ADVANCED_FACE('',(#1549),#10700,.F.);
#11288=ADVANCED_FACE('',(#1550),#10701,.F.);
#11289=ADVANCED_FACE('',(#1551),#959,.T.);
#11290=ADVANCED_FACE('',(#1552),#171,.T.);
#11291=ADVANCED_FACE('',(#1553),#65,.F.);
#11292=ADVANCED_FACE('',(#1554),#172,.T.);
#11293=ADVANCED_FACE('',(#1555),#66,.F.);
#11294=ADVANCED_FACE('',(#1556),#960,.F.);
#11295=ADVANCED_FACE('',(#1557),#10702,.T.);
#11296=ADVANCED_FACE('',(#1558),#10703,.T.);
#11297=ADVANCED_FACE('',(#1559),#961,.F.);
#11298=ADVANCED_FACE('',(#1560),#173,.F.);
#11299=ADVANCED_FACE('',(#1561),#10704,.F.);
#11300=ADVANCED_FACE('',(#1562),#962,.F.);
#11301=ADVANCED_FACE('',(#1563),#10705,.F.);
#11302=ADVANCED_FACE('',(#1564),#10706,.F.);
#11303=ADVANCED_FACE('',(#1565),#963,.F.);
#11304=ADVANCED_FACE('',(#1566),#174,.T.);
#11305=ADVANCED_FACE('',(#1567),#964,.T.);
#11306=ADVANCED_FACE('',(#1568),#67,.F.);
#11307=ADVANCED_FACE('',(#1569),#68,.F.);
#11308=ADVANCED_FACE('',(#1570),#69,.F.);
#11309=ADVANCED_FACE('',(#1571),#70,.F.);
#11310=ADVANCED_FACE('',(#1572),#175,.T.);
#11311=ADVANCED_FACE('',(#1573),#10707,.T.);
#11312=ADVANCED_FACE('',(#1574),#10708,.F.);
#11313=ADVANCED_FACE('',(#1575),#10709,.F.);
#11314=ADVANCED_FACE('',(#1576),#10710,.F.);
#11315=ADVANCED_FACE('',(#1577),#176,.F.);
#11316=ADVANCED_FACE('',(#1578),#177,.T.);
#11317=ADVANCED_FACE('',(#1579),#965,.F.);
#11318=ADVANCED_FACE('',(#1580),#71,.F.);
#11319=ADVANCED_FACE('',(#1581),#72,.F.);
#11320=ADVANCED_FACE('',(#1582),#966,.F.);
#11321=ADVANCED_FACE('',(#1583),#10711,.F.);
#11322=ADVANCED_FACE('',(#1584),#10712,.F.);
#11323=ADVANCED_FACE('',(#1585),#73,.F.);
#11324=ADVANCED_FACE('',(#1586),#74,.F.);
#11325=ADVANCED_FACE('',(#1587),#178,.F.);
#11326=ADVANCED_FACE('',(#1588),#219,.T.);
#11327=ADVANCED_FACE('',(#1589),#220,.T.);
#11328=ADVANCED_FACE('',(#1590),#221,.T.);
#11329=ADVANCED_FACE('',(#1591),#222,.T.);
#11330=ADVANCED_FACE('',(#1592),#223,.T.);
#11331=ADVANCED_FACE('',(#1593),#224,.T.);
#11332=ADVANCED_FACE('',(#1594),#225,.T.);
#11333=ADVANCED_FACE('',(#1595),#226,.T.);
#11334=ADVANCED_FACE('',(#1596),#227,.T.);
#11335=ADVANCED_FACE('',(#1597),#228,.T.);
#11336=ADVANCED_FACE('',(#1598),#229,.T.);
#11337=ADVANCED_FACE('',(#1599),#230,.T.);
#11338=ADVANCED_FACE('',(#1600),#231,.T.);
#11339=ADVANCED_FACE('',(#1601),#232,.T.);
#11340=ADVANCED_FACE('',(#1602),#233,.T.);
#11341=ADVANCED_FACE('',(#1603),#234,.T.);
#11342=ADVANCED_FACE('',(#1604),#235,.T.);
#11343=ADVANCED_FACE('',(#1605),#236,.T.);
#11344=ADVANCED_FACE('',(#1606),#237,.T.);
#11345=ADVANCED_FACE('',(#1607),#238,.T.);
#11346=ADVANCED_FACE('',(#1608),#10713,.T.);
#11347=ADVANCED_FACE('',(#1609),#179,.T.);
#11348=ADVANCED_FACE('',(#1610),#180,.T.);
#11349=ADVANCED_FACE('',(#1611),#181,.F.);
#11350=ADVANCED_FACE('',(#1612),#182,.F.);
#11351=ADVANCED_FACE('',(#1613),#967,.T.);
#11352=ADVANCED_FACE('',(#1614),#10714,.T.);
#11353=ADVANCED_FACE('',(#1615),#968,.T.);
#11354=ADVANCED_FACE('',(#1616),#239,.T.);
#11355=ADVANCED_FACE('',(#1617),#183,.T.);
#11356=ADVANCED_FACE('',(#1618),#184,.T.);
#11357=ADVANCED_FACE('',(#1619),#185,.T.);
#11358=ADVANCED_FACE('',(#1620),#186,.F.);
#11359=ADVANCED_FACE('',(#1621),#969,.T.);
#11360=ADVANCED_FACE('',(#1622),#970,.T.);
#11361=ADVANCED_FACE('',(#1623),#187,.F.);
#11362=ADVANCED_FACE('',(#1624),#188,.F.);
#11363=ADVANCED_FACE('',(#1625),#971,.T.);
#11364=ADVANCED_FACE('',(#1626),#10715,.T.);
#11365=ADVANCED_FACE('',(#1627),#189,.F.);
#11366=ADVANCED_FACE('',(#1628),#240,.T.);
#11367=ADVANCED_FACE('',(#1629),#241,.T.);
#11368=ADVANCED_FACE('',(#1630),#190,.T.);
#11369=ADVANCED_FACE('',(#1631),#191,.T.);
#11370=ADVANCED_FACE('',(#1632),#972,.T.);
#11371=ADVANCED_FACE('',(#1633),#973,.T.);
#11372=ADVANCED_FACE('',(#1634),#192,.F.);
#11373=ADVANCED_FACE('',(#1635),#10716,.T.);
#11374=ADVANCED_FACE('',(#1636),#974,.T.);
#11375=ADVANCED_FACE('',(#1637),#242,.T.);
#11376=ADVANCED_FACE('',(#1638),#193,.T.);
#11377=ADVANCED_FACE('',(#1639),#194,.F.);
#11378=ADVANCED_FACE('',(#1640),#975,.T.);
#11379=ADVANCED_FACE('',(#1641),#10717,.T.);
#11380=ADVANCED_FACE('',(#1642),#10718,.T.);
#11381=ADVANCED_FACE('',(#1643),#976,.T.);
#11382=ADVANCED_FACE('',(#1644),#977,.T.);
#11383=ADVANCED_FACE('',(#1645),#10719,.T.);
#11384=ADVANCED_FACE('',(#1646),#10720,.T.);
#11385=ADVANCED_FACE('',(#1647),#978,.T.);
#11386=ADVANCED_FACE('',(#1648),#979,.T.);
#11387=ADVANCED_FACE('',(#1649),#10721,.T.);
#11388=ADVANCED_FACE('',(#1650),#10722,.T.);
#11389=ADVANCED_FACE('',(#1651),#980,.T.);
#11390=ADVANCED_FACE('',(#1652),#981,.T.);
#11391=ADVANCED_FACE('',(#1653),#10723,.T.);
#11392=ADVANCED_FACE('',(#1654),#10724,.T.);
#11393=ADVANCED_FACE('',(#1655),#982,.T.);
#11394=ADVANCED_FACE('',(#1656),#983,.T.);
#11395=ADVANCED_FACE('',(#1657),#984,.T.);
#11396=ADVANCED_FACE('',(#1658),#10725,.T.);
#11397=ADVANCED_FACE('',(#1659),#10726,.T.);
#11398=ADVANCED_FACE('',(#1660),#985,.T.);
#11399=ADVANCED_FACE('',(#1661),#986,.T.);
#11400=ADVANCED_FACE('',(#1662),#987,.T.);
#11401=ADVANCED_FACE('',(#1663),#988,.F.);
#11402=ADVANCED_FACE('',(#1664),#989,.F.);
#11403=ADVANCED_FACE('',(#1665),#10727,.F.);
#11404=ADVANCED_FACE('',(#1666),#10728,.F.);
#11405=ADVANCED_FACE('',(#1667),#990,.F.);
#11406=ADVANCED_FACE('',(#1668),#991,.F.);
#11407=ADVANCED_FACE('',(#1669),#992,.F.);
#11408=ADVANCED_FACE('',(#1670),#993,.T.);
#11409=ADVANCED_FACE('',(#1671),#994,.T.);
#11410=ADVANCED_FACE('',(#1672),#10729,.T.);
#11411=ADVANCED_FACE('',(#1673),#10730,.T.);
#11412=ADVANCED_FACE('',(#1674),#995,.T.);
#11413=ADVANCED_FACE('',(#1675),#996,.T.);
#11414=ADVANCED_FACE('',(#1676),#997,.F.);
#11415=ADVANCED_FACE('',(#1677),#998,.F.);
#11416=ADVANCED_FACE('',(#1678),#10731,.F.);
#11417=ADVANCED_FACE('',(#1679),#10732,.F.);
#11418=ADVANCED_FACE('',(#1680),#999,.F.);
#11419=ADVANCED_FACE('',(#1681),#1000,.F.);
#11420=ADVANCED_FACE('',(#1682),#1001,.T.);
#11421=ADVANCED_FACE('',(#1683),#1002,.T.);
#11422=ADVANCED_FACE('',(#1684),#10733,.T.);
#11423=ADVANCED_FACE('',(#1685),#10734,.T.);
#11424=ADVANCED_FACE('',(#1686),#1003,.T.);
#11425=ADVANCED_FACE('',(#1687),#1004,.T.);
#11426=ADVANCED_FACE('',(#1688),#1005,.F.);
#11427=ADVANCED_FACE('',(#1689),#1006,.F.);
#11428=ADVANCED_FACE('',(#1690),#10735,.F.);
#11429=ADVANCED_FACE('',(#1691),#10736,.F.);
#11430=ADVANCED_FACE('',(#1692),#1007,.F.);
#11431=ADVANCED_FACE('',(#1693),#1008,.F.);
#11432=ADVANCED_FACE('',(#1694),#10737,.F.);
#11433=ADVANCED_FACE('',(#1695),#391,.F.);
#11434=ADVANCED_FACE('',(#1696),#392,.T.);
#11435=ADVANCED_FACE('',(#1697),#10738,.T.);
#11436=ADVANCED_FACE('',(#1698,#309),#393,.T.);
#11437=ADVANCED_FACE('',(#1699,#310),#394,.T.);
#11438=ADVANCED_FACE('',(#1700,#311),#395,.F.);
#11439=ADVANCED_FACE('',(#1701),#396,.F.);
#11440=ADVANCED_FACE('',(#1702),#397,.F.);
#11441=ADVANCED_FACE('',(#1703),#398,.F.);
#11442=ADVANCED_FACE('',(#1704),#399,.F.);
#11443=ADVANCED_FACE('',(#1705),#400,.T.);
#11444=ADVANCED_FACE('',(#1706),#401,.T.);
#11445=ADVANCED_FACE('',(#1707),#402,.T.);
#11446=ADVANCED_FACE('',(#1708),#403,.F.);
#11447=ADVANCED_FACE('',(#1709),#404,.F.);
#11448=ADVANCED_FACE('',(#1710),#405,.T.);
#11449=ADVANCED_FACE('',(#1711),#406,.T.);
#11450=ADVANCED_FACE('',(#1712),#407,.T.);
#11451=ADVANCED_FACE('',(#1713),#408,.T.);
#11452=ADVANCED_FACE('',(#1714),#409,.F.);
#11453=ADVANCED_FACE('',(#1715),#410,.T.);
#11454=ADVANCED_FACE('',(#1716),#411,.F.);
#11455=ADVANCED_FACE('',(#1717),#412,.F.);
#11456=ADVANCED_FACE('',(#1718),#413,.F.);
#11457=ADVANCED_FACE('',(#1719),#10739,.T.);
#11458=ADVANCED_FACE('',(#1720),#1009,.F.);
#11459=ADVANCED_FACE('',(#1721),#10740,.F.);
#11460=ADVANCED_FACE('',(#1722),#1010,.F.);
#11461=ADVANCED_FACE('',(#1723),#10741,.F.);
#11462=ADVANCED_FACE('',(#1724),#10742,.T.);
#11463=ADVANCED_FACE('',(#1725),#1011,.T.);
#11464=ADVANCED_FACE('',(#1726),#10743,.T.);
#11465=ADVANCED_FACE('',(#1727),#243,.T.);
#11466=ADVANCED_FACE('',(#1728),#244,.T.);
#11467=ADVANCED_FACE('',(#1729),#245,.T.);
#11468=ADVANCED_FACE('',(#1730),#246,.T.);
#11469=ADVANCED_FACE('',(#1731),#247,.T.);
#11470=ADVANCED_FACE('',(#1732),#248,.T.);
#11471=ADVANCED_FACE('',(#1733),#249,.T.);
#11472=ADVANCED_FACE('',(#1734),#250,.T.);
#11473=ADVANCED_FACE('',(#1735),#251,.T.);
#11474=ADVANCED_FACE('',(#1736),#252,.T.);
#11475=ADVANCED_FACE('',(#1737),#253,.T.);
#11476=ADVANCED_FACE('',(#1738),#254,.T.);
#11477=ADVANCED_FACE('',(#1739),#255,.T.);
#11478=ADVANCED_FACE('',(#1740),#256,.T.);
#11479=ADVANCED_FACE('',(#1741),#257,.T.);
#11480=ADVANCED_FACE('',(#1742),#258,.T.);
#11481=ADVANCED_FACE('',(#1743),#259,.T.);
#11482=ADVANCED_FACE('',(#1744),#260,.T.);
#11483=ADVANCED_FACE('',(#1745),#261,.T.);
#11484=ADVANCED_FACE('',(#1746),#262,.T.);
#11485=ADVANCED_FACE('',(#1747),#263,.T.);
#11486=ADVANCED_FACE('',(#1748),#414,.T.);
#11487=ADVANCED_FACE('',(#1749,#312),#415,.F.);
#11488=ADVANCED_FACE('',(#1750),#10744,.T.);
#11489=ADVANCED_FACE('',(#1751),#10745,.T.);
#11490=ADVANCED_FACE('',(#1752),#10746,.T.);
#11491=ADVANCED_FACE('',(#1753),#10747,.T.);
#11492=ADVANCED_FACE('',(#1754),#10748,.T.);
#11493=ADVANCED_FACE('',(#1755),#10749,.T.);
#11494=ADVANCED_FACE('',(#1756,#313),#416,.T.);
#11495=ADVANCED_FACE('',(#1757,#314),#417,.T.);
#11496=ADVANCED_FACE('',(#1758),#418,.T.);
#11497=CLOSED_SHELL('',(#10750,#10751,#10752,#10753,#10754,#10755,#10756,
#10757,#10758,#10759,#10760,#10761,#10762,#10763,#10764,#10765,#10766,#10767,
#10768,#10769,#10770,#10771,#10772,#10773,#10774,#10775,#10776,#10777,#10778,
#10779,#10780,#10781,#10782,#10783,#10784,#10785,#10786,#10787,#10788,#10789,
#10790,#10791,#10792,#10793,#10794,#10795,#10796,#10797,#10798,#10799,#10800,
#10801,#10802,#10803,#10804,#10805,#10806,#10807,#10808,#10809,#10810,#10811,
#10812,#10813,#10814,#10815,#10816,#10817,#10818,#10819,#10820,#10821,#10822,
#10823,#10824,#10825,#10826,#10827,#10828,#10829,#10830,#10831,#10832,#10833,
#10834,#10835,#10836,#10837,#10838,#10839,#10840,#10841,#10842,#10843,#10844,
#10845,#10846,#10847,#10848,#10849,#10850,#10851,#10852,#10853,#10854,#10855,
#10856,#10857,#10858,#10859,#10860,#10861,#10862,#10863,#10864,#10865,#10866,
#10867,#10868,#10869,#10870,#10871,#10872,#10873,#10874,#10875,#10876,#10877,
#10878,#10879,#10880,#10881,#10882,#10883,#10884,#10885,#10886,#10887,#10888,
#10889,#10890,#10891,#10892,#10893,#10894,#10895,#10896,#10897,#10898,#10899,
#10900,#10901,#10902,#10903,#10904,#10905,#10906,#10907,#10908,#10909,#10910,
#10911,#10912,#10913,#10914,#10915,#10916,#10917,#10918,#10919,#10920,#10921,
#10922,#10923,#10924,#10925,#10926,#10927,#10928,#10929,#10930,#10931,#10932,
#10933,#10934,#10935,#10936,#10937,#10938,#10939,#10940,#10941,#10942,#10943,
#10944,#10945,#10946,#10947,#10948,#10949,#10950,#10951,#10952,#10953,#10954,
#10955,#10956,#10957,#10958,#10959,#10960,#10961,#10962,#10963,#10964,#10965,
#10966,#10967,#10968,#10969,#10970,#10971,#10972,#10973,#10974,#10975,#10976,
#10977,#10978,#10979,#10980,#10981,#10982,#10983,#10984,#10985,#10986,#10987,
#10988,#10989,#10990,#10991,#10992,#10993,#10994,#10995,#10996,#10997,#10998,
#10999,#11000,#11001,#11002,#11003,#11004,#11005,#11006,#11007,#11008,#11009,
#11010,#11011,#11012,#11013,#11014,#11015,#11016,#11017,#11018,#11019,#11020,
#11021,#11022,#11023,#11024,#11025,#11026,#11027,#11028,#11029,#11030,#11031,
#11032,#11033,#11034,#11035,#11036,#11037,#11038,#11039,#11040,#11041,#11042,
#11043,#11044,#11045,#11046,#11047,#11048,#11049,#11050,#11051,#11052,#11053,
#11054,#11055,#11056,#11057,#11058,#11059,#11060,#11061,#11062,#11063,#11064,
#11065,#11066,#11067,#11068,#11069,#11070,#11071,#11072,#11073,#11074,#11075,
#11076,#11077,#11078,#11079,#11080,#11081,#11082,#11083,#11084,#11085,#11086,
#11087,#11088,#11089,#11090,#11091,#11092,#11093,#11094,#11095,#11096,#11097,
#11098,#11099,#11100,#11101,#11102,#11103,#11104,#11105,#11106,#11107,#11108,
#11109,#11110,#11111,#11112,#11113,#11114,#11115,#11116,#11117,#11118,#11119,
#11120,#11121,#11122,#11123,#11124,#11125,#11126,#11127,#11128,#11129,#11130,
#11131,#11132,#11133,#11134,#11135,#11136,#11137,#11138,#11139,#11140,#11141,
#11142,#11143,#11144,#11145,#11146,#11147,#11148,#11149,#11150,#11151,#11152,
#11153,#11154,#11155,#11156,#11157,#11158,#11159,#11160,#11161,#11162,#11163,
#11164,#11165,#11166,#11167,#11168,#11169,#11170,#11171,#11172,#11173,#11174,
#11175,#11176,#11177,#11178,#11179,#11180,#11181,#11182,#11183,#11184,#11185,
#11186,#11187,#11188,#11189,#11190,#11191,#11192,#11193,#11194,#11195,#11196,
#11197,#11198,#11199,#11200,#11201,#11202,#11203,#11204,#11205,#11206,#11207,
#11208,#11209,#11210,#11211,#11212,#11213,#11214,#11215,#11216,#11217,#11218,
#11219,#11220,#11221,#11222,#11223,#11224,#11225,#11226,#11227,#11228,#11229,
#11230,#11231,#11232,#11233,#11234,#11235,#11236,#11237,#11238,#11239,#11240,
#11241,#11242,#11243,#11244,#11245,#11246,#11247,#11248,#11249,#11250,#11251,
#11252,#11253,#11254,#11255,#11256,#11257,#11258,#11259,#11260,#11261,#11262,
#11263,#11264,#11265,#11266,#11267,#11268,#11269,#11270,#11271,#11272,#11273,
#11274,#11275,#11276,#11277,#11278,#11279,#11280,#11281,#11282,#11283,#11284,
#11285,#11286,#11287,#11288,#11289,#11290,#11291,#11292,#11293,#11294,#11295,
#11296,#11297,#11298,#11299,#11300,#11301,#11302,#11303,#11304,#11305,#11306,
#11307,#11308,#11309,#11310,#11311,#11312,#11313,#11314,#11315,#11316,#11317,
#11318,#11319,#11320,#11321,#11322,#11323,#11324,#11325,#11326,#11327,#11328,
#11329,#11330,#11331,#11332,#11333,#11334,#11335,#11336,#11337,#11338,#11339,
#11340,#11341,#11342,#11343,#11344,#11345,#11346,#11347,#11348,#11349,#11350,
#11351,#11352,#11353,#11354,#11355,#11356,#11357,#11358,#11359,#11360,#11361,
#11362,#11363,#11364,#11365,#11366,#11367,#11368,#11369,#11370,#11371,#11372,
#11373,#11374,#11375,#11376,#11377,#11378,#11379,#11380,#11381,#11382,#11383,
#11384,#11385,#11386,#11387,#11388,#11389,#11390,#11391,#11392,#11393,#11394,
#11395,#11396,#11397,#11398,#11399,#11400,#11401,#11402,#11403,#11404,#11405,
#11406,#11407,#11408,#11409,#11410,#11411,#11412,#11413,#11414,#11415,#11416,
#11417,#11418,#11419,#11420,#11421,#11422,#11423,#11424,#11425,#11426,#11427,
#11428,#11429,#11430,#11431,#11432,#11433,#11434,#11435,#11436,#11437,#11438,
#11439,#11440,#11441,#11442,#11443,#11444,#11445,#11446,#11447,#11448,#11449,
#11450,#11451,#11452,#11453,#11454,#11455,#11456));
#11498=CLOSED_SHELL('',(#11457,#11458,#11459,#11460,#11461,#11462,#11463,
#11464,#11465,#11466,#11467,#11468,#11469,#11470,#11471,#11472,#11473,#11474,
#11475,#11476,#11477,#11478,#11479,#11480,#11481,#11482,#11483,#11484,#11485,
#11486,#11487,#11488,#11489,#11490,#11491,#11492,#11493,#11494,#11495,#11496));
#11499=DERIVED_UNIT_ELEMENT(#11503,1.);
#11500=DERIVED_UNIT_ELEMENT(#37627,-3.);
#11501=DERIVED_UNIT_ELEMENT(#11503,1.);
#11502=DERIVED_UNIT_ELEMENT(#37627,-3.);
#11503=(
MASS_UNIT()
NAMED_UNIT(*)
SI_UNIT(.KILO.,.GRAM.)
);
#11504=DERIVED_UNIT((#11499,#11500));
#11505=DERIVED_UNIT((#11501,#11502));
#11506=MEASURE_REPRESENTATION_ITEM('density measure',
POSITIVE_RATIO_MEASURE(7850.),#11504);
#11507=MEASURE_REPRESENTATION_ITEM('density measure',
POSITIVE_RATIO_MEASURE(7850.),#11505);
#11508=PROPERTY_DEFINITION_REPRESENTATION(#11518,#11512);
#11509=PROPERTY_DEFINITION_REPRESENTATION(#11519,#11513);
#11510=PROPERTY_DEFINITION_REPRESENTATION(#11520,#11514);
#11511=PROPERTY_DEFINITION_REPRESENTATION(#11521,#11515);
#11512=REPRESENTATION('material name',(#11516),#37623);
#11513=REPRESENTATION('density',(#11506),#37623);
#11514=REPRESENTATION('material name',(#11517),#37624);
#11515=REPRESENTATION('density',(#11507),#37624);
#11516=DESCRIPTIVE_REPRESENTATION_ITEM('Steel','Steel');
#11517=DESCRIPTIVE_REPRESENTATION_ITEM('Steel','Steel');
#11518=PROPERTY_DEFINITION('material property','material name',#37643);
#11519=PROPERTY_DEFINITION('material property','density of part',#37643);
#11520=PROPERTY_DEFINITION('material property','material name',#37644);
#11521=PROPERTY_DEFINITION('material property','density of part',#37644);
#11522=AXIS2_PLACEMENT_3D('',#16373,#12993,#12994);
#11523=AXIS2_PLACEMENT_3D('',#16374,#12995,#12996);
#11524=AXIS2_PLACEMENT_3D('',#16375,#12997,#12998);
#11525=AXIS2_PLACEMENT_3D('',#16377,#12999,#13000);
#11526=AXIS2_PLACEMENT_3D('',#16380,#13002,#13003);
#11527=AXIS2_PLACEMENT_3D('',#16381,#13004,#13005);
#11528=AXIS2_PLACEMENT_3D('',#16383,#13006,#13007);
#11529=AXIS2_PLACEMENT_3D('',#16386,#13009,#13010);
#11530=AXIS2_PLACEMENT_3D('',#16387,#13011,#13012);
#11531=AXIS2_PLACEMENT_3D('',#16389,#13013,#13014);
#11532=AXIS2_PLACEMENT_3D('',#16392,#13016,#13017);
#11533=AXIS2_PLACEMENT_3D('',#16393,#13018,#13019);
#11534=AXIS2_PLACEMENT_3D('',#16395,#13020,#13021);
#11535=AXIS2_PLACEMENT_3D('',#16398,#13023,#13024);
#11536=AXIS2_PLACEMENT_3D('',#16399,#13025,#13026);
#11537=AXIS2_PLACEMENT_3D('',#16402,#13027,#13028);
#11538=AXIS2_PLACEMENT_3D('',#16403,#13029,#13030);
#11539=AXIS2_PLACEMENT_3D('',#16405,#13031,#13032);
#11540=AXIS2_PLACEMENT_3D('',#16406,#13033,#13034);
#11541=AXIS2_PLACEMENT_3D('',#16407,#13035,#13036);
#11542=AXIS2_PLACEMENT_3D('',#16409,#13037,#13038);
#11543=AXIS2_PLACEMENT_3D('',#16411,#13039,#13040);
#11544=AXIS2_PLACEMENT_3D('',#16413,#13041,#13042);
#11545=AXIS2_PLACEMENT_3D('',#16414,#13043,#13044);
#11546=AXIS2_PLACEMENT_3D('',#16415,#13045,#13046);
#11547=AXIS2_PLACEMENT_3D('',#16417,#13047,#13048);
#11548=AXIS2_PLACEMENT_3D('',#16419,#13049,#13050);
#11549=AXIS2_PLACEMENT_3D('',#16420,#13051,#13052);
#11550=AXIS2_PLACEMENT_3D('',#16421,#13053,#13054);
#11551=AXIS2_PLACEMENT_3D('',#16423,#13055,#13056);
#11552=AXIS2_PLACEMENT_3D('',#16425,#13057,#13058);
#11553=AXIS2_PLACEMENT_3D('',#16427,#13059,#13060);
#11554=AXIS2_PLACEMENT_3D('',#16428,#13061,#13062);
#11555=AXIS2_PLACEMENT_3D('',#16429,#13063,#13064);
#11556=AXIS2_PLACEMENT_3D('',#16432,#13065,#13066);
#11557=AXIS2_PLACEMENT_3D('',#16434,#13067,#13068);
#11558=AXIS2_PLACEMENT_3D('',#16436,#13069,#13070);
#11559=AXIS2_PLACEMENT_3D('',#16437,#13071,#13072);
#11560=AXIS2_PLACEMENT_3D('',#16438,#13073,#13074);
#11561=AXIS2_PLACEMENT_3D('',#16441,#13075,#13076);
#11562=AXIS2_PLACEMENT_3D('',#16443,#13077,#13078);
#11563=AXIS2_PLACEMENT_3D('',#16445,#13079,#13080);
#11564=AXIS2_PLACEMENT_3D('',#16446,#13081,#13082);
#11565=AXIS2_PLACEMENT_3D('',#16447,#13083,#13084);
#11566=AXIS2_PLACEMENT_3D('',#16450,#13085,#13086);
#11567=AXIS2_PLACEMENT_3D('',#16452,#13087,#13088);
#11568=AXIS2_PLACEMENT_3D('',#16454,#13089,#13090);
#11569=AXIS2_PLACEMENT_3D('',#16455,#13091,#13092);
#11570=AXIS2_PLACEMENT_3D('',#16456,#13093,#13094);
#11571=AXIS2_PLACEMENT_3D('',#16459,#13095,#13096);
#11572=AXIS2_PLACEMENT_3D('',#16461,#13097,#13098);
#11573=AXIS2_PLACEMENT_3D('',#16463,#13099,#13100);
#11574=AXIS2_PLACEMENT_3D('',#16464,#13101,#13102);
#11575=AXIS2_PLACEMENT_3D('',#16465,#13103,#13104);
#11576=AXIS2_PLACEMENT_3D('',#16468,#13105,#13106);
#11577=AXIS2_PLACEMENT_3D('',#16469,#13107,#13108);
#11578=AXIS2_PLACEMENT_3D('',#16471,#13109,#13110);
#11579=AXIS2_PLACEMENT_3D('',#16472,#13111,#13112);
#11580=AXIS2_PLACEMENT_3D('',#16473,#13113,#13114);
#11581=AXIS2_PLACEMENT_3D('',#16475,#13115,#13116);
#11582=AXIS2_PLACEMENT_3D('',#16477,#13117,#13118);
#11583=AXIS2_PLACEMENT_3D('',#16479,#13119,#13120);
#11584=AXIS2_PLACEMENT_3D('',#16480,#13121,#13122);
#11585=AXIS2_PLACEMENT_3D('',#16481,#13123,#13124);
#11586=AXIS2_PLACEMENT_3D('',#16483,#13125,#13126);
#11587=AXIS2_PLACEMENT_3D('',#16485,#13127,#13128);
#11588=AXIS2_PLACEMENT_3D('',#16487,#13129,#13130);
#11589=AXIS2_PLACEMENT_3D('',#16488,#13131,#13132);
#11590=AXIS2_PLACEMENT_3D('',#16489,#13133,#13134);
#11591=AXIS2_PLACEMENT_3D('',#16491,#13135,#13136);
#11592=AXIS2_PLACEMENT_3D('',#16493,#13137,#13138);
#11593=AXIS2_PLACEMENT_3D('',#16495,#13139,#13140);
#11594=AXIS2_PLACEMENT_3D('',#16496,#13141,#13142);
#11595=AXIS2_PLACEMENT_3D('',#16497,#13143,#13144);
#11596=AXIS2_PLACEMENT_3D('',#16500,#13145,#13146);
#11597=AXIS2_PLACEMENT_3D('',#16502,#13147,#13148);
#11598=AXIS2_PLACEMENT_3D('',#16504,#13149,#13150);
#11599=AXIS2_PLACEMENT_3D('',#16505,#13151,#13152);
#11600=AXIS2_PLACEMENT_3D('',#16506,#13153,#13154);
#11601=AXIS2_PLACEMENT_3D('',#16509,#13155,#13156);
#11602=AXIS2_PLACEMENT_3D('',#16511,#13157,#13158);
#11603=AXIS2_PLACEMENT_3D('',#16513,#13159,#13160);
#11604=AXIS2_PLACEMENT_3D('',#16514,#13161,#13162);
#11605=AXIS2_PLACEMENT_3D('',#16515,#13163,#13164);
#11606=AXIS2_PLACEMENT_3D('',#16518,#13165,#13166);
#11607=AXIS2_PLACEMENT_3D('',#16520,#13167,#13168);
#11608=AXIS2_PLACEMENT_3D('',#16522,#13169,#13170);
#11609=AXIS2_PLACEMENT_3D('',#16523,#13171,#13172);
#11610=AXIS2_PLACEMENT_3D('',#16524,#13173,#13174);
#11611=AXIS2_PLACEMENT_3D('',#16527,#13175,#13176);
#11612=AXIS2_PLACEMENT_3D('',#16529,#13177,#13178);
#11613=AXIS2_PLACEMENT_3D('',#16531,#13179,#13180);
#11614=AXIS2_PLACEMENT_3D('',#16532,#13181,#13182);
#11615=AXIS2_PLACEMENT_3D('',#16533,#13183,#13184);
#11616=AXIS2_PLACEMENT_3D('',#16535,#13185,#13186);
#11617=AXIS2_PLACEMENT_3D('',#16537,#13187,#13188);
#11618=AXIS2_PLACEMENT_3D('',#16538,#13189,#13190);
#11619=AXIS2_PLACEMENT_3D('',#16539,#13191,#13192);
#11620=AXIS2_PLACEMENT_3D('',#16541,#13193,#13194);
#11621=AXIS2_PLACEMENT_3D('',#16543,#13195,#13196);
#11622=AXIS2_PLACEMENT_3D('',#16544,#13197,#13198);
#11623=AXIS2_PLACEMENT_3D('',#16545,#13199,#13200);
#11624=AXIS2_PLACEMENT_3D('',#16547,#13201,#13202);
#11625=AXIS2_PLACEMENT_3D('',#16549,#13203,#13204);
#11626=AXIS2_PLACEMENT_3D('',#16551,#13205,#13206);
#11627=AXIS2_PLACEMENT_3D('',#16552,#13207,#13208);
#11628=AXIS2_PLACEMENT_3D('',#16553,#13209,#13210);
#11629=AXIS2_PLACEMENT_3D('',#16555,#13211,#13212);
#11630=AXIS2_PLACEMENT_3D('',#16557,#13213,#13214);
#11631=AXIS2_PLACEMENT_3D('',#16558,#13215,#13216);
#11632=AXIS2_PLACEMENT_3D('',#16559,#13217,#13218);
#11633=AXIS2_PLACEMENT_3D('',#16562,#13219,#13220);
#11634=AXIS2_PLACEMENT_3D('',#16564,#13221,#13222);
#11635=AXIS2_PLACEMENT_3D('',#16566,#13223,#13224);
#11636=AXIS2_PLACEMENT_3D('',#16567,#13225,#13226);
#11637=AXIS2_PLACEMENT_3D('',#16568,#13227,#13228);
#11638=AXIS2_PLACEMENT_3D('',#16571,#13229,#13230);
#11639=AXIS2_PLACEMENT_3D('',#16573,#13231,#13232);
#11640=AXIS2_PLACEMENT_3D('',#16575,#13233,#13234);
#11641=AXIS2_PLACEMENT_3D('',#16576,#13235,#13236);
#11642=AXIS2_PLACEMENT_3D('',#16577,#13237,#13238);
#11643=AXIS2_PLACEMENT_3D('',#16580,#13239,#13240);
#11644=AXIS2_PLACEMENT_3D('',#16582,#13241,#13242);
#11645=AXIS2_PLACEMENT_3D('',#16583,#13243,#13244);
#11646=AXIS2_PLACEMENT_3D('',#16584,#13245,#13246);
#11647=AXIS2_PLACEMENT_3D('',#16585,#13247,#13248);
#11648=AXIS2_PLACEMENT_3D('',#16587,#13249,#13250);
#11649=AXIS2_PLACEMENT_3D('',#16589,#13251,#13252);
#11650=AXIS2_PLACEMENT_3D('',#16591,#13253,#13254);
#11651=AXIS2_PLACEMENT_3D('',#16592,#13255,#13256);
#11652=AXIS2_PLACEMENT_3D('',#16593,#13257,#13258);
#11653=AXIS2_PLACEMENT_3D('',#16595,#13259,#13260);
#11654=AXIS2_PLACEMENT_3D('',#16597,#13261,#13262);
#11655=AXIS2_PLACEMENT_3D('',#16599,#13263,#13264);
#11656=AXIS2_PLACEMENT_3D('',#16600,#13265,#13266);
#11657=AXIS2_PLACEMENT_3D('',#16601,#13267,#13268);
#11658=AXIS2_PLACEMENT_3D('',#16603,#13269,#13270);
#11659=AXIS2_PLACEMENT_3D('',#16605,#13271,#13272);
#11660=AXIS2_PLACEMENT_3D('',#16607,#13273,#13274);
#11661=AXIS2_PLACEMENT_3D('',#16608,#13275,#13276);
#11662=AXIS2_PLACEMENT_3D('',#16609,#13277,#13278);
#11663=AXIS2_PLACEMENT_3D('',#16612,#13279,#13280);
#11664=AXIS2_PLACEMENT_3D('',#16614,#13281,#13282);
#11665=AXIS2_PLACEMENT_3D('',#16616,#13283,#13284);
#11666=AXIS2_PLACEMENT_3D('',#16617,#13285,#13286);
#11667=AXIS2_PLACEMENT_3D('',#16618,#13287,#13288);
#11668=AXIS2_PLACEMENT_3D('',#16621,#13289,#13290);
#11669=AXIS2_PLACEMENT_3D('',#16623,#13291,#13292);
#11670=AXIS2_PLACEMENT_3D('',#16625,#13293,#13294);
#11671=AXIS2_PLACEMENT_3D('',#16626,#13295,#13296);
#11672=AXIS2_PLACEMENT_3D('',#16627,#13297,#13298);
#11673=AXIS2_PLACEMENT_3D('',#16630,#13299,#13300);
#11674=AXIS2_PLACEMENT_3D('',#16632,#13301,#13302);
#11675=AXIS2_PLACEMENT_3D('',#16634,#13303,#13304);
#11676=AXIS2_PLACEMENT_3D('',#16635,#13305,#13306);
#11677=AXIS2_PLACEMENT_3D('',#16636,#13307,#13308);
#11678=AXIS2_PLACEMENT_3D('',#16639,#13309,#13310);
#11679=AXIS2_PLACEMENT_3D('',#16641,#13311,#13312);
#11680=AXIS2_PLACEMENT_3D('',#16643,#13313,#13314);
#11681=AXIS2_PLACEMENT_3D('',#16644,#13315,#13316);
#11682=AXIS2_PLACEMENT_3D('',#16645,#13317,#13318);
#11683=AXIS2_PLACEMENT_3D('',#16648,#13319,#13320);
#11684=AXIS2_PLACEMENT_3D('',#16650,#13321,#13322);
#11685=AXIS2_PLACEMENT_3D('',#16652,#13323,#13324);
#11686=AXIS2_PLACEMENT_3D('',#16653,#13325,#13326);
#11687=AXIS2_PLACEMENT_3D('',#16654,#13327,#13328);
#11688=AXIS2_PLACEMENT_3D('',#16657,#13329,#13330);
#11689=AXIS2_PLACEMENT_3D('',#16659,#13331,#13332);
#11690=AXIS2_PLACEMENT_3D('',#16661,#13333,#13334);
#11691=AXIS2_PLACEMENT_3D('',#16662,#13335,#13336);
#11692=AXIS2_PLACEMENT_3D('',#16663,#13337,#13338);
#11693=AXIS2_PLACEMENT_3D('',#16666,#13339,#13340);
#11694=AXIS2_PLACEMENT_3D('',#16670,#13342,#13343);
#11695=AXIS2_PLACEMENT_3D('',#16672,#13345,#13346);
#11696=AXIS2_PLACEMENT_3D('',#16675,#13347,#13348);
#11697=AXIS2_PLACEMENT_3D('',#16679,#13350,#13351);
#11698=AXIS2_PLACEMENT_3D('',#16681,#13353,#13354);
#11699=AXIS2_PLACEMENT_3D('',#16684,#13355,#13356);
#11700=AXIS2_PLACEMENT_3D('',#16688,#13358,#13359);
#11701=AXIS2_PLACEMENT_3D('',#16690,#13361,#13362);
#11702=AXIS2_PLACEMENT_3D('',#16692,#13363,#13364);
#11703=AXIS2_PLACEMENT_3D('',#16694,#13365,#13366);
#11704=AXIS2_PLACEMENT_3D('',#16695,#13367,#13368);
#11705=AXIS2_PLACEMENT_3D('',#16696,#13369,#13370);
#11706=AXIS2_PLACEMENT_3D('',#16699,#13371,#13372);
#11707=AXIS2_PLACEMENT_3D('',#16703,#13374,#13375);
#11708=AXIS2_PLACEMENT_3D('',#16705,#13377,#13378);
#11709=AXIS2_PLACEMENT_3D('',#16708,#13379,#13380);
#11710=AXIS2_PLACEMENT_3D('',#16712,#13382,#13383);
#11711=AXIS2_PLACEMENT_3D('',#16714,#13385,#13386);
#11712=AXIS2_PLACEMENT_3D('',#16717,#13387,#13388);
#11713=AXIS2_PLACEMENT_3D('',#16721,#13390,#13391);
#11714=AXIS2_PLACEMENT_3D('',#16723,#13393,#13394);
#11715=AXIS2_PLACEMENT_3D('',#16726,#13395,#13396);
#11716=AXIS2_PLACEMENT_3D('',#16730,#13398,#13399);
#11717=AXIS2_PLACEMENT_3D('',#16732,#13401,#13402);
#11718=AXIS2_PLACEMENT_3D('',#16735,#13403,#13404);
#11719=AXIS2_PLACEMENT_3D('',#16737,#13405,#13406);
#11720=AXIS2_PLACEMENT_3D('',#16739,#13407,#13408);
#11721=AXIS2_PLACEMENT_3D('',#16740,#13409,#13410);
#11722=AXIS2_PLACEMENT_3D('',#16741,#13411,#13412);
#11723=AXIS2_PLACEMENT_3D('',#16744,#13413,#13414);
#11724=AXIS2_PLACEMENT_3D('',#16746,#13415,#13416);
#11725=AXIS2_PLACEMENT_3D('',#16748,#13417,#13418);
#11726=AXIS2_PLACEMENT_3D('',#16749,#13419,#13420);
#11727=AXIS2_PLACEMENT_3D('',#16750,#13421,#13422);
#11728=AXIS2_PLACEMENT_3D('',#16753,#13423,#13424);
#11729=AXIS2_PLACEMENT_3D('',#16755,#13425,#13426);
#11730=AXIS2_PLACEMENT_3D('',#16757,#13427,#13428);
#11731=AXIS2_PLACEMENT_3D('',#16758,#13429,#13430);
#11732=AXIS2_PLACEMENT_3D('',#16759,#13431,#13432);
#11733=AXIS2_PLACEMENT_3D('',#16762,#13433,#13434);
#11734=AXIS2_PLACEMENT_3D('',#16766,#13436,#13437);
#11735=AXIS2_PLACEMENT_3D('',#16768,#13439,#13440);
#11736=AXIS2_PLACEMENT_3D('',#16770,#13441,#13442);
#11737=AXIS2_PLACEMENT_3D('',#16773,#13444,#13445);
#11738=AXIS2_PLACEMENT_3D('',#16775,#13447,#13448);
#11739=AXIS2_PLACEMENT_3D('',#16777,#13450,#13451);
#11740=AXIS2_PLACEMENT_3D('',#16779,#13453,#13454);
#11741=AXIS2_PLACEMENT_3D('',#16783,#13456,#13457);
#11742=AXIS2_PLACEMENT_3D('',#16785,#13459,#13460);
#11743=AXIS2_PLACEMENT_3D('',#16788,#13461,#13462);
#11744=AXIS2_PLACEMENT_3D('',#16792,#13464,#13465);
#11745=AXIS2_PLACEMENT_3D('',#16794,#13467,#13468);
#11746=AXIS2_PLACEMENT_3D('',#16796,#13469,#13470);
#11747=AXIS2_PLACEMENT_3D('',#16799,#13472,#13473);
#11748=AXIS2_PLACEMENT_3D('',#16801,#13475,#13476);
#11749=AXIS2_PLACEMENT_3D('',#16803,#13478,#13479);
#11750=AXIS2_PLACEMENT_3D('',#16805,#13481,#13482);
#11751=AXIS2_PLACEMENT_3D('',#16816,#13483,#13484);
#11752=AXIS2_PLACEMENT_3D('',#16840,#13485,#13486);
#11753=AXIS2_PLACEMENT_3D('',#16849,#13487,#13488);
#11754=AXIS2_PLACEMENT_3D('',#16853,#13490,#13491);
#11755=AXIS2_PLACEMENT_3D('',#16855,#13493,#13494);
#11756=AXIS2_PLACEMENT_3D('',#16858,#13495,#13496);
#11757=AXIS2_PLACEMENT_3D('',#16862,#13498,#13499);
#11758=AXIS2_PLACEMENT_3D('',#16864,#13501,#13502);
#11759=AXIS2_PLACEMENT_3D('',#16867,#13505,#13506);
#11760=AXIS2_PLACEMENT_3D('',#16869,#13508,#13509);
#11761=AXIS2_PLACEMENT_3D('',#16871,#13511,#13512);
#11762=AXIS2_PLACEMENT_3D('',#16874,#13513,#13514);
#11763=AXIS2_PLACEMENT_3D('',#16885,#13515,#13516);
#11764=AXIS2_PLACEMENT_3D('',#16909,#13517,#13518);
#11765=AXIS2_PLACEMENT_3D('',#16918,#13519,#13520);
#11766=AXIS2_PLACEMENT_3D('',#16921,#13521,#13522);
#11767=AXIS2_PLACEMENT_3D('',#16924,#13525,#13526);
#11768=AXIS2_PLACEMENT_3D('',#16927,#13529,#13530);
#11769=AXIS2_PLACEMENT_3D('',#16930,#13533,#13534);
#11770=AXIS2_PLACEMENT_3D('',#16933,#13535,#13536);
#11771=AXIS2_PLACEMENT_3D('',#16935,#13537,#13538);
#11772=AXIS2_PLACEMENT_3D('',#16937,#13539,#13540);
#11773=AXIS2_PLACEMENT_3D('',#16939,#13541,#13542);
#11774=AXIS2_PLACEMENT_3D('',#16941,#13543,#13544);
#11775=AXIS2_PLACEMENT_3D('',#16943,#13545,#13546);
#11776=AXIS2_PLACEMENT_3D('',#16947,#13548,#13549);
#11777=AXIS2_PLACEMENT_3D('',#16949,#13550,#13551);
#11778=AXIS2_PLACEMENT_3D('',#17000,#13553,#13554);
#11779=AXIS2_PLACEMENT_3D('',#17036,#13556,#13557);
#11780=AXIS2_PLACEMENT_3D('',#17074,#13559,#13560);
#11781=AXIS2_PLACEMENT_3D('',#17120,#13561,#13562);
#11782=AXIS2_PLACEMENT_3D('',#17122,#13563,#13564);
#11783=AXIS2_PLACEMENT_3D('',#17124,#13565,#13566);
#11784=AXIS2_PLACEMENT_3D('',#17126,#13567,#13568);
#11785=AXIS2_PLACEMENT_3D('',#17176,#13570,#13571);
#11786=AXIS2_PLACEMENT_3D('',#17210,#13572,#13573);
#11787=AXIS2_PLACEMENT_3D('',#17249,#13575,#13576);
#11788=AXIS2_PLACEMENT_3D('',#17297,#13578,#13579);
#11789=AXIS2_PLACEMENT_3D('',#17299,#13580,#13581);
#11790=AXIS2_PLACEMENT_3D('',#17301,#13582,#13583);
#11791=AXIS2_PLACEMENT_3D('',#17303,#13584,#13585);
#11792=AXIS2_PLACEMENT_3D('',#17354,#13587,#13588);
#11793=AXIS2_PLACEMENT_3D('',#17390,#13590,#13591);
#11794=AXIS2_PLACEMENT_3D('',#17426,#13592,#13593);
#11795=AXIS2_PLACEMENT_3D('',#17474,#13595,#13596);
#11796=AXIS2_PLACEMENT_3D('',#17476,#13597,#13598);
#11797=AXIS2_PLACEMENT_3D('',#17478,#13599,#13600);
#11798=AXIS2_PLACEMENT_3D('',#17480,#13601,#13602);
#11799=AXIS2_PLACEMENT_3D('',#17528,#13603,#13604);
#11800=AXIS2_PLACEMENT_3D('',#17564,#13606,#13607);
#11801=AXIS2_PLACEMENT_3D('',#17603,#13609,#13610);
#11802=AXIS2_PLACEMENT_3D('',#17651,#13612,#13613);
#11803=AXIS2_PLACEMENT_3D('',#17652,#13614,#13615);
#11804=AXIS2_PLACEMENT_3D('',#17654,#13616,#13617);
#11805=AXIS2_PLACEMENT_3D('',#17656,#13618,#13619);
#11806=AXIS2_PLACEMENT_3D('',#17658,#13620,#13621);
#11807=AXIS2_PLACEMENT_3D('',#17660,#13622,#13623);
#11808=AXIS2_PLACEMENT_3D('',#17662,#13624,#13625);
#11809=AXIS2_PLACEMENT_3D('',#17663,#13626,#13627);
#11810=AXIS2_PLACEMENT_3D('',#17664,#13628,#13629);
#11811=AXIS2_PLACEMENT_3D('',#17666,#13631,#13632);
#11812=AXIS2_PLACEMENT_3D('',#17668,#13634,#13635);
#11813=AXIS2_PLACEMENT_3D('',#17671,#13636,#13637);
#11814=AXIS2_PLACEMENT_3D('',#17682,#13638,#13639);
#11815=AXIS2_PLACEMENT_3D('',#17706,#13640,#13641);
#11816=AXIS2_PLACEMENT_3D('',#17715,#13642,#13643);
#11817=AXIS2_PLACEMENT_3D('',#17718,#13644,#13645);
#11818=AXIS2_PLACEMENT_3D('',#17721,#13648,#13649);
#11819=AXIS2_PLACEMENT_3D('',#17724,#13650,#13651);
#11820=AXIS2_PLACEMENT_3D('',#17728,#13653,#13654);
#11821=AXIS2_PLACEMENT_3D('',#17730,#13656,#13657);
#11822=AXIS2_PLACEMENT_3D('',#17740,#13662,#13663);
#11823=AXIS2_PLACEMENT_3D('',#17742,#13664,#13665);
#11824=AXIS2_PLACEMENT_3D('',#17746,#13667,#13668);
#11825=AXIS2_PLACEMENT_3D('',#17748,#13669,#13670);
#11826=AXIS2_PLACEMENT_3D('',#17750,#13671,#13672);
#11827=AXIS2_PLACEMENT_3D('',#17760,#13677,#13678);
#11828=AXIS2_PLACEMENT_3D('',#17764,#13680,#13681);
#11829=AXIS2_PLACEMENT_3D('',#17768,#13683,#13684);
#11830=AXIS2_PLACEMENT_3D('',#17771,#13686,#13687);
#11831=AXIS2_PLACEMENT_3D('',#17774,#13688,#13689);
#11832=AXIS2_PLACEMENT_3D('',#17776,#13690,#13691);
#11833=AXIS2_PLACEMENT_3D('',#17780,#13693,#13694);
#11834=AXIS2_PLACEMENT_3D('',#17781,#13695,#13696);
#11835=AXIS2_PLACEMENT_3D('',#17784,#13698,#13699);
#11836=AXIS2_PLACEMENT_3D('',#17786,#13700,#13701);
#11837=AXIS2_PLACEMENT_3D('',#17788,#13702,#13703);
#11838=AXIS2_PLACEMENT_3D('',#17791,#13705,#13706);
#11839=AXIS2_PLACEMENT_3D('',#17793,#13707,#13708);
#11840=AXIS2_PLACEMENT_3D('',#17796,#13710,#13711);
#11841=AXIS2_PLACEMENT_3D('',#17799,#13713,#13714);
#11842=AXIS2_PLACEMENT_3D('',#17801,#13715,#13716);
#11843=AXIS2_PLACEMENT_3D('',#17804,#13718,#13719);
#11844=AXIS2_PLACEMENT_3D('',#17816,#13720,#13721);
#11845=AXIS2_PLACEMENT_3D('',#17849,#13723,#13724);
#11846=AXIS2_PLACEMENT_3D('',#17893,#13726,#13727);
#11847=AXIS2_PLACEMENT_3D('',#17926,#13729,#13730);
#11848=AXIS2_PLACEMENT_3D('',#17948,#13732,#13733);
#11849=AXIS2_PLACEMENT_3D('',#17957,#13738,#13739);
#11850=AXIS2_PLACEMENT_3D('',#17966,#13744,#13745);
#11851=AXIS2_PLACEMENT_3D('',#17983,#13753,#13754);
#11852=AXIS2_PLACEMENT_3D('',#17987,#13756,#13757);
#11853=AXIS2_PLACEMENT_3D('',#17991,#13759,#13760);
#11854=AXIS2_PLACEMENT_3D('',#17995,#13762,#13763);
#11855=AXIS2_PLACEMENT_3D('',#18003,#13768,#13769);
#11856=AXIS2_PLACEMENT_3D('',#18010,#13772,#13773);
#11857=AXIS2_PLACEMENT_3D('',#18014,#13775,#13776);
#11858=AXIS2_PLACEMENT_3D('',#18019,#13779,#13780);
#11859=AXIS2_PLACEMENT_3D('',#18033,#13788,#13789);
#11860=AXIS2_PLACEMENT_3D('',#18040,#13794,#13795);
#11861=AXIS2_PLACEMENT_3D('',#18041,#13796,#13797);
#11862=AXIS2_PLACEMENT_3D('',#18042,#13798,#13799);
#11863=AXIS2_PLACEMENT_3D('',#18043,#13800,#13801);
#11864=AXIS2_PLACEMENT_3D('',#18044,#13802,#13803);
#11865=AXIS2_PLACEMENT_3D('',#18045,#13804,#13805);
#11866=AXIS2_PLACEMENT_3D('',#18046,#13806,#13807);
#11867=AXIS2_PLACEMENT_3D('',#18050,#13809,#13810);
#11868=AXIS2_PLACEMENT_3D('',#18051,#13811,#13812);
#11869=AXIS2_PLACEMENT_3D('',#18052,#13813,#13814);
#11870=AXIS2_PLACEMENT_3D('',#18053,#13815,#13816);
#11871=AXIS2_PLACEMENT_3D('',#18054,#13817,#13818);
#11872=AXIS2_PLACEMENT_3D('',#18055,#13819,#13820);
#11873=AXIS2_PLACEMENT_3D('',#18056,#13821,#13822);
#11874=AXIS2_PLACEMENT_3D('',#18057,#13823,#13824);
#11875=AXIS2_PLACEMENT_3D('',#18059,#13825,#13826);
#11876=AXIS2_PLACEMENT_3D('',#18061,#13828,#13829);
#11877=AXIS2_PLACEMENT_3D('',#18070,#13834,#13835);
#11878=AXIS2_PLACEMENT_3D('',#18072,#13836,#13837);
#11879=AXIS2_PLACEMENT_3D('',#18075,#13839,#13840);
#11880=AXIS2_PLACEMENT_3D('',#18076,#13841,#13842);
#11881=AXIS2_PLACEMENT_3D('',#18078,#13843,#13844);
#11882=AXIS2_PLACEMENT_3D('',#18080,#13845,#13846);
#11883=AXIS2_PLACEMENT_3D('',#18082,#13848,#13849);
#11884=AXIS2_PLACEMENT_3D('',#18087,#13851,#13852);
#11885=AXIS2_PLACEMENT_3D('',#18089,#13853,#13854);
#11886=AXIS2_PLACEMENT_3D('',#18093,#13857,#13858);
#11887=AXIS2_PLACEMENT_3D('',#18096,#13859,#13860);
#11888=AXIS2_PLACEMENT_3D('',#18098,#13861,#13862);
#11889=AXIS2_PLACEMENT_3D('',#18170,#13864,#13865);
#11890=AXIS2_PLACEMENT_3D('',#18173,#13866,#13867);
#11891=AXIS2_PLACEMENT_3D('',#18175,#13868,#13869);
#11892=AXIS2_PLACEMENT_3D('',#18247,#13871,#13872);
#11893=AXIS2_PLACEMENT_3D('',#18250,#13873,#13874);
#11894=AXIS2_PLACEMENT_3D('',#18252,#13875,#13876);
#11895=AXIS2_PLACEMENT_3D('',#18324,#13878,#13879);
#11896=AXIS2_PLACEMENT_3D('',#18327,#13880,#13881);
#11897=AXIS2_PLACEMENT_3D('',#18329,#13882,#13883);
#11898=AXIS2_PLACEMENT_3D('',#18401,#13885,#13886);
#11899=AXIS2_PLACEMENT_3D('',#18404,#13887,#13888);
#11900=AXIS2_PLACEMENT_3D('',#18456,#13889,#13890);
#11901=AXIS2_PLACEMENT_3D('',#18458,#13891,#13892);
#11902=AXIS2_PLACEMENT_3D('',#18469,#13893,#13894);
#11903=AXIS2_PLACEMENT_3D('',#18470,#13895,#13896);
#11904=AXIS2_PLACEMENT_3D('',#18471,#13897,#13898);
#11905=AXIS2_PLACEMENT_3D('',#18477,#13901,#13902);
#11906=AXIS2_PLACEMENT_3D('',#18479,#13903,#13904);
#11907=AXIS2_PLACEMENT_3D('',#18483,#13906,#13907);
#11908=AXIS2_PLACEMENT_3D('',#18487,#13909,#13910);
#11909=AXIS2_PLACEMENT_3D('',#18489,#13911,#13912);
#11910=AXIS2_PLACEMENT_3D('',#18493,#13914,#13915);
#11911=AXIS2_PLACEMENT_3D('',#18497,#13917,#13918);
#11912=AXIS2_PLACEMENT_3D('',#18499,#13919,#13920);
#11913=AXIS2_PLACEMENT_3D('',#18503,#13922,#13923);
#11914=AXIS2_PLACEMENT_3D('',#18506,#13925,#13926);
#11915=AXIS2_PLACEMENT_3D('',#18510,#13928,#13929);
#11916=AXIS2_PLACEMENT_3D('',#18517,#13933,#13934);
#11917=AXIS2_PLACEMENT_3D('',#18518,#13935,#13936);
#11918=AXIS2_PLACEMENT_3D('',#18519,#13937,#13938);
#11919=AXIS2_PLACEMENT_3D('',#18562,#13942,#13943);
#11920=AXIS2_PLACEMENT_3D('',#18564,#13945,#13946);
#11921=AXIS2_PLACEMENT_3D('',#18575,#13951,#13952);
#11922=AXIS2_PLACEMENT_3D('',#18606,#13954,#13955);
#11923=AXIS2_PLACEMENT_3D('',#18609,#13956,#13957);
#11924=AXIS2_PLACEMENT_3D('',#18672,#13958,#13959);
#11925=AXIS2_PLACEMENT_3D('',#18674,#13960,#13961);
#11926=AXIS2_PLACEMENT_3D('',#18676,#13962,#13963);
#11927=AXIS2_PLACEMENT_3D('',#18732,#13964,#13965);
#11928=AXIS2_PLACEMENT_3D('',#18744,#13966,#13967);
#11929=AXIS2_PLACEMENT_3D('',#18755,#13968,#13969);
#11930=AXIS2_PLACEMENT_3D('',#18777,#13970,#13971);
#11931=AXIS2_PLACEMENT_3D('',#18778,#13972,#13973);
#11932=AXIS2_PLACEMENT_3D('',#18783,#13975,#13976);
#11933=AXIS2_PLACEMENT_3D('',#18786,#13978,#13979);
#11934=AXIS2_PLACEMENT_3D('',#18787,#13980,#13981);
#11935=AXIS2_PLACEMENT_3D('',#18788,#13982,#13983);
#11936=AXIS2_PLACEMENT_3D('',#18789,#13984,#13985);
#11937=AXIS2_PLACEMENT_3D('',#18790,#13986,#13987);
#11938=AXIS2_PLACEMENT_3D('',#18795,#13989,#13990);
#11939=AXIS2_PLACEMENT_3D('',#18799,#13992,#13993);
#11940=AXIS2_PLACEMENT_3D('',#18829,#13994,#13995);
#11941=AXIS2_PLACEMENT_3D('',#18830,#13996,#13997);
#11942=AXIS2_PLACEMENT_3D('',#18835,#13999,#14000);
#11943=AXIS2_PLACEMENT_3D('',#18839,#14002,#14003);
#11944=AXIS2_PLACEMENT_3D('',#18881,#14004,#14005);
#11945=AXIS2_PLACEMENT_3D('',#18882,#14006,#14007);
#11946=AXIS2_PLACEMENT_3D('',#18887,#14009,#14010);
#11947=AXIS2_PLACEMENT_3D('',#18891,#14012,#14013);
#11948=AXIS2_PLACEMENT_3D('',#18895,#14016,#14017);
#11949=AXIS2_PLACEMENT_3D('',#18896,#14018,#14019);
#11950=AXIS2_PLACEMENT_3D('',#18901,#14021,#14022);
#11951=AXIS2_PLACEMENT_3D('',#18905,#14024,#14025);
#11952=AXIS2_PLACEMENT_3D('',#18909,#14027,#14028);
#11953=AXIS2_PLACEMENT_3D('',#18912,#14030,#14031);
#11954=AXIS2_PLACEMENT_3D('',#18913,#14032,#14033);
#11955=AXIS2_PLACEMENT_3D('',#19026,#14039,#14040);
#11956=AXIS2_PLACEMENT_3D('',#19154,#14046,#14047);
#11957=AXIS2_PLACEMENT_3D('',#19155,#14048,#14049);
#11958=AXIS2_PLACEMENT_3D('',#19156,#14050,#14051);
#11959=AXIS2_PLACEMENT_3D('',#19157,#14052,#14053);
#11960=AXIS2_PLACEMENT_3D('',#19231,#14059,#14060);
#11961=AXIS2_PLACEMENT_3D('',#19290,#14066,#14067);
#11962=AXIS2_PLACEMENT_3D('',#19361,#14074,#14075);
#11963=AXIS2_PLACEMENT_3D('',#19394,#14077,#14078);
#11964=AXIS2_PLACEMENT_3D('',#19454,#14080,#14081);
#11965=AXIS2_PLACEMENT_3D('',#19455,#14082,#14083);
#11966=AXIS2_PLACEMENT_3D('',#19468,#14090,#14091);
#11967=AXIS2_PLACEMENT_3D('',#19472,#14093,#14094);
#11968=AXIS2_PLACEMENT_3D('',#19476,#14096,#14097);
#11969=AXIS2_PLACEMENT_3D('',#19479,#14099,#14100);
#11970=AXIS2_PLACEMENT_3D('',#19482,#14101,#14102);
#11971=AXIS2_PLACEMENT_3D('',#19542,#14104,#14105);
#11972=AXIS2_PLACEMENT_3D('',#19544,#14106,#14107);
#11973=AXIS2_PLACEMENT_3D('',#19604,#14109,#14110);
#11974=AXIS2_PLACEMENT_3D('',#19640,#14112,#14113);
#11975=AXIS2_PLACEMENT_3D('',#19699,#14115,#14116);
#11976=AXIS2_PLACEMENT_3D('',#19759,#14118,#14119);
#11977=AXIS2_PLACEMENT_3D('',#19795,#14121,#14122);
#11978=AXIS2_PLACEMENT_3D('',#19797,#14123,#14124);
#11979=AXIS2_PLACEMENT_3D('',#19857,#14126,#14127);
#11980=AXIS2_PLACEMENT_3D('',#19893,#14129,#14130);
#11981=AXIS2_PLACEMENT_3D('',#19951,#14132,#14133);
#11982=AXIS2_PLACEMENT_3D('',#19952,#14134,#14135);
#11983=AXIS2_PLACEMENT_3D('',#19953,#14136,#14137);
#11984=AXIS2_PLACEMENT_3D('',#19954,#14138,#14139);
#11985=AXIS2_PLACEMENT_3D('',#19966,#14140,#14141);
#11986=AXIS2_PLACEMENT_3D('',#19976,#14142,#14143);
#11987=AXIS2_PLACEMENT_3D('',#19977,#14144,#14145);
#11988=AXIS2_PLACEMENT_3D('',#19980,#14146,#14147);
#11989=AXIS2_PLACEMENT_3D('',#20053,#14149,#14150);
#11990=AXIS2_PLACEMENT_3D('',#20054,#14151,#14152);
#11991=AXIS2_PLACEMENT_3D('',#20057,#14153,#14154);
#11992=AXIS2_PLACEMENT_3D('',#20130,#14156,#14157);
#11993=AXIS2_PLACEMENT_3D('',#20131,#14158,#14159);
#11994=AXIS2_PLACEMENT_3D('',#20143,#14163,#14164);
#11995=AXIS2_PLACEMENT_3D('',#20158,#14169,#14170);
#11996=AXIS2_PLACEMENT_3D('',#20163,#14172,#14173);
#11997=AXIS2_PLACEMENT_3D('',#20166,#14175,#14176);
#11998=AXIS2_PLACEMENT_3D('',#20167,#14177,#14178);
#11999=AXIS2_PLACEMENT_3D('',#20172,#14180,#14181);
#12000=AXIS2_PLACEMENT_3D('',#20175,#14183,#14184);
#12001=AXIS2_PLACEMENT_3D('',#20176,#14185,#14186);
#12002=AXIS2_PLACEMENT_3D('',#20189,#14189,#14190);
#12003=AXIS2_PLACEMENT_3D('',#20194,#14192,#14193);
#12004=AXIS2_PLACEMENT_3D('',#20197,#14195,#14196);
#12005=AXIS2_PLACEMENT_3D('',#20198,#14197,#14198);
#12006=AXIS2_PLACEMENT_3D('',#20208,#14201,#14202);
#12007=AXIS2_PLACEMENT_3D('',#20210,#14203,#14204);
#12008=AXIS2_PLACEMENT_3D('',#20213,#14206,#14207);
#12009=AXIS2_PLACEMENT_3D('',#20214,#14208,#14209);
#12010=AXIS2_PLACEMENT_3D('',#20220,#14213,#14214);
#12011=AXIS2_PLACEMENT_3D('',#20229,#14219,#14220);
#12012=AXIS2_PLACEMENT_3D('',#20231,#14221,#14222);
#12013=AXIS2_PLACEMENT_3D('',#20234,#14224,#14225);
#12014=AXIS2_PLACEMENT_3D('',#20236,#14226,#14227);
#12015=AXIS2_PLACEMENT_3D('',#20239,#14229,#14230);
#12016=AXIS2_PLACEMENT_3D('',#20240,#14231,#14232);
#12017=AXIS2_PLACEMENT_3D('',#20241,#14233,#14234);
#12018=AXIS2_PLACEMENT_3D('',#20242,#14235,#14236);
#12019=AXIS2_PLACEMENT_3D('',#20243,#14237,#14238);
#12020=AXIS2_PLACEMENT_3D('',#20244,#14239,#14240);
#12021=AXIS2_PLACEMENT_3D('',#20245,#14241,#14242);
#12022=AXIS2_PLACEMENT_3D('',#20246,#14243,#14244);
#12023=AXIS2_PLACEMENT_3D('',#20247,#14245,#14246);
#12024=AXIS2_PLACEMENT_3D('',#20248,#14247,#14248);
#12025=AXIS2_PLACEMENT_3D('',#20249,#14249,#14250);
#12026=AXIS2_PLACEMENT_3D('',#20252,#14251,#14252);
#12027=AXIS2_PLACEMENT_3D('',#20304,#14253,#14254);
#12028=AXIS2_PLACEMENT_3D('',#20306,#14255,#14256);
#12029=AXIS2_PLACEMENT_3D('',#20317,#14257,#14258);
#12030=AXIS2_PLACEMENT_3D('',#20318,#14259,#14260);
#12031=AXIS2_PLACEMENT_3D('',#20319,#14261,#14262);
#12032=AXIS2_PLACEMENT_3D('',#20364,#14267,#14268);
#12033=AXIS2_PLACEMENT_3D('',#20366,#14270,#14271);
#12034=AXIS2_PLACEMENT_3D('',#20374,#14275,#14276);
#12035=AXIS2_PLACEMENT_3D('',#20405,#14278,#14279);
#12036=AXIS2_PLACEMENT_3D('',#20408,#14280,#14281);
#12037=AXIS2_PLACEMENT_3D('',#20471,#14282,#14283);
#12038=AXIS2_PLACEMENT_3D('',#20473,#14284,#14285);
#12039=AXIS2_PLACEMENT_3D('',#20475,#14286,#14287);
#12040=AXIS2_PLACEMENT_3D('',#20531,#14288,#14289);
#12041=AXIS2_PLACEMENT_3D('',#20536,#14291,#14292);
#12042=AXIS2_PLACEMENT_3D('',#20539,#14294,#14295);
#12043=AXIS2_PLACEMENT_3D('',#20540,#14296,#14297);
#12044=AXIS2_PLACEMENT_3D('',#20545,#14299,#14300);
#12045=AXIS2_PLACEMENT_3D('',#20549,#14302,#14303);
#12046=AXIS2_PLACEMENT_3D('',#20591,#14304,#14305);
#12047=AXIS2_PLACEMENT_3D('',#20592,#14306,#14307);
#12048=AXIS2_PLACEMENT_3D('',#20597,#14309,#14310);
#12049=AXIS2_PLACEMENT_3D('',#20601,#14312,#14313);
#12050=AXIS2_PLACEMENT_3D('',#20605,#14316,#14317);
#12051=AXIS2_PLACEMENT_3D('',#20606,#14318,#14319);
#12052=AXIS2_PLACEMENT_3D('',#20611,#14321,#14322);
#12053=AXIS2_PLACEMENT_3D('',#20615,#14324,#14325);
#12054=AXIS2_PLACEMENT_3D('',#20619,#14327,#14328);
#12055=AXIS2_PLACEMENT_3D('',#20622,#14330,#14331);
#12056=AXIS2_PLACEMENT_3D('',#20623,#14332,#14333);
#12057=AXIS2_PLACEMENT_3D('',#20736,#14339,#14340);
#12058=AXIS2_PLACEMENT_3D('',#20737,#14341,#14342);
#12059=AXIS2_PLACEMENT_3D('',#20738,#14343,#14344);
#12060=AXIS2_PLACEMENT_3D('',#20739,#14345,#14346);
#12061=AXIS2_PLACEMENT_3D('',#20813,#14352,#14353);
#12062=AXIS2_PLACEMENT_3D('',#20814,#14354,#14355);
#12063=AXIS2_PLACEMENT_3D('',#20815,#14356,#14357);
#12064=AXIS2_PLACEMENT_3D('',#20816,#14358,#14359);
#12065=AXIS2_PLACEMENT_3D('',#20828,#14360,#14361);
#12066=AXIS2_PLACEMENT_3D('',#20838,#14362,#14363);
#12067=AXIS2_PLACEMENT_3D('',#20839,#14364,#14365);
#12068=AXIS2_PLACEMENT_3D('',#20842,#14366,#14367);
#12069=AXIS2_PLACEMENT_3D('',#20915,#14369,#14370);
#12070=AXIS2_PLACEMENT_3D('',#20916,#14371,#14372);
#12071=AXIS2_PLACEMENT_3D('',#20931,#14377,#14378);
#12072=AXIS2_PLACEMENT_3D('',#20943,#14382,#14383);
#12073=AXIS2_PLACEMENT_3D('',#20946,#14385,#14386);
#12074=AXIS2_PLACEMENT_3D('',#20947,#14387,#14388);
#12075=AXIS2_PLACEMENT_3D('',#20948,#14389,#14390);
#12076=AXIS2_PLACEMENT_3D('',#20953,#14392,#14393);
#12077=AXIS2_PLACEMENT_3D('',#20956,#14395,#14396);
#12078=AXIS2_PLACEMENT_3D('',#20957,#14397,#14398);
#12079=AXIS2_PLACEMENT_3D('',#20970,#14401,#14402);
#12080=AXIS2_PLACEMENT_3D('',#20975,#14404,#14405);
#12081=AXIS2_PLACEMENT_3D('',#20978,#14407,#14408);
#12082=AXIS2_PLACEMENT_3D('',#20979,#14409,#14410);
#12083=AXIS2_PLACEMENT_3D('',#20989,#14413,#14414);
#12084=AXIS2_PLACEMENT_3D('',#20990,#14415,#14416);
#12085=AXIS2_PLACEMENT_3D('',#20992,#14418,#14419);
#12086=AXIS2_PLACEMENT_3D('',#20993,#14420,#14421);
#12087=AXIS2_PLACEMENT_3D('',#20999,#14425,#14426);
#12088=AXIS2_PLACEMENT_3D('',#21006,#14431,#14432);
#12089=AXIS2_PLACEMENT_3D('',#21008,#14433,#14434);
#12090=AXIS2_PLACEMENT_3D('',#21012,#14436,#14437);
#12091=AXIS2_PLACEMENT_3D('',#21013,#14438,#14439);
#12092=AXIS2_PLACEMENT_3D('',#21016,#14441,#14442);
#12093=AXIS2_PLACEMENT_3D('',#21017,#14443,#14444);
#12094=AXIS2_PLACEMENT_3D('',#21018,#14445,#14446);
#12095=AXIS2_PLACEMENT_3D('',#21019,#14447,#14448);
#12096=AXIS2_PLACEMENT_3D('',#21020,#14449,#14450);
#12097=AXIS2_PLACEMENT_3D('',#21021,#14451,#14452);
#12098=AXIS2_PLACEMENT_3D('',#21022,#14453,#14454);
#12099=AXIS2_PLACEMENT_3D('',#21023,#14455,#14456);
#12100=AXIS2_PLACEMENT_3D('',#21024,#14457,#14458);
#12101=AXIS2_PLACEMENT_3D('',#21027,#14459,#14460);
#12102=AXIS2_PLACEMENT_3D('',#21079,#14461,#14462);
#12103=AXIS2_PLACEMENT_3D('',#21081,#14463,#14464);
#12104=AXIS2_PLACEMENT_3D('',#21092,#14465,#14466);
#12105=AXIS2_PLACEMENT_3D('',#21093,#14467,#14468);
#12106=AXIS2_PLACEMENT_3D('',#21094,#14469,#14470);
#12107=AXIS2_PLACEMENT_3D('',#21141,#14476,#14477);
#12108=AXIS2_PLACEMENT_3D('',#21142,#14478,#14479);
#12109=AXIS2_PLACEMENT_3D('',#21153,#14484,#14485);
#12110=AXIS2_PLACEMENT_3D('',#21184,#14487,#14488);
#12111=AXIS2_PLACEMENT_3D('',#21187,#14489,#14490);
#12112=AXIS2_PLACEMENT_3D('',#21250,#14491,#14492);
#12113=AXIS2_PLACEMENT_3D('',#21252,#14493,#14494);
#12114=AXIS2_PLACEMENT_3D('',#21254,#14495,#14496);
#12115=AXIS2_PLACEMENT_3D('',#21310,#14497,#14498);
#12116=AXIS2_PLACEMENT_3D('',#21313,#14501,#14502);
#12117=AXIS2_PLACEMENT_3D('',#21319,#14505,#14506);
#12118=AXIS2_PLACEMENT_3D('',#21361,#14507,#14508);
#12119=AXIS2_PLACEMENT_3D('',#21362,#14509,#14510);
#12120=AXIS2_PLACEMENT_3D('',#21475,#14516,#14517);
#12121=AXIS2_PLACEMENT_3D('',#21476,#14518,#14519);
#12122=AXIS2_PLACEMENT_3D('',#21477,#14520,#14521);
#12123=AXIS2_PLACEMENT_3D('',#21478,#14522,#14523);
#12124=AXIS2_PLACEMENT_3D('',#21552,#14529,#14530);
#12125=AXIS2_PLACEMENT_3D('',#21553,#14531,#14532);
#12126=AXIS2_PLACEMENT_3D('',#21554,#14533,#14534);
#12127=AXIS2_PLACEMENT_3D('',#21555,#14535,#14536);
#12128=AXIS2_PLACEMENT_3D('',#21567,#14537,#14538);
#12129=AXIS2_PLACEMENT_3D('',#21577,#14539,#14540);
#12130=AXIS2_PLACEMENT_3D('',#21578,#14541,#14542);
#12131=AXIS2_PLACEMENT_3D('',#21581,#14543,#14544);
#12132=AXIS2_PLACEMENT_3D('',#21654,#14546,#14547);
#12133=AXIS2_PLACEMENT_3D('',#21655,#14548,#14549);
#12134=AXIS2_PLACEMENT_3D('',#21670,#14554,#14555);
#12135=AXIS2_PLACEMENT_3D('',#21685,#14560,#14561);
#12136=AXIS2_PLACEMENT_3D('',#21689,#14563,#14564);
#12137=AXIS2_PLACEMENT_3D('',#21690,#14565,#14566);
#12138=AXIS2_PLACEMENT_3D('',#21691,#14567,#14568);
#12139=AXIS2_PLACEMENT_3D('',#21696,#14570,#14571);
#12140=AXIS2_PLACEMENT_3D('',#21699,#14573,#14574);
#12141=AXIS2_PLACEMENT_3D('',#21700,#14575,#14576);
#12142=AXIS2_PLACEMENT_3D('',#21713,#14579,#14580);
#12143=AXIS2_PLACEMENT_3D('',#21718,#14582,#14583);
#12144=AXIS2_PLACEMENT_3D('',#21721,#14585,#14586);
#12145=AXIS2_PLACEMENT_3D('',#21722,#14587,#14588);
#12146=AXIS2_PLACEMENT_3D('',#21729,#14590,#14591);
#12147=AXIS2_PLACEMENT_3D('',#21731,#14592,#14593);
#12148=AXIS2_PLACEMENT_3D('',#21734,#14595,#14596);
#12149=AXIS2_PLACEMENT_3D('',#21735,#14597,#14598);
#12150=AXIS2_PLACEMENT_3D('',#21741,#14602,#14603);
#12151=AXIS2_PLACEMENT_3D('',#21750,#14608,#14609);
#12152=AXIS2_PLACEMENT_3D('',#21757,#14612,#14613);
#12153=AXIS2_PLACEMENT_3D('',#21759,#14614,#14615);
#12154=AXIS2_PLACEMENT_3D('',#21761,#14616,#14617);
#12155=AXIS2_PLACEMENT_3D('',#21765,#14619,#14620);
#12156=AXIS2_PLACEMENT_3D('',#21766,#14621,#14622);
#12157=AXIS2_PLACEMENT_3D('',#21770,#14625,#14626);
#12158=AXIS2_PLACEMENT_3D('',#21771,#14627,#14628);
#12159=AXIS2_PLACEMENT_3D('',#21772,#14629,#14630);
#12160=AXIS2_PLACEMENT_3D('',#21773,#14631,#14632);
#12161=AXIS2_PLACEMENT_3D('',#21774,#14633,#14634);
#12162=AXIS2_PLACEMENT_3D('',#21775,#14635,#14636);
#12163=AXIS2_PLACEMENT_3D('',#21776,#14637,#14638);
#12164=AXIS2_PLACEMENT_3D('',#21777,#14639,#14640);
#12165=AXIS2_PLACEMENT_3D('',#21780,#14641,#14642);
#12166=AXIS2_PLACEMENT_3D('',#21832,#14643,#14644);
#12167=AXIS2_PLACEMENT_3D('',#21834,#14645,#14646);
#12168=AXIS2_PLACEMENT_3D('',#21845,#14647,#14648);
#12169=AXIS2_PLACEMENT_3D('',#21846,#14649,#14650);
#12170=AXIS2_PLACEMENT_3D('',#21847,#14651,#14652);
#12171=AXIS2_PLACEMENT_3D('',#21890,#14656,#14657);
#12172=AXIS2_PLACEMENT_3D('',#21892,#14659,#14660);
#12173=AXIS2_PLACEMENT_3D('',#21900,#14664,#14665);
#12174=AXIS2_PLACEMENT_3D('',#21931,#14667,#14668);
#12175=AXIS2_PLACEMENT_3D('',#21934,#14669,#14670);
#12176=AXIS2_PLACEMENT_3D('',#21997,#14671,#14672);
#12177=AXIS2_PLACEMENT_3D('',#21999,#14673,#14674);
#12178=AXIS2_PLACEMENT_3D('',#22001,#14675,#14676);
#12179=AXIS2_PLACEMENT_3D('',#22057,#14677,#14678);
#12180=AXIS2_PLACEMENT_3D('',#22062,#14680,#14681);
#12181=AXIS2_PLACEMENT_3D('',#22066,#14683,#14684);
#12182=AXIS2_PLACEMENT_3D('',#22070,#14686,#14687);
#12183=AXIS2_PLACEMENT_3D('',#22073,#14689,#14690);
#12184=AXIS2_PLACEMENT_3D('',#22074,#14691,#14692);
#12185=AXIS2_PLACEMENT_3D('',#22079,#14694,#14695);
#12186=AXIS2_PLACEMENT_3D('',#22083,#14697,#14698);
#12187=AXIS2_PLACEMENT_3D('',#22087,#14701,#14702);
#12188=AXIS2_PLACEMENT_3D('',#22088,#14703,#14704);
#12189=AXIS2_PLACEMENT_3D('',#22089,#14705,#14706);
#12190=AXIS2_PLACEMENT_3D('',#22090,#14707,#14708);
#12191=AXIS2_PLACEMENT_3D('',#22091,#14709,#14710);
#12192=AXIS2_PLACEMENT_3D('',#22092,#14711,#14712);
#12193=AXIS2_PLACEMENT_3D('',#22093,#14713,#14714);
#12194=AXIS2_PLACEMENT_3D('',#22094,#14715,#14716);
#12195=AXIS2_PLACEMENT_3D('',#22106,#14717,#14718);
#12196=AXIS2_PLACEMENT_3D('',#22116,#14719,#14720);
#12197=AXIS2_PLACEMENT_3D('',#22117,#14721,#14722);
#12198=AXIS2_PLACEMENT_3D('',#22132,#14727,#14728);
#12199=AXIS2_PLACEMENT_3D('',#22147,#14733,#14734);
#12200=AXIS2_PLACEMENT_3D('',#22148,#14735,#14736);
#12201=AXIS2_PLACEMENT_3D('',#22149,#14737,#14738);
#12202=AXIS2_PLACEMENT_3D('',#22150,#14739,#14740);
#12203=AXIS2_PLACEMENT_3D('',#22155,#14742,#14743);
#12204=AXIS2_PLACEMENT_3D('',#22158,#14745,#14746);
#12205=AXIS2_PLACEMENT_3D('',#22159,#14747,#14748);
#12206=AXIS2_PLACEMENT_3D('',#22169,#14750,#14751);
#12207=AXIS2_PLACEMENT_3D('',#22174,#14753,#14754);
#12208=AXIS2_PLACEMENT_3D('',#22177,#14756,#14757);
#12209=AXIS2_PLACEMENT_3D('',#22178,#14758,#14759);
#12210=AXIS2_PLACEMENT_3D('',#22188,#14762,#14763);
#12211=AXIS2_PLACEMENT_3D('',#22190,#14764,#14765);
#12212=AXIS2_PLACEMENT_3D('',#22193,#14767,#14768);
#12213=AXIS2_PLACEMENT_3D('',#22194,#14769,#14770);
#12214=AXIS2_PLACEMENT_3D('',#22200,#14774,#14775);
#12215=AXIS2_PLACEMENT_3D('',#22207,#14780,#14781);
#12216=AXIS2_PLACEMENT_3D('',#22209,#14782,#14783);
#12217=AXIS2_PLACEMENT_3D('',#22211,#14784,#14785);
#12218=AXIS2_PLACEMENT_3D('',#22215,#14787,#14788);
#12219=AXIS2_PLACEMENT_3D('',#22217,#14789,#14790);
#12220=AXIS2_PLACEMENT_3D('',#22219,#14791,#14792);
#12221=AXIS2_PLACEMENT_3D('',#22221,#14794,#14795);
#12222=AXIS2_PLACEMENT_3D('',#22222,#14796,#14797);
#12223=AXIS2_PLACEMENT_3D('',#22223,#14798,#14799);
#12224=AXIS2_PLACEMENT_3D('',#22224,#14800,#14801);
#12225=AXIS2_PLACEMENT_3D('',#22225,#14802,#14803);
#12226=AXIS2_PLACEMENT_3D('',#22226,#14804,#14805);
#12227=AXIS2_PLACEMENT_3D('',#22227,#14806,#14807);
#12228=AXIS2_PLACEMENT_3D('',#22228,#14808,#14809);
#12229=AXIS2_PLACEMENT_3D('',#22229,#14810,#14811);
#12230=AXIS2_PLACEMENT_3D('',#22230,#14812,#14813);
#12231=AXIS2_PLACEMENT_3D('',#22231,#14814,#14815);
#12232=AXIS2_PLACEMENT_3D('',#22232,#14816,#14817);
#12233=AXIS2_PLACEMENT_3D('',#22233,#14818,#14819);
#12234=AXIS2_PLACEMENT_3D('',#22234,#14820,#14821);
#12235=AXIS2_PLACEMENT_3D('',#22235,#14822,#14823);
#12236=AXIS2_PLACEMENT_3D('',#22236,#14824,#14825);
#12237=AXIS2_PLACEMENT_3D('',#22237,#14826,#14827);
#12238=AXIS2_PLACEMENT_3D('',#22238,#14828,#14829);
#12239=AXIS2_PLACEMENT_3D('',#22239,#14830,#14831);
#12240=AXIS2_PLACEMENT_3D('',#22240,#14832,#14833);
#12241=AXIS2_PLACEMENT_3D('',#22241,#14834,#14835);
#12242=AXIS2_PLACEMENT_3D('',#22242,#14836,#14837);
#12243=AXIS2_PLACEMENT_3D('',#22243,#14838,#14839);
#12244=AXIS2_PLACEMENT_3D('',#22244,#14840,#14841);
#12245=AXIS2_PLACEMENT_3D('',#22245,#14842,#14843);
#12246=AXIS2_PLACEMENT_3D('',#22246,#14844,#14845);
#12247=AXIS2_PLACEMENT_3D('',#22247,#14846,#14847);
#12248=AXIS2_PLACEMENT_3D('',#22248,#14848,#14849);
#12249=AXIS2_PLACEMENT_3D('',#22249,#14850,#14851);
#12250=AXIS2_PLACEMENT_3D('',#22250,#14852,#14853);
#12251=AXIS2_PLACEMENT_3D('',#22251,#14854,#14855);
#12252=AXIS2_PLACEMENT_3D('',#22252,#14856,#14857);
#12253=AXIS2_PLACEMENT_3D('',#22253,#14858,#14859);
#12254=AXIS2_PLACEMENT_3D('',#23068,#14860,#14861);
#12255=AXIS2_PLACEMENT_3D('',#23889,#14862,#14863);
#12256=AXIS2_PLACEMENT_3D('',#23984,#14864,#14865);
#12257=AXIS2_PLACEMENT_3D('',#24009,#14866,#14867);
#12258=AXIS2_PLACEMENT_3D('',#24092,#14868,#14869);
#12259=AXIS2_PLACEMENT_3D('',#24093,#14870,#14871);
#12260=AXIS2_PLACEMENT_3D('',#24094,#14872,#14873);
#12261=AXIS2_PLACEMENT_3D('',#24095,#14874,#14875);
#12262=AXIS2_PLACEMENT_3D('',#24096,#14876,#14877);
#12263=AXIS2_PLACEMENT_3D('',#24097,#14878,#14879);
#12264=AXIS2_PLACEMENT_3D('',#24098,#14880,#14881);
#12265=AXIS2_PLACEMENT_3D('',#24099,#14882,#14883);
#12266=AXIS2_PLACEMENT_3D('',#24100,#14884,#14885);
#12267=AXIS2_PLACEMENT_3D('',#24217,#14886,#14887);
#12268=AXIS2_PLACEMENT_3D('',#24218,#14888,#14889);
#12269=AXIS2_PLACEMENT_3D('',#24219,#14890,#14891);
#12270=AXIS2_PLACEMENT_3D('',#24238,#14892,#14893);
#12271=AXIS2_PLACEMENT_3D('',#24239,#14894,#14895);
#12272=AXIS2_PLACEMENT_3D('',#24240,#14896,#14897);
#12273=AXIS2_PLACEMENT_3D('',#24241,#14898,#14899);
#12274=AXIS2_PLACEMENT_3D('',#24266,#14900,#14901);
#12275=AXIS2_PLACEMENT_3D('',#24267,#14902,#14903);
#12276=AXIS2_PLACEMENT_3D('',#24320,#14904,#14905);
#12277=AXIS2_PLACEMENT_3D('',#24321,#14906,#14907);
#12278=AXIS2_PLACEMENT_3D('',#24459,#14908,#14909);
#12279=AXIS2_PLACEMENT_3D('',#24460,#14910,#14911);
#12280=AXIS2_PLACEMENT_3D('',#24461,#14912,#14913);
#12281=AXIS2_PLACEMENT_3D('',#24520,#14914,#14915);
#12282=AXIS2_PLACEMENT_3D('',#24521,#14916,#14917);
#12283=AXIS2_PLACEMENT_3D('',#24522,#14918,#14919);
#12284=AXIS2_PLACEMENT_3D('',#24581,#14920,#14921);
#12285=AXIS2_PLACEMENT_3D('',#24582,#14922,#14923);
#12286=AXIS2_PLACEMENT_3D('',#24583,#14924,#14925);
#12287=AXIS2_PLACEMENT_3D('',#24584,#14926,#14927);
#12288=AXIS2_PLACEMENT_3D('',#24585,#14928,#14929);
#12289=AXIS2_PLACEMENT_3D('',#24586,#14930,#14931);
#12290=AXIS2_PLACEMENT_3D('',#24587,#14932,#14933);
#12291=AXIS2_PLACEMENT_3D('',#24618,#14934,#14935);
#12292=AXIS2_PLACEMENT_3D('',#24619,#14936,#14937);
#12293=AXIS2_PLACEMENT_3D('',#24620,#14938,#14939);
#12294=AXIS2_PLACEMENT_3D('',#24633,#14940,#14941);
#12295=AXIS2_PLACEMENT_3D('',#24646,#14942,#14943);
#12296=AXIS2_PLACEMENT_3D('',#24647,#14944,#14945);
#12297=AXIS2_PLACEMENT_3D('',#24648,#14946,#14947);
#12298=AXIS2_PLACEMENT_3D('',#24649,#14948,#14949);
#12299=AXIS2_PLACEMENT_3D('',#24650,#14950,#14951);
#12300=AXIS2_PLACEMENT_3D('',#24669,#14952,#14953);
#12301=AXIS2_PLACEMENT_3D('',#24688,#14954,#14955);
#12302=AXIS2_PLACEMENT_3D('',#24689,#14956,#14957);
#12303=AXIS2_PLACEMENT_3D('',#24690,#14958,#14959);
#12304=AXIS2_PLACEMENT_3D('',#24691,#14960,#14961);
#12305=AXIS2_PLACEMENT_3D('',#24692,#14962,#14963);
#12306=AXIS2_PLACEMENT_3D('',#24693,#14964,#14965);
#12307=AXIS2_PLACEMENT_3D('',#24712,#14966,#14967);
#12308=AXIS2_PLACEMENT_3D('',#24713,#14968,#14969);
#12309=AXIS2_PLACEMENT_3D('',#24739,#14970,#14971);
#12310=AXIS2_PLACEMENT_3D('',#24740,#14972,#14973);
#12311=AXIS2_PLACEMENT_3D('',#24826,#14974,#14975);
#12312=AXIS2_PLACEMENT_3D('',#24857,#14976,#14977);
#12313=AXIS2_PLACEMENT_3D('',#24934,#14978,#14979);
#12314=AXIS2_PLACEMENT_3D('',#25029,#14980,#14981);
#12315=AXIS2_PLACEMENT_3D('',#25030,#14982,#14983);
#12316=AXIS2_PLACEMENT_3D('',#25031,#14984,#14985);
#12317=AXIS2_PLACEMENT_3D('',#25032,#14986,#14987);
#12318=AXIS2_PLACEMENT_3D('',#25033,#14988,#14989);
#12319=AXIS2_PLACEMENT_3D('',#25080,#14990,#14991);
#12320=AXIS2_PLACEMENT_3D('',#25081,#14992,#14993);
#12321=AXIS2_PLACEMENT_3D('',#25155,#14994,#14995);
#12322=AXIS2_PLACEMENT_3D('',#25156,#14996,#14997);
#12323=AXIS2_PLACEMENT_3D('',#25175,#14998,#14999);
#12324=AXIS2_PLACEMENT_3D('',#25236,#15000,#15001);
#12325=AXIS2_PLACEMENT_3D('',#25237,#15002,#15003);
#12326=AXIS2_PLACEMENT_3D('',#25238,#15004,#15005);
#12327=AXIS2_PLACEMENT_3D('',#25239,#15006,#15007);
#12328=AXIS2_PLACEMENT_3D('',#25240,#15008,#15009);
#12329=AXIS2_PLACEMENT_3D('',#25241,#15010,#15011);
#12330=AXIS2_PLACEMENT_3D('',#25242,#15012,#15013);
#12331=AXIS2_PLACEMENT_3D('',#25255,#15014,#15015);
#12332=AXIS2_PLACEMENT_3D('',#25311,#15016,#15017);
#12333=AXIS2_PLACEMENT_3D('',#25372,#15018,#15019);
#12334=AXIS2_PLACEMENT_3D('',#25373,#15020,#15021);
#12335=AXIS2_PLACEMENT_3D('',#25374,#15022,#15023);
#12336=AXIS2_PLACEMENT_3D('',#25463,#15024,#15025);
#12337=AXIS2_PLACEMENT_3D('',#25552,#15026,#15027);
#12338=AXIS2_PLACEMENT_3D('',#25553,#15028,#15029);
#12339=AXIS2_PLACEMENT_3D('',#25554,#15030,#15031);
#12340=AXIS2_PLACEMENT_3D('',#25555,#15032,#15033);
#12341=AXIS2_PLACEMENT_3D('',#25556,#15034,#15035);
#12342=AXIS2_PLACEMENT_3D('',#25557,#15036,#15037);
#12343=AXIS2_PLACEMENT_3D('',#25558,#15038,#15039);
#12344=AXIS2_PLACEMENT_3D('',#25559,#15040,#15041);
#12345=AXIS2_PLACEMENT_3D('',#25560,#15042,#15043);
#12346=AXIS2_PLACEMENT_3D('',#25561,#15044,#15045);
#12347=AXIS2_PLACEMENT_3D('',#25562,#15046,#15047);
#12348=AXIS2_PLACEMENT_3D('',#25563,#15048,#15049);
#12349=AXIS2_PLACEMENT_3D('',#25564,#15050,#15051);
#12350=AXIS2_PLACEMENT_3D('',#25565,#15052,#15053);
#12351=AXIS2_PLACEMENT_3D('',#25566,#15054,#15055);
#12352=AXIS2_PLACEMENT_3D('',#25585,#15056,#15057);
#12353=AXIS2_PLACEMENT_3D('',#25656,#15058,#15059);
#12354=AXIS2_PLACEMENT_3D('',#25763,#15060,#15061);
#12355=AXIS2_PLACEMENT_3D('',#25846,#15062,#15063);
#12356=AXIS2_PLACEMENT_3D('',#25847,#15064,#15065);
#12357=AXIS2_PLACEMENT_3D('',#25848,#15066,#15067);
#12358=AXIS2_PLACEMENT_3D('',#25849,#15068,#15069);
#12359=AXIS2_PLACEMENT_3D('',#25850,#15070,#15071);
#12360=AXIS2_PLACEMENT_3D('',#25851,#15072,#15073);
#12361=AXIS2_PLACEMENT_3D('',#25852,#15074,#15075);
#12362=AXIS2_PLACEMENT_3D('',#25853,#15076,#15077);
#12363=AXIS2_PLACEMENT_3D('',#25854,#15078,#15079);
#12364=AXIS2_PLACEMENT_3D('',#25901,#15080,#15081);
#12365=AXIS2_PLACEMENT_3D('',#25902,#15082,#15083);
#12366=AXIS2_PLACEMENT_3D('',#25903,#15084,#15085);
#12367=AXIS2_PLACEMENT_3D('',#25904,#15086,#15087);
#12368=AXIS2_PLACEMENT_3D('',#25981,#15088,#15089);
#12369=AXIS2_PLACEMENT_3D('',#25982,#15090,#15091);
#12370=AXIS2_PLACEMENT_3D('',#25983,#15092,#15093);
#12371=AXIS2_PLACEMENT_3D('',#25984,#15094,#15095);
#12372=AXIS2_PLACEMENT_3D('',#25997,#15096,#15097);
#12373=AXIS2_PLACEMENT_3D('',#25998,#15098,#15099);
#12374=AXIS2_PLACEMENT_3D('',#25999,#15100,#15101);
#12375=AXIS2_PLACEMENT_3D('',#26000,#15102,#15103);
#12376=AXIS2_PLACEMENT_3D('',#26001,#15104,#15105);
#12377=AXIS2_PLACEMENT_3D('',#26002,#15106,#15107);
#12378=AXIS2_PLACEMENT_3D('',#26119,#15108,#15109);
#12379=AXIS2_PLACEMENT_3D('',#26120,#15110,#15111);
#12380=AXIS2_PLACEMENT_3D('',#26121,#15112,#15113);
#12381=AXIS2_PLACEMENT_3D('',#26140,#15114,#15115);
#12382=AXIS2_PLACEMENT_3D('',#26141,#15116,#15117);
#12383=AXIS2_PLACEMENT_3D('',#26142,#15118,#15119);
#12384=AXIS2_PLACEMENT_3D('',#26143,#15120,#15121);
#12385=AXIS2_PLACEMENT_3D('',#26144,#15122,#15123);
#12386=AXIS2_PLACEMENT_3D('',#26145,#15124,#15125);
#12387=AXIS2_PLACEMENT_3D('',#26176,#15126,#15127);
#12388=AXIS2_PLACEMENT_3D('',#26177,#15128,#15129);
#12389=AXIS2_PLACEMENT_3D('',#26178,#15130,#15131);
#12390=AXIS2_PLACEMENT_3D('',#26179,#15132,#15133);
#12391=AXIS2_PLACEMENT_3D('',#26180,#15134,#15135);
#12392=AXIS2_PLACEMENT_3D('',#26181,#15136,#15137);
#12393=AXIS2_PLACEMENT_3D('',#26182,#15138,#15139);
#12394=AXIS2_PLACEMENT_3D('',#26183,#15140,#15141);
#12395=AXIS2_PLACEMENT_3D('',#26184,#15142,#15143);
#12396=AXIS2_PLACEMENT_3D('',#26185,#15144,#15145);
#12397=AXIS2_PLACEMENT_3D('',#26186,#15146,#15147);
#12398=AXIS2_PLACEMENT_3D('',#26324,#15148,#15149);
#12399=AXIS2_PLACEMENT_3D('',#26325,#15150,#15151);
#12400=AXIS2_PLACEMENT_3D('',#26326,#15152,#15153);
#12401=AXIS2_PLACEMENT_3D('',#26385,#15154,#15155);
#12402=AXIS2_PLACEMENT_3D('',#26386,#15156,#15157);
#12403=AXIS2_PLACEMENT_3D('',#26387,#15158,#15159);
#12404=AXIS2_PLACEMENT_3D('',#26422,#15160,#15161);
#12405=AXIS2_PLACEMENT_3D('',#26423,#15162,#15163);
#12406=AXIS2_PLACEMENT_3D('',#26424,#15164,#15165);
#12407=AXIS2_PLACEMENT_3D('',#26471,#15166,#15167);
#12408=AXIS2_PLACEMENT_3D('',#26472,#15168,#15169);
#12409=AXIS2_PLACEMENT_3D('',#26473,#15170,#15171);
#12410=AXIS2_PLACEMENT_3D('',#26474,#15172,#15173);
#12411=AXIS2_PLACEMENT_3D('',#26475,#15174,#15175);
#12412=AXIS2_PLACEMENT_3D('',#26476,#15176,#15177);
#12413=AXIS2_PLACEMENT_3D('',#26477,#15178,#15179);
#12414=AXIS2_PLACEMENT_3D('',#26512,#15180,#15181);
#12415=AXIS2_PLACEMENT_3D('',#26513,#15182,#15183);
#12416=AXIS2_PLACEMENT_3D('',#26526,#15184,#15185);
#12417=AXIS2_PLACEMENT_3D('',#26539,#15186,#15187);
#12418=AXIS2_PLACEMENT_3D('',#26540,#15188,#15189);
#12419=AXIS2_PLACEMENT_3D('',#26541,#15190,#15191);
#12420=AXIS2_PLACEMENT_3D('',#26542,#15192,#15193);
#12421=AXIS2_PLACEMENT_3D('',#26543,#15194,#15195);
#12422=AXIS2_PLACEMENT_3D('',#26562,#15196,#15197);
#12423=AXIS2_PLACEMENT_3D('',#26611,#15198,#15199);
#12424=AXIS2_PLACEMENT_3D('',#26612,#15200,#15201);
#12425=AXIS2_PLACEMENT_3D('',#26631,#15202,#15203);
#12426=AXIS2_PLACEMENT_3D('',#26738,#15204,#15205);
#12427=AXIS2_PLACEMENT_3D('',#26833,#15206,#15207);
#12428=AXIS2_PLACEMENT_3D('',#26834,#15208,#15209);
#12429=AXIS2_PLACEMENT_3D('',#26835,#15210,#15211);
#12430=AXIS2_PLACEMENT_3D('',#26836,#15212,#15213);
#12431=AXIS2_PLACEMENT_3D('',#26837,#15214,#15215);
#12432=AXIS2_PLACEMENT_3D('',#26838,#15216,#15217);
#12433=AXIS2_PLACEMENT_3D('',#26839,#15218,#15219);
#12434=AXIS2_PLACEMENT_3D('',#26840,#15220,#15221);
#12435=AXIS2_PLACEMENT_3D('',#26872,#15222,#15223);
#12436=AXIS2_PLACEMENT_3D('',#26873,#15224,#15225);
#12437=AXIS2_PLACEMENT_3D('',#26874,#15226,#15227);
#12438=AXIS2_PLACEMENT_3D('',#26875,#15228,#15229);
#12439=AXIS2_PLACEMENT_3D('',#26876,#15230,#15231);
#12440=AXIS2_PLACEMENT_3D('',#26877,#15232,#15233);
#12441=AXIS2_PLACEMENT_3D('',#26890,#15234,#15235);
#12442=AXIS2_PLACEMENT_3D('',#26891,#15236,#15237);
#12443=AXIS2_PLACEMENT_3D('',#26892,#15238,#15239);
#12444=AXIS2_PLACEMENT_3D('',#26966,#15240,#15241);
#12445=AXIS2_PLACEMENT_3D('',#26967,#15242,#15243);
#12446=AXIS2_PLACEMENT_3D('',#26968,#15244,#15245);
#12447=AXIS2_PLACEMENT_3D('',#26969,#15246,#15247);
#12448=AXIS2_PLACEMENT_3D('',#26970,#15248,#15249);
#12449=AXIS2_PLACEMENT_3D('',#26971,#15250,#15251);
#12450=AXIS2_PLACEMENT_3D('',#26972,#15252,#15253);
#12451=AXIS2_PLACEMENT_3D('',#26973,#15254,#15255);
#12452=AXIS2_PLACEMENT_3D('',#26974,#15256,#15257);
#12453=AXIS2_PLACEMENT_3D('',#26975,#15258,#15259);
#12454=AXIS2_PLACEMENT_3D('',#26976,#15260,#15261);
#12455=AXIS2_PLACEMENT_3D('',#26977,#15262,#15263);
#12456=AXIS2_PLACEMENT_3D('',#26978,#15264,#15265);
#12457=AXIS2_PLACEMENT_3D('',#26979,#15266,#15267);
#12458=AXIS2_PLACEMENT_3D('',#26980,#15268,#15269);
#12459=AXIS2_PLACEMENT_3D('',#26981,#15270,#15271);
#12460=AXIS2_PLACEMENT_3D('',#26982,#15272,#15273);
#12461=AXIS2_PLACEMENT_3D('',#27059,#15274,#15275);
#12462=AXIS2_PLACEMENT_3D('',#27106,#15276,#15277);
#12463=AXIS2_PLACEMENT_3D('',#27107,#15278,#15279);
#12464=AXIS2_PLACEMENT_3D('',#27108,#15280,#15281);
#12465=AXIS2_PLACEMENT_3D('',#27109,#15282,#15283);
#12466=AXIS2_PLACEMENT_3D('',#27186,#15284,#15285);
#12467=AXIS2_PLACEMENT_3D('',#27187,#15286,#15287);
#12468=AXIS2_PLACEMENT_3D('',#27188,#15288,#15289);
#12469=AXIS2_PLACEMENT_3D('',#27189,#15290,#15291);
#12470=AXIS2_PLACEMENT_3D('',#27190,#15292,#15293);
#12471=AXIS2_PLACEMENT_3D('',#27191,#15294,#15295);
#12472=AXIS2_PLACEMENT_3D('',#27192,#15296,#15297);
#12473=AXIS2_PLACEMENT_3D('',#27245,#15298,#15299);
#12474=AXIS2_PLACEMENT_3D('',#27246,#15300,#15301);
#12475=AXIS2_PLACEMENT_3D('',#27277,#15302,#15303);
#12476=AXIS2_PLACEMENT_3D('',#27278,#15304,#15305);
#12477=AXIS2_PLACEMENT_3D('',#27279,#15306,#15307);
#12478=AXIS2_PLACEMENT_3D('',#27280,#15308,#15309);
#12479=AXIS2_PLACEMENT_3D('',#27281,#15310,#15311);
#12480=AXIS2_PLACEMENT_3D('',#27379,#15312,#15313);
#12481=AXIS2_PLACEMENT_3D('',#27380,#15314,#15315);
#12482=AXIS2_PLACEMENT_3D('',#27381,#15316,#15317);
#12483=AXIS2_PLACEMENT_3D('',#27382,#15318,#15319);
#12484=AXIS2_PLACEMENT_3D('',#27383,#15320,#15321);
#12485=AXIS2_PLACEMENT_3D('',#27384,#15322,#15323);
#12486=AXIS2_PLACEMENT_3D('',#27431,#15324,#15325);
#12487=AXIS2_PLACEMENT_3D('',#27462,#15326,#15327);
#12488=AXIS2_PLACEMENT_3D('',#27463,#15328,#15329);
#12489=AXIS2_PLACEMENT_3D('',#27464,#15330,#15331);
#12490=AXIS2_PLACEMENT_3D('',#27465,#15332,#15333);
#12491=AXIS2_PLACEMENT_3D('',#27490,#15334,#15335);
#12492=AXIS2_PLACEMENT_3D('',#27491,#15336,#15337);
#12493=AXIS2_PLACEMENT_3D('',#27522,#15338,#15339);
#12494=AXIS2_PLACEMENT_3D('',#27523,#15340,#15341);
#12495=AXIS2_PLACEMENT_3D('',#27524,#15342,#15343);
#12496=AXIS2_PLACEMENT_3D('',#27543,#15344,#15345);
#12497=AXIS2_PLACEMENT_3D('',#27599,#15346,#15347);
#12498=AXIS2_PLACEMENT_3D('',#27600,#15348,#15349);
#12499=AXIS2_PLACEMENT_3D('',#27601,#15350,#15351);
#12500=AXIS2_PLACEMENT_3D('',#27602,#15352,#15353);
#12501=AXIS2_PLACEMENT_3D('',#27634,#15354,#15355);
#12502=AXIS2_PLACEMENT_3D('',#27635,#15356,#15357);
#12503=AXIS2_PLACEMENT_3D('',#27636,#15358,#15359);
#12504=AXIS2_PLACEMENT_3D('',#27637,#15360,#15361);
#12505=AXIS2_PLACEMENT_3D('',#27723,#15362,#15363);
#12506=AXIS2_PLACEMENT_3D('',#27742,#15364,#15365);
#12507=AXIS2_PLACEMENT_3D('',#27743,#15366,#15367);
#12508=AXIS2_PLACEMENT_3D('',#27744,#15368,#15369);
#12509=AXIS2_PLACEMENT_3D('',#27763,#15370,#15371);
#12510=AXIS2_PLACEMENT_3D('',#27824,#15372,#15373);
#12511=AXIS2_PLACEMENT_3D('',#27825,#15374,#15375);
#12512=AXIS2_PLACEMENT_3D('',#27826,#15376,#15377);
#12513=AXIS2_PLACEMENT_3D('',#27827,#15378,#15379);
#12514=AXIS2_PLACEMENT_3D('',#27828,#15380,#15381);
#12515=AXIS2_PLACEMENT_3D('',#27829,#15382,#15383);
#12516=AXIS2_PLACEMENT_3D('',#27830,#15384,#15385);
#12517=AXIS2_PLACEMENT_3D('',#27831,#15386,#15387);
#12518=AXIS2_PLACEMENT_3D('',#27832,#15388,#15389);
#12519=AXIS2_PLACEMENT_3D('',#27833,#15390,#15391);
#12520=AXIS2_PLACEMENT_3D('',#27834,#15392,#15393);
#12521=AXIS2_PLACEMENT_3D('',#27835,#15394,#15395);
#12522=AXIS2_PLACEMENT_3D('',#27836,#15396,#15397);
#12523=AXIS2_PLACEMENT_3D('',#27871,#15398,#15399);
#12524=AXIS2_PLACEMENT_3D('',#27890,#15400,#15401);
#12525=AXIS2_PLACEMENT_3D('',#28064,#15402,#15403);
#12526=AXIS2_PLACEMENT_3D('',#28065,#15404,#15405);
#12527=AXIS2_PLACEMENT_3D('',#28066,#15406,#15407);
#12528=AXIS2_PLACEMENT_3D('',#28067,#15408,#15409);
#12529=AXIS2_PLACEMENT_3D('',#28080,#15410,#15411);
#12530=AXIS2_PLACEMENT_3D('',#28093,#15412,#15413);
#12531=AXIS2_PLACEMENT_3D('',#28094,#15414,#15415);
#12532=AXIS2_PLACEMENT_3D('',#28183,#15416,#15417);
#12533=AXIS2_PLACEMENT_3D('',#28184,#15418,#15419);
#12534=AXIS2_PLACEMENT_3D('',#28209,#15420,#15421);
#12535=AXIS2_PLACEMENT_3D('',#28210,#15422,#15423);
#12536=AXIS2_PLACEMENT_3D('',#28211,#15424,#15425);
#12537=AXIS2_PLACEMENT_3D('',#28212,#15426,#15427);
#12538=AXIS2_PLACEMENT_3D('',#28213,#15428,#15429);
#12539=AXIS2_PLACEMENT_3D('',#28214,#15430,#15431);
#12540=AXIS2_PLACEMENT_3D('',#28215,#15432,#15433);
#12541=AXIS2_PLACEMENT_3D('',#28216,#15434,#15435);
#12542=AXIS2_PLACEMENT_3D('',#28217,#15436,#15437);
#12543=AXIS2_PLACEMENT_3D('',#28218,#15438,#15439);
#12544=AXIS2_PLACEMENT_3D('',#28219,#15440,#15441);
#12545=AXIS2_PLACEMENT_3D('',#28220,#15442,#15443);
#12546=AXIS2_PLACEMENT_3D('',#28221,#15444,#15445);
#12547=AXIS2_PLACEMENT_3D('',#28235,#15446,#15447);
#12548=AXIS2_PLACEMENT_3D('',#28236,#15448,#15449);
#12549=AXIS2_PLACEMENT_3D('',#28237,#15450,#15451);
#12550=AXIS2_PLACEMENT_3D('',#28238,#15452,#15453);
#12551=AXIS2_PLACEMENT_3D('',#28239,#15454,#15455);
#12552=AXIS2_PLACEMENT_3D('',#28240,#15456,#15457);
#12553=AXIS2_PLACEMENT_3D('',#28241,#15458,#15459);
#12554=AXIS2_PLACEMENT_3D('',#28260,#15460,#15461);
#12555=AXIS2_PLACEMENT_3D('',#28261,#15462,#15463);
#12556=AXIS2_PLACEMENT_3D('',#28262,#15464,#15465);
#12557=AXIS2_PLACEMENT_3D('',#28263,#15466,#15467);
#12558=AXIS2_PLACEMENT_3D('',#28276,#15468,#15469);
#12559=AXIS2_PLACEMENT_3D('',#28277,#15470,#15471);
#12560=AXIS2_PLACEMENT_3D('',#28278,#15472,#15473);
#12561=AXIS2_PLACEMENT_3D('',#28279,#15474,#15475);
#12562=AXIS2_PLACEMENT_3D('',#28280,#15476,#15477);
#12563=AXIS2_PLACEMENT_3D('',#28281,#15478,#15479);
#12564=AXIS2_PLACEMENT_3D('',#28298,#15480,#15481);
#12565=AXIS2_PLACEMENT_3D('',#28323,#15482,#15483);
#12566=AXIS2_PLACEMENT_3D('',#28324,#15484,#15485);
#12567=AXIS2_PLACEMENT_3D('',#28325,#15486,#15487);
#12568=AXIS2_PLACEMENT_3D('',#28326,#15488,#15489);
#12569=AXIS2_PLACEMENT_3D('',#28327,#15490,#15491);
#12570=AXIS2_PLACEMENT_3D('',#28328,#15492,#15493);
#12571=AXIS2_PLACEMENT_3D('',#28329,#15494,#15495);
#12572=AXIS2_PLACEMENT_3D('',#28330,#15496,#15497);
#12573=AXIS2_PLACEMENT_3D('',#28331,#15498,#15499);
#12574=AXIS2_PLACEMENT_3D('',#28332,#15500,#15501);
#12575=AXIS2_PLACEMENT_3D('',#28333,#15502,#15503);
#12576=AXIS2_PLACEMENT_3D('',#28334,#15504,#15505);
#12577=AXIS2_PLACEMENT_3D('',#28353,#15506,#15507);
#12578=AXIS2_PLACEMENT_3D('',#28354,#15508,#15509);
#12579=AXIS2_PLACEMENT_3D('',#28355,#15510,#15511);
#12580=AXIS2_PLACEMENT_3D('',#28356,#15512,#15513);
#12581=AXIS2_PLACEMENT_3D('',#28357,#15514,#15515);
#12582=AXIS2_PLACEMENT_3D('',#28358,#15516,#15517);
#12583=AXIS2_PLACEMENT_3D('',#28359,#15518,#15519);
#12584=AXIS2_PLACEMENT_3D('',#28360,#15520,#15521);
#12585=AXIS2_PLACEMENT_3D('',#28395,#15522,#15523);
#12586=AXIS2_PLACEMENT_3D('',#28396,#15524,#15525);
#12587=AXIS2_PLACEMENT_3D('',#28397,#15526,#15527);
#12588=AXIS2_PLACEMENT_3D('',#28398,#15528,#15529);
#12589=AXIS2_PLACEMENT_3D('',#28399,#15530,#15531);
#12590=AXIS2_PLACEMENT_3D('',#28400,#15532,#15533);
#12591=AXIS2_PLACEMENT_3D('',#28401,#15534,#15535);
#12592=AXIS2_PLACEMENT_3D('',#28402,#15536,#15537);
#12593=AXIS2_PLACEMENT_3D('',#28419,#15538,#15539);
#12594=AXIS2_PLACEMENT_3D('',#28420,#15540,#15541);
#12595=AXIS2_PLACEMENT_3D('',#28439,#15542,#15543);
#12596=AXIS2_PLACEMENT_3D('',#28440,#15544,#15545);
#12597=AXIS2_PLACEMENT_3D('',#28441,#15546,#15547);
#12598=AXIS2_PLACEMENT_3D('',#28442,#15548,#15549);
#12599=AXIS2_PLACEMENT_3D('',#28443,#15550,#15551);
#12600=AXIS2_PLACEMENT_3D('',#28444,#15552,#15553);
#12601=AXIS2_PLACEMENT_3D('',#28445,#15554,#15555);
#12602=AXIS2_PLACEMENT_3D('',#28446,#15556,#15557);
#12603=AXIS2_PLACEMENT_3D('',#28447,#15558,#15559);
#12604=AXIS2_PLACEMENT_3D('',#28466,#15560,#15561);
#12605=AXIS2_PLACEMENT_3D('',#28467,#15562,#15563);
#12606=AXIS2_PLACEMENT_3D('',#28468,#15564,#15565);
#12607=AXIS2_PLACEMENT_3D('',#28469,#15566,#15567);
#12608=AXIS2_PLACEMENT_3D('',#28470,#15568,#15569);
#12609=AXIS2_PLACEMENT_3D('',#28471,#15570,#15571);
#12610=AXIS2_PLACEMENT_3D('',#28472,#15572,#15573);
#12611=AXIS2_PLACEMENT_3D('',#28473,#15574,#15575);
#12612=AXIS2_PLACEMENT_3D('',#28528,#15576,#15577);
#12613=AXIS2_PLACEMENT_3D('',#28529,#15578,#15579);
#12614=AXIS2_PLACEMENT_3D('',#28549,#15580,#15581);
#12615=AXIS2_PLACEMENT_3D('',#28550,#15582,#15583);
#12616=AXIS2_PLACEMENT_3D('',#28551,#15584,#15585);
#12617=AXIS2_PLACEMENT_3D('',#28552,#15586,#15587);
#12618=AXIS2_PLACEMENT_3D('',#28566,#15588,#15589);
#12619=AXIS2_PLACEMENT_3D('',#28567,#15590,#15591);
#12620=AXIS2_PLACEMENT_3D('',#28568,#15592,#15593);
#12621=AXIS2_PLACEMENT_3D('',#28593,#15594,#15595);
#12622=AXIS2_PLACEMENT_3D('',#28594,#15596,#15597);
#12623=AXIS2_PLACEMENT_3D('',#28595,#15598,#15599);
#12624=AXIS2_PLACEMENT_3D('',#28596,#15600,#15601);
#12625=AXIS2_PLACEMENT_3D('',#28597,#15602,#15603);
#12626=AXIS2_PLACEMENT_3D('',#28610,#15604,#15605);
#12627=AXIS2_PLACEMENT_3D('',#28611,#15606,#15607);
#12628=AXIS2_PLACEMENT_3D('',#28612,#15608,#15609);
#12629=AXIS2_PLACEMENT_3D('',#28613,#15610,#15611);
#12630=AXIS2_PLACEMENT_3D('',#28614,#15612,#15613);
#12631=AXIS2_PLACEMENT_3D('',#28615,#15614,#15615);
#12632=AXIS2_PLACEMENT_3D('',#28634,#15616,#15617);
#12633=AXIS2_PLACEMENT_3D('',#28635,#15618,#15619);
#12634=AXIS2_PLACEMENT_3D('',#28636,#15620,#15621);
#12635=AXIS2_PLACEMENT_3D('',#28655,#15622,#15623);
#12636=AXIS2_PLACEMENT_3D('',#28674,#15624,#15625);
#12637=AXIS2_PLACEMENT_3D('',#28688,#15626,#15627);
#12638=AXIS2_PLACEMENT_3D('',#28689,#15628,#15629);
#12639=AXIS2_PLACEMENT_3D('',#28690,#15630,#15631);
#12640=AXIS2_PLACEMENT_3D('',#28691,#15632,#15633);
#12641=AXIS2_PLACEMENT_3D('',#28692,#15634,#15635);
#12642=AXIS2_PLACEMENT_3D('',#28693,#15636,#15637);
#12643=AXIS2_PLACEMENT_3D('',#28713,#15638,#15639);
#12644=AXIS2_PLACEMENT_3D('',#28714,#15640,#15641);
#12645=AXIS2_PLACEMENT_3D('',#28715,#15642,#15643);
#12646=AXIS2_PLACEMENT_3D('',#28716,#15644,#15645);
#12647=AXIS2_PLACEMENT_3D('',#28717,#15646,#15647);
#12648=AXIS2_PLACEMENT_3D('',#28718,#15648,#15649);
#12649=AXIS2_PLACEMENT_3D('',#28719,#15650,#15651);
#12650=AXIS2_PLACEMENT_3D('',#28720,#15652,#15653);
#12651=AXIS2_PLACEMENT_3D('',#28739,#15654,#15655);
#12652=AXIS2_PLACEMENT_3D('',#28740,#15656,#15657);
#12653=AXIS2_PLACEMENT_3D('',#28741,#15658,#15659);
#12654=AXIS2_PLACEMENT_3D('',#28742,#15660,#15661);
#12655=AXIS2_PLACEMENT_3D('',#28743,#15662,#15663);
#12656=AXIS2_PLACEMENT_3D('',#28744,#15664,#15665);
#12657=AXIS2_PLACEMENT_3D('',#28745,#15666,#15667);
#12658=AXIS2_PLACEMENT_3D('',#28746,#15668,#15669);
#12659=AXIS2_PLACEMENT_3D('',#28747,#15670,#15671);
#12660=AXIS2_PLACEMENT_3D('',#28748,#15672,#15673);
#12661=AXIS2_PLACEMENT_3D('',#28749,#15674,#15675);
#12662=AXIS2_PLACEMENT_3D('',#28768,#15676,#15677);
#12663=AXIS2_PLACEMENT_3D('',#28769,#15678,#15679);
#12664=AXIS2_PLACEMENT_3D('',#28770,#15680,#15681);
#12665=AXIS2_PLACEMENT_3D('',#28771,#15682,#15683);
#12666=AXIS2_PLACEMENT_3D('',#28772,#15684,#15685);
#12667=AXIS2_PLACEMENT_3D('',#28773,#15686,#15687);
#12668=AXIS2_PLACEMENT_3D('',#28774,#15688,#15689);
#12669=AXIS2_PLACEMENT_3D('',#28775,#15690,#15691);
#12670=AXIS2_PLACEMENT_3D('',#28776,#15692,#15693);
#12671=AXIS2_PLACEMENT_3D('',#28811,#15694,#15695);
#12672=AXIS2_PLACEMENT_3D('',#28812,#15696,#15697);
#12673=AXIS2_PLACEMENT_3D('',#28813,#15698,#15699);
#12674=AXIS2_PLACEMENT_3D('',#28814,#15700,#15701);
#12675=AXIS2_PLACEMENT_3D('',#28815,#15702,#15703);
#12676=AXIS2_PLACEMENT_3D('',#28816,#15704,#15705);
#12677=AXIS2_PLACEMENT_3D('',#28817,#15706,#15707);
#12678=AXIS2_PLACEMENT_3D('',#28872,#15708,#15709);
#12679=AXIS2_PLACEMENT_3D('',#28873,#15710,#15711);
#12680=AXIS2_PLACEMENT_3D('',#28874,#15712,#15713);
#12681=AXIS2_PLACEMENT_3D('',#28875,#15714,#15715);
#12682=AXIS2_PLACEMENT_3D('',#28910,#15716,#15717);
#12683=AXIS2_PLACEMENT_3D('',#28911,#15718,#15719);
#12684=AXIS2_PLACEMENT_3D('',#28912,#15720,#15721);
#12685=AXIS2_PLACEMENT_3D('',#28913,#15722,#15723);
#12686=AXIS2_PLACEMENT_3D('',#28914,#15724,#15725);
#12687=AXIS2_PLACEMENT_3D('',#28915,#15726,#15727);
#12688=AXIS2_PLACEMENT_3D('',#28916,#15728,#15729);
#12689=AXIS2_PLACEMENT_3D('',#28917,#15730,#15731);
#12690=AXIS2_PLACEMENT_3D('',#28918,#15732,#15733);
#12691=AXIS2_PLACEMENT_3D('',#28919,#15734,#15735);
#12692=AXIS2_PLACEMENT_3D('',#28920,#15736,#15737);
#12693=AXIS2_PLACEMENT_3D('',#28921,#15738,#15739);
#12694=AXIS2_PLACEMENT_3D('',#28922,#15740,#15741);
#12695=AXIS2_PLACEMENT_3D('',#28923,#15742,#15743);
#12696=AXIS2_PLACEMENT_3D('',#28924,#15744,#15745);
#12697=AXIS2_PLACEMENT_3D('',#28937,#15746,#15747);
#12698=AXIS2_PLACEMENT_3D('',#28938,#15748,#15749);
#12699=AXIS2_PLACEMENT_3D('',#28961,#15750,#15751);
#12700=AXIS2_PLACEMENT_3D('',#28980,#15752,#15753);
#12701=AXIS2_PLACEMENT_3D('',#28999,#15754,#15755);
#12702=AXIS2_PLACEMENT_3D('',#29000,#15756,#15757);
#12703=AXIS2_PLACEMENT_3D('',#29001,#15758,#15759);
#12704=AXIS2_PLACEMENT_3D('',#29002,#15760,#15761);
#12705=AXIS2_PLACEMENT_3D('',#29003,#15762,#15763);
#12706=AXIS2_PLACEMENT_3D('',#29004,#15764,#15765);
#12707=AXIS2_PLACEMENT_3D('',#29005,#15766,#15767);
#12708=AXIS2_PLACEMENT_3D('',#29006,#15768,#15769);
#12709=AXIS2_PLACEMENT_3D('',#29007,#15770,#15771);
#12710=AXIS2_PLACEMENT_3D('',#29026,#15772,#15773);
#12711=AXIS2_PLACEMENT_3D('',#29043,#15774,#15775);
#12712=AXIS2_PLACEMENT_3D('',#29044,#15776,#15777);
#12713=AXIS2_PLACEMENT_3D('',#29045,#15778,#15779);
#12714=AXIS2_PLACEMENT_3D('',#29046,#15780,#15781);
#12715=AXIS2_PLACEMENT_3D('',#29107,#15782,#15783);
#12716=AXIS2_PLACEMENT_3D('',#29108,#15784,#15785);
#12717=AXIS2_PLACEMENT_3D('',#29109,#15786,#15787);
#12718=AXIS2_PLACEMENT_3D('',#29110,#15788,#15789);
#12719=AXIS2_PLACEMENT_3D('',#29111,#15790,#15791);
#12720=AXIS2_PLACEMENT_3D('',#29112,#15792,#15793);
#12721=AXIS2_PLACEMENT_3D('',#29113,#15794,#15795);
#12722=AXIS2_PLACEMENT_3D('',#29114,#15796,#15797);
#12723=AXIS2_PLACEMENT_3D('',#29139,#15798,#15799);
#12724=AXIS2_PLACEMENT_3D('',#29140,#15800,#15801);
#12725=AXIS2_PLACEMENT_3D('',#29141,#15802,#15803);
#12726=AXIS2_PLACEMENT_3D('',#29142,#15804,#15805);
#12727=AXIS2_PLACEMENT_3D('',#29143,#15806,#15807);
#12728=AXIS2_PLACEMENT_3D('',#29144,#15808,#15809);
#12729=AXIS2_PLACEMENT_3D('',#29145,#15810,#15811);
#12730=AXIS2_PLACEMENT_3D('',#29146,#15812,#15813);
#12731=AXIS2_PLACEMENT_3D('',#29147,#15814,#15815);
#12732=AXIS2_PLACEMENT_3D('',#29166,#15816,#15817);
#12733=AXIS2_PLACEMENT_3D('',#29186,#15818,#15819);
#12734=AXIS2_PLACEMENT_3D('',#29187,#15820,#15821);
#12735=AXIS2_PLACEMENT_3D('',#29219,#15822,#15823);
#12736=AXIS2_PLACEMENT_3D('',#29220,#15824,#15825);
#12737=AXIS2_PLACEMENT_3D('',#29221,#15826,#15827);
#12738=AXIS2_PLACEMENT_3D('',#29222,#15828,#15829);
#12739=AXIS2_PLACEMENT_3D('',#29223,#15830,#15831);
#12740=AXIS2_PLACEMENT_3D('',#29224,#15832,#15833);
#12741=AXIS2_PLACEMENT_3D('',#29225,#15834,#15835);
#12742=AXIS2_PLACEMENT_3D('',#29226,#15836,#15837);
#12743=AXIS2_PLACEMENT_3D('',#29227,#15838,#15839);
#12744=AXIS2_PLACEMENT_3D('',#29228,#15840,#15841);
#12745=AXIS2_PLACEMENT_3D('',#29241,#15842,#15843);
#12746=AXIS2_PLACEMENT_3D('',#29242,#15844,#15845);
#12747=AXIS2_PLACEMENT_3D('',#29243,#15846,#15847);
#12748=AXIS2_PLACEMENT_3D('',#29244,#15848,#15849);
#12749=AXIS2_PLACEMENT_3D('',#29245,#15850,#15851);
#12750=AXIS2_PLACEMENT_3D('',#29246,#15852,#15853);
#12751=AXIS2_PLACEMENT_3D('',#29247,#15854,#15855);
#12752=AXIS2_PLACEMENT_3D('',#29248,#15856,#15857);
#12753=AXIS2_PLACEMENT_3D('',#29249,#15858,#15859);
#12754=AXIS2_PLACEMENT_3D('',#29250,#15860,#15861);
#12755=AXIS2_PLACEMENT_3D('',#29270,#15862,#15863);
#12756=AXIS2_PLACEMENT_3D('',#29289,#15864,#15865);
#12757=AXIS2_PLACEMENT_3D('',#29290,#15866,#15867);
#12758=AXIS2_PLACEMENT_3D('',#29291,#15868,#15869);
#12759=AXIS2_PLACEMENT_3D('',#29292,#15870,#15871);
#12760=AXIS2_PLACEMENT_3D('',#29293,#15872,#15873);
#12761=AXIS2_PLACEMENT_3D('',#29294,#15874,#15875);
#12762=AXIS2_PLACEMENT_3D('',#29295,#15876,#15877);
#12763=AXIS2_PLACEMENT_3D('',#29296,#15878,#15879);
#12764=AXIS2_PLACEMENT_3D('',#29297,#15880,#15881);
#12765=AXIS2_PLACEMENT_3D('',#29298,#15882,#15883);
#12766=AXIS2_PLACEMENT_3D('',#29299,#15884,#15885);
#12767=AXIS2_PLACEMENT_3D('',#29354,#15886,#15887);
#12768=AXIS2_PLACEMENT_3D('',#29355,#15888,#15889);
#12769=AXIS2_PLACEMENT_3D('',#29356,#15890,#15891);
#12770=AXIS2_PLACEMENT_3D('',#29357,#15892,#15893);
#12771=AXIS2_PLACEMENT_3D('',#29358,#15894,#15895);
#12772=AXIS2_PLACEMENT_3D('',#29359,#15896,#15897);
#12773=AXIS2_PLACEMENT_3D('',#29360,#15898,#15899);
#12774=AXIS2_PLACEMENT_3D('',#29361,#15900,#15901);
#12775=AXIS2_PLACEMENT_3D('',#29362,#15902,#15903);
#12776=AXIS2_PLACEMENT_3D('',#29375,#15904,#15905);
#12777=AXIS2_PLACEMENT_3D('',#29416,#15906,#15907);
#12778=AXIS2_PLACEMENT_3D('',#29417,#15908,#15909);
#12779=AXIS2_PLACEMENT_3D('',#29418,#15910,#15911);
#12780=AXIS2_PLACEMENT_3D('',#29419,#15912,#15913);
#12781=AXIS2_PLACEMENT_3D('',#29420,#15914,#15915);
#12782=AXIS2_PLACEMENT_3D('',#29421,#15916,#15917);
#12783=AXIS2_PLACEMENT_3D('',#29422,#15918,#15919);
#12784=AXIS2_PLACEMENT_3D('',#29423,#15920,#15921);
#12785=AXIS2_PLACEMENT_3D('',#29424,#15922,#15923);
#12786=AXIS2_PLACEMENT_3D('',#29425,#15924,#15925);
#12787=AXIS2_PLACEMENT_3D('',#29426,#15926,#15927);
#12788=AXIS2_PLACEMENT_3D('',#29427,#15928,#15929);
#12789=AXIS2_PLACEMENT_3D('',#29428,#15930,#15931);
#12790=AXIS2_PLACEMENT_3D('',#29429,#15932,#15933);
#12791=AXIS2_PLACEMENT_3D('',#29430,#15934,#15935);
#12792=AXIS2_PLACEMENT_3D('',#30273,#15936,#15937);
#12793=AXIS2_PLACEMENT_3D('',#31065,#15938,#15939);
#12794=AXIS2_PLACEMENT_3D('',#31133,#15940,#15941);
#12795=AXIS2_PLACEMENT_3D('',#31140,#15942,#15943);
#12796=AXIS2_PLACEMENT_3D('',#31141,#15944,#15945);
#12797=AXIS2_PLACEMENT_3D('',#31142,#15946,#15947);
#12798=AXIS2_PLACEMENT_3D('',#31183,#15948,#15949);
#12799=AXIS2_PLACEMENT_3D('',#31202,#15950,#15951);
#12800=AXIS2_PLACEMENT_3D('',#31279,#15952,#15953);
#12801=AXIS2_PLACEMENT_3D('',#31280,#15954,#15955);
#12802=AXIS2_PLACEMENT_3D('',#31281,#15956,#15957);
#12803=AXIS2_PLACEMENT_3D('',#31282,#15958,#15959);
#12804=AXIS2_PLACEMENT_3D('',#31283,#15960,#15961);
#12805=AXIS2_PLACEMENT_3D('',#31284,#15962,#15963);
#12806=AXIS2_PLACEMENT_3D('',#31285,#15964,#15965);
#12807=AXIS2_PLACEMENT_3D('',#31488,#15966,#15967);
#12808=AXIS2_PLACEMENT_3D('',#31507,#15968,#15969);
#12809=AXIS2_PLACEMENT_3D('',#31554,#15970,#15971);
#12810=AXIS2_PLACEMENT_3D('',#31555,#15972,#15973);
#12811=AXIS2_PLACEMENT_3D('',#31610,#15974,#15975);
#12812=AXIS2_PLACEMENT_3D('',#31611,#15976,#15977);
#12813=AXIS2_PLACEMENT_3D('',#31612,#15978,#15979);
#12814=AXIS2_PLACEMENT_3D('',#31613,#15980,#15981);
#12815=AXIS2_PLACEMENT_3D('',#31723,#15982,#15983);
#12816=AXIS2_PLACEMENT_3D('',#31880,#15984,#15985);
#12817=AXIS2_PLACEMENT_3D('',#31899,#15986,#15987);
#12818=AXIS2_PLACEMENT_3D('',#31900,#15988,#15989);
#12819=AXIS2_PLACEMENT_3D('',#31901,#15990,#15991);
#12820=AXIS2_PLACEMENT_3D('',#31926,#15992,#15993);
#12821=AXIS2_PLACEMENT_3D('',#31927,#15994,#15995);
#12822=AXIS2_PLACEMENT_3D('',#31928,#15996,#15997);
#12823=AXIS2_PLACEMENT_3D('',#31929,#15998,#15999);
#12824=AXIS2_PLACEMENT_3D('',#31978,#16000,#16001);
#12825=AXIS2_PLACEMENT_3D('',#32043,#16002,#16003);
#12826=AXIS2_PLACEMENT_3D('',#32044,#16004,#16005);
#12827=AXIS2_PLACEMENT_3D('',#32045,#16006,#16007);
#12828=AXIS2_PLACEMENT_3D('',#32046,#16008,#16009);
#12829=AXIS2_PLACEMENT_3D('',#32047,#16010,#16011);
#12830=AXIS2_PLACEMENT_3D('',#32048,#16012,#16013);
#12831=AXIS2_PLACEMENT_3D('',#32049,#16014,#16015);
#12832=AXIS2_PLACEMENT_3D('',#32050,#16016,#16017);
#12833=AXIS2_PLACEMENT_3D('',#32051,#16018,#16019);
#12834=AXIS2_PLACEMENT_3D('',#32052,#16020,#16021);
#12835=AXIS2_PLACEMENT_3D('',#32053,#16022,#16023);
#12836=AXIS2_PLACEMENT_3D('',#32054,#16024,#16025);
#12837=AXIS2_PLACEMENT_3D('',#32055,#16026,#16027);
#12838=AXIS2_PLACEMENT_3D('',#32056,#16028,#16029);
#12839=AXIS2_PLACEMENT_3D('',#32057,#16030,#16031);
#12840=AXIS2_PLACEMENT_3D('',#32058,#16032,#16033);
#12841=AXIS2_PLACEMENT_3D('',#32059,#16034,#16035);
#12842=AXIS2_PLACEMENT_3D('',#32060,#16036,#16037);
#12843=AXIS2_PLACEMENT_3D('',#32061,#16038,#16039);
#12844=AXIS2_PLACEMENT_3D('',#32062,#16040,#16041);
#12845=AXIS2_PLACEMENT_3D('',#32063,#16042,#16043);
#12846=AXIS2_PLACEMENT_3D('',#32064,#16044,#16045);
#12847=AXIS2_PLACEMENT_3D('',#32065,#16046,#16047);
#12848=AXIS2_PLACEMENT_3D('',#32066,#16048,#16049);
#12849=AXIS2_PLACEMENT_3D('',#32067,#16050,#16051);
#12850=AXIS2_PLACEMENT_3D('',#32068,#16052,#16053);
#12851=AXIS2_PLACEMENT_3D('',#32069,#16054,#16055);
#12852=AXIS2_PLACEMENT_3D('',#32070,#16056,#16057);
#12853=AXIS2_PLACEMENT_3D('',#32071,#16058,#16059);
#12854=AXIS2_PLACEMENT_3D('',#32072,#16060,#16061);
#12855=AXIS2_PLACEMENT_3D('',#32073,#16062,#16063);
#12856=AXIS2_PLACEMENT_3D('',#32074,#16064,#16065);
#12857=AXIS2_PLACEMENT_3D('',#32075,#16066,#16067);
#12858=AXIS2_PLACEMENT_3D('',#32076,#16068,#16069);
#12859=AXIS2_PLACEMENT_3D('',#32077,#16070,#16071);
#12860=AXIS2_PLACEMENT_3D('',#32078,#16072,#16073);
#12861=AXIS2_PLACEMENT_3D('',#32079,#16074,#16075);
#12862=AXIS2_PLACEMENT_3D('',#32080,#16076,#16077);
#12863=AXIS2_PLACEMENT_3D('',#32081,#16078,#16079);
#12864=AXIS2_PLACEMENT_3D('',#32082,#16080,#16081);
#12865=AXIS2_PLACEMENT_3D('',#32083,#16082,#16083);
#12866=AXIS2_PLACEMENT_3D('',#32084,#16084,#16085);
#12867=AXIS2_PLACEMENT_3D('',#32085,#16086,#16087);
#12868=AXIS2_PLACEMENT_3D('',#32086,#16088,#16089);
#12869=AXIS2_PLACEMENT_3D('',#32087,#16090,#16091);
#12870=AXIS2_PLACEMENT_3D('',#32088,#16092,#16093);
#12871=AXIS2_PLACEMENT_3D('',#32089,#16094,#16095);
#12872=AXIS2_PLACEMENT_3D('',#32090,#16096,#16097);
#12873=AXIS2_PLACEMENT_3D('',#32091,#16098,#16099);
#12874=AXIS2_PLACEMENT_3D('',#32092,#16100,#16101);
#12875=AXIS2_PLACEMENT_3D('',#32093,#16102,#16103);
#12876=AXIS2_PLACEMENT_3D('',#32094,#16104,#16105);
#12877=AXIS2_PLACEMENT_3D('',#32095,#16106,#16107);
#12878=AXIS2_PLACEMENT_3D('',#32096,#16108,#16109);
#12879=AXIS2_PLACEMENT_3D('',#32097,#16110,#16111);
#12880=AXIS2_PLACEMENT_3D('',#32098,#16112,#16113);
#12881=AXIS2_PLACEMENT_3D('',#32099,#16114,#16115);
#12882=AXIS2_PLACEMENT_3D('',#32100,#16116,#16117);
#12883=AXIS2_PLACEMENT_3D('',#32101,#16118,#16119);
#12884=AXIS2_PLACEMENT_3D('',#32102,#16120,#16121);
#12885=AXIS2_PLACEMENT_3D('',#32103,#16122,#16123);
#12886=AXIS2_PLACEMENT_3D('',#32104,#16124,#16125);
#12887=AXIS2_PLACEMENT_3D('',#32105,#16126,#16127);
#12888=AXIS2_PLACEMENT_3D('',#32106,#16128,#16129);
#12889=AXIS2_PLACEMENT_3D('',#32107,#16130,#16131);
#12890=AXIS2_PLACEMENT_3D('',#32108,#16132,#16133);
#12891=AXIS2_PLACEMENT_3D('',#32109,#16134,#16135);
#12892=AXIS2_PLACEMENT_3D('',#32110,#16136,#16137);
#12893=AXIS2_PLACEMENT_3D('',#32111,#16138,#16139);
#12894=AXIS2_PLACEMENT_3D('',#32112,#16140,#16141);
#12895=AXIS2_PLACEMENT_3D('',#32113,#16142,#16143);
#12896=AXIS2_PLACEMENT_3D('',#32114,#16144,#16145);
#12897=AXIS2_PLACEMENT_3D('',#32115,#16146,#16147);
#12898=AXIS2_PLACEMENT_3D('',#32116,#16148,#16149);
#12899=AXIS2_PLACEMENT_3D('',#32117,#16150,#16151);
#12900=AXIS2_PLACEMENT_3D('',#32118,#16152,#16153);
#12901=AXIS2_PLACEMENT_3D('',#32119,#16154,#16155);
#12902=AXIS2_PLACEMENT_3D('',#32120,#16156,#16157);
#12903=AXIS2_PLACEMENT_3D('',#32121,#16158,#16159);
#12904=AXIS2_PLACEMENT_3D('',#32122,#16160,#16161);
#12905=AXIS2_PLACEMENT_3D('',#32123,#16162,#16163);
#12906=AXIS2_PLACEMENT_3D('',#32124,#16164,#16165);
#12907=AXIS2_PLACEMENT_3D('',#32125,#16166,#16167);
#12908=AXIS2_PLACEMENT_3D('',#32126,#16168,#16169);
#12909=AXIS2_PLACEMENT_3D('',#32127,#16170,#16171);
#12910=AXIS2_PLACEMENT_3D('',#32128,#16172,#16173);
#12911=AXIS2_PLACEMENT_3D('',#32129,#16174,#16175);
#12912=AXIS2_PLACEMENT_3D('',#32130,#16176,#16177);
#12913=AXIS2_PLACEMENT_3D('',#32131,#16178,#16179);
#12914=AXIS2_PLACEMENT_3D('',#32132,#16180,#16181);
#12915=AXIS2_PLACEMENT_3D('',#32133,#16182,#16183);
#12916=AXIS2_PLACEMENT_3D('',#32134,#16184,#16185);
#12917=AXIS2_PLACEMENT_3D('',#32135,#16186,#16187);
#12918=AXIS2_PLACEMENT_3D('',#32136,#16188,#16189);
#12919=AXIS2_PLACEMENT_3D('',#32137,#16190,#16191);
#12920=AXIS2_PLACEMENT_3D('',#32138,#16192,#16193);
#12921=AXIS2_PLACEMENT_3D('',#32139,#16194,#16195);
#12922=AXIS2_PLACEMENT_3D('',#32140,#16196,#16197);
#12923=AXIS2_PLACEMENT_3D('',#32141,#16198,#16199);
#12924=AXIS2_PLACEMENT_3D('',#32142,#16200,#16201);
#12925=AXIS2_PLACEMENT_3D('',#32143,#16202,#16203);
#12926=AXIS2_PLACEMENT_3D('',#32146,#16206,#16207);
#12927=AXIS2_PLACEMENT_3D('',#32149,#16210,#16211);
#12928=AXIS2_PLACEMENT_3D('',#32155,#16216,#16217);
#12929=AXIS2_PLACEMENT_3D('',#32156,#16218,#16219);
#12930=AXIS2_PLACEMENT_3D('',#32157,#16220,#16221);
#12931=AXIS2_PLACEMENT_3D('',#32158,#16222,#16223);
#12932=AXIS2_PLACEMENT_3D('',#32159,#16224,#16225);
#12933=AXIS2_PLACEMENT_3D('',#32163,#16228,#16229);
#12934=AXIS2_PLACEMENT_3D('',#32164,#16230,#16231);
#12935=AXIS2_PLACEMENT_3D('',#32167,#16234,#16235);
#12936=AXIS2_PLACEMENT_3D('',#32171,#16238,#16239);
#12937=AXIS2_PLACEMENT_3D('',#32173,#16241,#16242);
#12938=AXIS2_PLACEMENT_3D('',#32175,#16244,#16245);
#12939=AXIS2_PLACEMENT_3D('',#32177,#16247,#16248);
#12940=AXIS2_PLACEMENT_3D('',#32179,#16250,#16251);
#12941=AXIS2_PLACEMENT_3D('',#32180,#16252,#16253);
#12942=AXIS2_PLACEMENT_3D('',#32181,#16254,#16255);
#12943=AXIS2_PLACEMENT_3D('',#32183,#16257,#16258);
#12944=AXIS2_PLACEMENT_3D('',#32185,#16260,#16261);
#12945=AXIS2_PLACEMENT_3D('',#32187,#16263,#16264);
#12946=AXIS2_PLACEMENT_3D('',#32189,#16266,#16267);
#12947=AXIS2_PLACEMENT_3D('',#32191,#16269,#16270);
#12948=AXIS2_PLACEMENT_3D('',#32193,#16272,#16273);
#12949=AXIS2_PLACEMENT_3D('',#32194,#16274,#16275);
#12950=AXIS2_PLACEMENT_3D('',#32195,#16276,#16277);
#12951=AXIS2_PLACEMENT_3D('',#32196,#16278,#16279);
#12952=AXIS2_PLACEMENT_3D('',#32198,#16280,#16281);
#12953=AXIS2_PLACEMENT_3D('',#32213,#16283,#16284);
#12954=AXIS2_PLACEMENT_3D('',#32237,#16285,#16286);
#12955=AXIS2_PLACEMENT_3D('',#32261,#16287,#16288);
#12956=AXIS2_PLACEMENT_3D('',#32263,#16289,#16290);
#12957=AXIS2_PLACEMENT_3D('',#32287,#16291,#16292);
#12958=AXIS2_PLACEMENT_3D('',#32311,#16293,#16294);
#12959=AXIS2_PLACEMENT_3D('',#32335,#16295,#16296);
#12960=AXIS2_PLACEMENT_3D('',#32359,#16297,#16298);
#12961=AXIS2_PLACEMENT_3D('',#32371,#16300,#16301);
#12962=AXIS2_PLACEMENT_3D('',#32373,#16302,#16303);
#12963=AXIS2_PLACEMENT_3D('',#32375,#16304,#16305);
#12964=AXIS2_PLACEMENT_3D('',#32376,#16306,#16307);
#12965=AXIS2_PLACEMENT_3D('',#32377,#16308,#16309);
#12966=AXIS2_PLACEMENT_3D('',#32379,#16310,#16311);
#12967=AXIS2_PLACEMENT_3D('',#32382,#16313,#16314);
#12968=AXIS2_PLACEMENT_3D('',#32383,#16315,#16316);
#12969=AXIS2_PLACEMENT_3D('',#32385,#16317,#16318);
#12970=AXIS2_PLACEMENT_3D('',#32387,#16319,#16320);
#12971=AXIS2_PLACEMENT_3D('',#32388,#16321,#16322);
#12972=AXIS2_PLACEMENT_3D('',#32389,#16323,#16324);
#12973=AXIS2_PLACEMENT_3D('',#32392,#16326,#16327);
#12974=AXIS2_PLACEMENT_3D('',#32393,#16328,#16329);
#12975=AXIS2_PLACEMENT_3D('',#32416,#16331,#16332);
#12976=AXIS2_PLACEMENT_3D('',#32418,#16333,#16334);
#12977=AXIS2_PLACEMENT_3D('',#32419,#16335,#16336);
#12978=AXIS2_PLACEMENT_3D('',#32514,#16337,#16338);
#12979=AXIS2_PLACEMENT_3D('',#32639,#16339,#16340);
#12980=AXIS2_PLACEMENT_3D('',#37605,#16347,#16348);
#12981=AXIS2_PLACEMENT_3D('',#37606,#16349,#16350);
#12982=AXIS2_PLACEMENT_3D('',#37607,#16351,#16352);
#12983=AXIS2_PLACEMENT_3D('',#37608,#16353,#16354);
#12984=AXIS2_PLACEMENT_3D('',#37609,#16355,#16356);
#12985=AXIS2_PLACEMENT_3D('',#37610,#16357,#16358);
#12986=AXIS2_PLACEMENT_3D('',#37611,#16359,#16360);
#12987=AXIS2_PLACEMENT_3D('',#37612,#16361,#16362);
#12988=AXIS2_PLACEMENT_3D('',#37613,#16363,#16364);
#12989=AXIS2_PLACEMENT_3D('',#37614,#16365,#16366);
#12990=AXIS2_PLACEMENT_3D('',#37615,#16367,#16368);
#12991=AXIS2_PLACEMENT_3D('',#37616,#16369,#16370);
#12992=AXIS2_PLACEMENT_3D('',#37617,#16371,#16372);
#12993=DIRECTION('axis',(0.,0.,1.));
#12994=DIRECTION('refdir',(1.,0.,0.));
#12995=DIRECTION('axis',(0.,0.,1.));
#12996=DIRECTION('refdir',(1.,0.,0.));
#12997=DIRECTION('center_axis',(0.,1.,0.));
#12998=DIRECTION('ref_axis',(0.,0.,1.));
#12999=DIRECTION('center_axis',(0.,1.,0.));
#13000=DIRECTION('ref_axis',(0.,0.,1.));
#13001=DIRECTION('',(0.,1.,0.));
#13002=DIRECTION('center_axis',(0.,1.,0.));
#13003=DIRECTION('ref_axis',(1.,0.,0.));
#13004=DIRECTION('center_axis',(0.,1.,0.));
#13005=DIRECTION('ref_axis',(0.,0.,1.));
#13006=DIRECTION('center_axis',(0.,1.,0.));
#13007=DIRECTION('ref_axis',(0.,0.,1.));
#13008=DIRECTION('',(0.,1.,0.));
#13009=DIRECTION('center_axis',(0.,1.,0.));
#13010=DIRECTION('ref_axis',(0.,0.,1.));
#13011=DIRECTION('center_axis',(0.,1.,0.));
#13012=DIRECTION('ref_axis',(0.,0.,1.));
#13013=DIRECTION('center_axis',(0.,1.,0.));
#13014=DIRECTION('ref_axis',(1.,0.,0.));
#13015=DIRECTION('',(0.,-1.,0.));
#13016=DIRECTION('center_axis',(0.,1.,0.));
#13017=DIRECTION('ref_axis',(0.,0.,1.));
#13018=DIRECTION('center_axis',(0.,1.,0.));
#13019=DIRECTION('ref_axis',(0.,0.,1.));
#13020=DIRECTION('center_axis',(0.,1.,0.));
#13021=DIRECTION('ref_axis',(0.,0.,1.));
#13022=DIRECTION('',(0.,1.,0.));
#13023=DIRECTION('center_axis',(0.,1.,0.));
#13024=DIRECTION('ref_axis',(0.,0.,1.));
#13025=DIRECTION('center_axis',(0.,1.,0.));
#13026=DIRECTION('ref_axis',(0.,0.,1.));
#13027=DIRECTION('center_axis',(0.,1.,0.));
#13028=DIRECTION('ref_axis',(0.,0.,1.));
#13029=DIRECTION('center_axis',(0.,1.,0.));
#13030=DIRECTION('ref_axis',(0.,0.,1.));
#13031=DIRECTION('center_axis',(-1.,0.,0.));
#13032=DIRECTION('ref_axis',(0.,0.,-1.));
#13033=DIRECTION('center_axis',(0.,-1.,0.));
#13034=DIRECTION('ref_axis',(0.,0.,1.));
#13035=DIRECTION('center_axis',(0.,1.,0.));
#13036=DIRECTION('ref_axis',(0.,0.,1.));
#13037=DIRECTION('center_axis',(0.,1.,0.));
#13038=DIRECTION('ref_axis',(0.,0.,1.));
#13039=DIRECTION('center_axis',(-1.,0.,0.));
#13040=DIRECTION('ref_axis',(0.,0.,-1.));
#13041=DIRECTION('center_axis',(0.,-1.,0.));
#13042=DIRECTION('ref_axis',(0.,0.,1.));
#13043=DIRECTION('center_axis',(0.,-1.,0.));
#13044=DIRECTION('ref_axis',(0.,0.,1.));
#13045=DIRECTION('center_axis',(0.,-1.,0.));
#13046=DIRECTION('ref_axis',(0.,0.,-1.));
#13047=DIRECTION('center_axis',(0.,-1.,0.));
#13048=DIRECTION('ref_axis',(0.,0.,-1.));
#13049=DIRECTION('center_axis',(-1.,0.,0.));
#13050=DIRECTION('ref_axis',(0.,0.,1.));
#13051=DIRECTION('center_axis',(0.,1.,0.));
#13052=DIRECTION('ref_axis',(0.,0.,-1.));
#13053=DIRECTION('center_axis',(0.,1.,0.));
#13054=DIRECTION('ref_axis',(0.,0.,1.));
#13055=DIRECTION('center_axis',(0.,1.,0.));
#13056=DIRECTION('ref_axis',(0.,0.,1.));
#13057=DIRECTION('center_axis',(-1.,0.,0.));
#13058=DIRECTION('ref_axis',(0.,0.,-1.));
#13059=DIRECTION('center_axis',(0.,-1.,0.));
#13060=DIRECTION('ref_axis',(0.,0.,1.));
#13061=DIRECTION('center_axis',(0.,-1.,0.));
#13062=DIRECTION('ref_axis',(0.,0.,1.));
#13063=DIRECTION('center_axis',(0.,1.,0.));
#13064=DIRECTION('ref_axis',(0.,0.,1.));
#13065=DIRECTION('center_axis',(0.,1.,0.));
#13066=DIRECTION('ref_axis',(0.,0.,1.));
#13067=DIRECTION('center_axis',(0.,0.,-1.));
#13068=DIRECTION('ref_axis',(-1.,0.,0.));
#13069=DIRECTION('center_axis',(0.,-1.,0.));
#13070=DIRECTION('ref_axis',(-7.40148683083437E-15,0.,1.));
#13071=DIRECTION('center_axis',(-0.528132444354927,0.,0.849162011173186));
#13072=DIRECTION('ref_axis',(0.849162011173186,0.,0.528132444354927));
#13073=DIRECTION('center_axis',(0.,1.,0.));
#13074=DIRECTION('ref_axis',(0.,0.,1.));
#13075=DIRECTION('center_axis',(0.,1.,0.));
#13076=DIRECTION('ref_axis',(0.,0.,1.));
#13077=DIRECTION('center_axis',(0.808689828521621,0.,0.588235294117645));
#13078=DIRECTION('ref_axis',(0.588235294117644,0.,-0.808689828521621));
#13079=DIRECTION('center_axis',(0.,-1.,0.));
#13080=DIRECTION('ref_axis',(0.,0.,1.));
#13081=DIRECTION('center_axis',(0.588235294117645,0.,0.808689828521621));
#13082=DIRECTION('ref_axis',(0.808689828521621,0.,-0.588235294117644));
#13083=DIRECTION('center_axis',(0.,1.,0.));
#13084=DIRECTION('ref_axis',(0.,0.,1.));
#13085=DIRECTION('center_axis',(0.,-1.,0.));
#13086=DIRECTION('ref_axis',(0.,0.,1.));
#13087=DIRECTION('center_axis',(0.528132444354927,1.46586199943601E-14,
-0.849162011173186));
#13088=DIRECTION('ref_axis',(-0.849162011173186,-1.56277058526093E-29,-0.528132444354927));
#13089=DIRECTION('center_axis',(0.,1.,0.));
#13090=DIRECTION('ref_axis',(0.,0.,1.));
#13091=DIRECTION('center_axis',(0.,0.,1.));
#13092=DIRECTION('ref_axis',(1.,0.,0.));
#13093=DIRECTION('center_axis',(0.,1.,0.));
#13094=DIRECTION('ref_axis',(0.,0.,1.));
#13095=DIRECTION('center_axis',(0.,-1.,0.));
#13096=DIRECTION('ref_axis',(0.,0.,1.));
#13097=DIRECTION('center_axis',(-0.588235294117631,0.,-0.80868982852163));
#13098=DIRECTION('ref_axis',(-0.80868982852163,0.,0.588235294117631));
#13099=DIRECTION('center_axis',(0.,1.,0.));
#13100=DIRECTION('ref_axis',(0.,0.,1.));
#13101=DIRECTION('center_axis',(-0.808689828521621,0.,-0.588235294117645));
#13102=DIRECTION('ref_axis',(-0.588235294117644,0.,0.808689828521621));
#13103=DIRECTION('center_axis',(0.,1.,0.));
#13104=DIRECTION('ref_axis',(0.,0.,1.));
#13105=DIRECTION('center_axis',(0.,1.,0.));
#13106=DIRECTION('ref_axis',(0.,0.,1.));
#13107=DIRECTION('center_axis',(0.,1.,0.));
#13108=DIRECTION('ref_axis',(0.,0.,1.));
#13109=DIRECTION('center_axis',(-1.,0.,0.));
#13110=DIRECTION('ref_axis',(0.,0.,-1.));
#13111=DIRECTION('center_axis',(0.,-1.,0.));
#13112=DIRECTION('ref_axis',(0.,0.,1.));
#13113=DIRECTION('center_axis',(0.,1.,0.));
#13114=DIRECTION('ref_axis',(0.,0.,1.));
#13115=DIRECTION('center_axis',(0.,1.,0.));
#13116=DIRECTION('ref_axis',(0.,0.,1.));
#13117=DIRECTION('center_axis',(-1.,0.,0.));
#13118=DIRECTION('ref_axis',(0.,0.,-1.));
#13119=DIRECTION('center_axis',(0.,-1.,0.));
#13120=DIRECTION('ref_axis',(0.,0.,1.));
#13121=DIRECTION('center_axis',(0.,-1.,0.));
#13122=DIRECTION('ref_axis',(0.,0.,1.));
#13123=DIRECTION('center_axis',(0.,-1.,0.));
#13124=DIRECTION('ref_axis',(0.,0.,-1.));
#13125=DIRECTION('center_axis',(0.,-1.,0.));
#13126=DIRECTION('ref_axis',(0.,0.,-1.));
#13127=DIRECTION('center_axis',(-1.,0.,0.));
#13128=DIRECTION('ref_axis',(0.,0.,1.));
#13129=DIRECTION('center_axis',(0.,1.,0.));
#13130=DIRECTION('ref_axis',(0.,0.,-1.));
#13131=DIRECTION('center_axis',(0.,1.,0.));
#13132=DIRECTION('ref_axis',(0.,0.,-1.));
#13133=DIRECTION('center_axis',(0.,1.,0.));
#13134=DIRECTION('ref_axis',(0.,0.,1.));
#13135=DIRECTION('center_axis',(0.,1.,0.));
#13136=DIRECTION('ref_axis',(0.,0.,1.));
#13137=DIRECTION('center_axis',(-1.,0.,0.));
#13138=DIRECTION('ref_axis',(0.,0.,-1.));
#13139=DIRECTION('center_axis',(0.,-1.,0.));
#13140=DIRECTION('ref_axis',(0.,0.,1.));
#13141=DIRECTION('center_axis',(0.,-1.,0.));
#13142=DIRECTION('ref_axis',(0.,0.,1.));
#13143=DIRECTION('center_axis',(0.,1.,0.));
#13144=DIRECTION('ref_axis',(0.,0.,1.));
#13145=DIRECTION('center_axis',(0.,1.,0.));
#13146=DIRECTION('ref_axis',(0.,0.,1.));
#13147=DIRECTION('center_axis',(0.528132444354927,0.,0.849162011173186));
#13148=DIRECTION('ref_axis',(0.849162011173186,0.,-0.528132444354927));
#13149=DIRECTION('center_axis',(0.,-1.,0.));
#13150=DIRECTION('ref_axis',(0.,0.,1.));
#13151=DIRECTION('center_axis',(0.,0.,-1.));
#13152=DIRECTION('ref_axis',(-1.,0.,0.));
#13153=DIRECTION('center_axis',(0.,1.,0.));
#13154=DIRECTION('ref_axis',(0.,0.,1.));
#13155=DIRECTION('center_axis',(0.,1.,0.));
#13156=DIRECTION('ref_axis',(0.,0.,1.));
#13157=DIRECTION('center_axis',(-0.588235294117645,0.,0.808689828521621));
#13158=DIRECTION('ref_axis',(0.808689828521621,0.,0.588235294117644));
#13159=DIRECTION('center_axis',(0.,-1.,0.));
#13160=DIRECTION('ref_axis',(-1.48029736616688E-15,0.,1.));
#13161=DIRECTION('center_axis',(-0.808689828521621,0.,0.588235294117645));
#13162=DIRECTION('ref_axis',(0.588235294117644,0.,0.808689828521621));
#13163=DIRECTION('center_axis',(0.,1.,0.));
#13164=DIRECTION('ref_axis',(0.,0.,1.));
#13165=DIRECTION('center_axis',(0.,-1.,0.));
#13166=DIRECTION('ref_axis',(0.,0.,1.));
#13167=DIRECTION('center_axis',(0.,0.,1.));
#13168=DIRECTION('ref_axis',(1.,0.,0.));
#13169=DIRECTION('center_axis',(0.,1.,0.));
#13170=DIRECTION('ref_axis',(0.,0.,1.));
#13171=DIRECTION('center_axis',(-0.528132444354927,0.,-0.849162011173186));
#13172=DIRECTION('ref_axis',(-0.849162011173186,0.,0.528132444354927));
#13173=DIRECTION('center_axis',(0.,1.,0.));
#13174=DIRECTION('ref_axis',(0.,0.,1.));
#13175=DIRECTION('center_axis',(0.,-1.,0.));
#13176=DIRECTION('ref_axis',(0.,0.,1.));
#13177=DIRECTION('center_axis',(0.808689828521621,0.,-0.588235294117645));
#13178=DIRECTION('ref_axis',(-0.588235294117644,0.,-0.808689828521621));
#13179=DIRECTION('center_axis',(0.,1.,0.));
#13180=DIRECTION('ref_axis',(0.,0.,1.));
#13181=DIRECTION('center_axis',(0.588235294117645,0.,-0.808689828521621));
#13182=DIRECTION('ref_axis',(-0.808689828521621,0.,-0.588235294117644));
#13183=DIRECTION('center_axis',(0.,1.,0.));
#13184=DIRECTION('ref_axis',(0.,0.,1.));
#13185=DIRECTION('center_axis',(0.,1.,0.));
#13186=DIRECTION('ref_axis',(0.,0.,1.));
#13187=DIRECTION('center_axis',(-1.,0.,0.));
#13188=DIRECTION('ref_axis',(0.,0.,-1.));
#13189=DIRECTION('center_axis',(0.,-1.,0.));
#13190=DIRECTION('ref_axis',(0.,0.,1.));
#13191=DIRECTION('center_axis',(0.,1.,0.));
#13192=DIRECTION('ref_axis',(0.,0.,1.));
#13193=DIRECTION('center_axis',(0.,1.,0.));
#13194=DIRECTION('ref_axis',(0.,0.,1.));
#13195=DIRECTION('center_axis',(-1.,0.,0.));
#13196=DIRECTION('ref_axis',(0.,0.,-1.));
#13197=DIRECTION('center_axis',(0.,-1.,0.));
#13198=DIRECTION('ref_axis',(0.,0.,1.));
#13199=DIRECTION('center_axis',(0.,-1.,0.));
#13200=DIRECTION('ref_axis',(0.,0.,-1.));
#13201=DIRECTION('center_axis',(0.,-1.,0.));
#13202=DIRECTION('ref_axis',(0.,0.,-1.));
#13203=DIRECTION('center_axis',(-1.,0.,0.));
#13204=DIRECTION('ref_axis',(0.,0.,1.));
#13205=DIRECTION('center_axis',(0.,1.,0.));
#13206=DIRECTION('ref_axis',(0.,0.,-1.));
#13207=DIRECTION('center_axis',(0.,1.,0.));
#13208=DIRECTION('ref_axis',(0.,0.,-1.));
#13209=DIRECTION('center_axis',(0.,1.,0.));
#13210=DIRECTION('ref_axis',(0.,0.,1.));
#13211=DIRECTION('center_axis',(0.,1.,0.));
#13212=DIRECTION('ref_axis',(0.,0.,1.));
#13213=DIRECTION('center_axis',(-1.,0.,0.));
#13214=DIRECTION('ref_axis',(0.,0.,-1.));
#13215=DIRECTION('center_axis',(0.,-1.,0.));
#13216=DIRECTION('ref_axis',(0.,0.,1.));
#13217=DIRECTION('center_axis',(0.,1.,0.));
#13218=DIRECTION('ref_axis',(0.,0.,1.));
#13219=DIRECTION('center_axis',(0.,1.,0.));
#13220=DIRECTION('ref_axis',(0.,0.,1.));
#13221=DIRECTION('center_axis',(-0.808689828521621,0.,-0.588235294117645));
#13222=DIRECTION('ref_axis',(-0.588235294117644,0.,0.808689828521621));
#13223=DIRECTION('center_axis',(0.,-1.,0.));
#13224=DIRECTION('ref_axis',(0.,0.,1.));
#13225=DIRECTION('center_axis',(0.,0.,1.));
#13226=DIRECTION('ref_axis',(1.,0.,0.));
#13227=DIRECTION('center_axis',(0.,1.,0.));
#13228=DIRECTION('ref_axis',(0.,0.,1.));
#13229=DIRECTION('center_axis',(0.,-1.,0.));
#13230=DIRECTION('ref_axis',(0.,0.,1.));
#13231=DIRECTION('center_axis',(0.,0.,-1.));
#13232=DIRECTION('ref_axis',(-1.,0.,0.));
#13233=DIRECTION('center_axis',(0.,1.,0.));
#13234=DIRECTION('ref_axis',(0.,0.,1.));
#13235=DIRECTION('center_axis',(0.808689828521621,0.,0.588235294117645));
#13236=DIRECTION('ref_axis',(0.588235294117644,0.,-0.808689828521621));
#13237=DIRECTION('center_axis',(0.,1.,0.));
#13238=DIRECTION('ref_axis',(0.,0.,1.));
#13239=DIRECTION('center_axis',(0.,1.,0.));
#13240=DIRECTION('ref_axis',(0.,0.,1.));
#13241=DIRECTION('center_axis',(-1.,0.,0.));
#13242=DIRECTION('ref_axis',(0.,0.,-1.));
#13243=DIRECTION('center_axis',(0.,-1.,0.));
#13244=DIRECTION('ref_axis',(0.,0.,1.));
#13245=DIRECTION('center_axis',(0.,1.,0.));
#13246=DIRECTION('ref_axis',(0.,0.,1.));
#13247=DIRECTION('center_axis',(0.,1.,0.));
#13248=DIRECTION('ref_axis',(0.,0.,1.));
#13249=DIRECTION('center_axis',(0.,1.,0.));
#13250=DIRECTION('ref_axis',(0.,0.,1.));
#13251=DIRECTION('center_axis',(-1.,0.,0.));
#13252=DIRECTION('ref_axis',(0.,0.,-1.));
#13253=DIRECTION('center_axis',(0.,-1.,0.));
#13254=DIRECTION('ref_axis',(0.,0.,1.));
#13255=DIRECTION('center_axis',(0.,-1.,0.));
#13256=DIRECTION('ref_axis',(0.,0.,1.));
#13257=DIRECTION('center_axis',(0.,-1.,0.));
#13258=DIRECTION('ref_axis',(0.,0.,-1.));
#13259=DIRECTION('center_axis',(0.,-1.,0.));
#13260=DIRECTION('ref_axis',(0.,0.,-1.));
#13261=DIRECTION('center_axis',(-1.,0.,0.));
#13262=DIRECTION('ref_axis',(0.,0.,1.));
#13263=DIRECTION('center_axis',(0.,1.,0.));
#13264=DIRECTION('ref_axis',(0.,0.,-1.));
#13265=DIRECTION('center_axis',(0.,1.,0.));
#13266=DIRECTION('ref_axis',(0.,0.,-1.));
#13267=DIRECTION('center_axis',(0.,1.,0.));
#13268=DIRECTION('ref_axis',(0.,0.,1.));
#13269=DIRECTION('center_axis',(0.,1.,0.));
#13270=DIRECTION('ref_axis',(0.,0.,1.));
#13271=DIRECTION('center_axis',(-1.,0.,0.));
#13272=DIRECTION('ref_axis',(0.,0.,-1.));
#13273=DIRECTION('center_axis',(0.,-1.,0.));
#13274=DIRECTION('ref_axis',(0.,0.,1.));
#13275=DIRECTION('center_axis',(0.,-1.,0.));
#13276=DIRECTION('ref_axis',(0.,0.,1.));
#13277=DIRECTION('center_axis',(0.,1.,0.));
#13278=DIRECTION('ref_axis',(0.,0.,1.));
#13279=DIRECTION('center_axis',(0.,1.,0.));
#13280=DIRECTION('ref_axis',(0.,0.,1.));
#13281=DIRECTION('center_axis',(0.724563445309589,-1.0182026595163E-14,
0.68920810625028));
#13282=DIRECTION('ref_axis',(0.689208106250281,9.56120314610186E-29,-0.724563445309589));
#13283=DIRECTION('center_axis',(0.,-1.,0.));
#13284=DIRECTION('ref_axis',(0.,0.,-1.));
#13285=DIRECTION('center_axis',(0.724563445309596,-1.34013438274573E-14,
-0.689208106250273));
#13286=DIRECTION('ref_axis',(0.689208106250273,-2.63677968348471E-14,0.724563445309596));
#13287=DIRECTION('center_axis',(0.,1.,0.));
#13288=DIRECTION('ref_axis',(0.,0.,1.));
#13289=DIRECTION('center_axis',(0.,1.,0.));
#13290=DIRECTION('ref_axis',(0.,0.,1.));
#13291=DIRECTION('center_axis',(0.724563445309589,1.0182026595163E-14,0.68920810625028));
#13292=DIRECTION('ref_axis',(0.68920810625028,-9.81293834229342E-29,-0.724563445309589));
#13293=DIRECTION('center_axis',(0.,-1.,0.));
#13294=DIRECTION('ref_axis',(-2.66454616931092E-15,0.,1.));
#13295=DIRECTION('center_axis',(0.724563445309603,9.43334816904809E-15,
-0.689208106250266));
#13296=DIRECTION('ref_axis',(0.689208106250266,-3.33066907387548E-14,0.724563445309603));
#13297=DIRECTION('center_axis',(0.,1.,0.));
#13298=DIRECTION('ref_axis',(0.,0.,1.));
#13299=DIRECTION('center_axis',(0.,1.,0.));
#13300=DIRECTION('ref_axis',(0.,0.,1.));
#13301=DIRECTION('center_axis',(0.707106781186548,0.,-0.707106781186548));
#13302=DIRECTION('ref_axis',(-0.707106781186548,0.,-0.707106781186548));
#13303=DIRECTION('center_axis',(0.,-1.,0.));
#13304=DIRECTION('ref_axis',(0.,0.,1.));
#13305=DIRECTION('center_axis',(-0.707106781186541,0.,0.707106781186554));
#13306=DIRECTION('ref_axis',(0.707106781186555,0.,0.707106781186541));
#13307=DIRECTION('center_axis',(0.,1.,0.));
#13308=DIRECTION('ref_axis',(0.,0.,1.));
#13309=DIRECTION('center_axis',(0.,1.,0.));
#13310=DIRECTION('ref_axis',(0.,0.,1.));
#13311=DIRECTION('center_axis',(0.707106781186548,9.81307786677359E-15,
0.707106781186548));
#13312=DIRECTION('ref_axis',(0.707106781186548,3.73353565333889E-32,-0.707106781186548));
#13313=DIRECTION('center_axis',(0.,-1.,0.));
#13314=DIRECTION('ref_axis',(0.,0.,1.));
#13315=DIRECTION('center_axis',(-0.707106781186548,9.81307786677359E-15,
-0.707106781186548));
#13316=DIRECTION('ref_axis',(-0.707106781186548,3.73353565333889E-32,0.707106781186548));
#13317=DIRECTION('center_axis',(0.,-1.,0.));
#13318=DIRECTION('ref_axis',(0.,0.,-1.));
#13319=DIRECTION('center_axis',(0.,-1.,0.));
#13320=DIRECTION('ref_axis',(0.,0.,-1.));
#13321=DIRECTION('center_axis',(-0.707106781186548,-9.81307786677366E-15,
-0.707106781186548));
#13322=DIRECTION('ref_axis',(-0.707106781186548,-1.63063665584286E-31,0.707106781186548));
#13323=DIRECTION('center_axis',(0.,1.,0.));
#13324=DIRECTION('ref_axis',(0.,0.,-1.));
#13325=DIRECTION('center_axis',(0.707106781186548,-9.81307786677359E-15,
0.707106781186548));
#13326=DIRECTION('ref_axis',(0.707106781186548,-3.73353565333889E-32,-0.707106781186548));
#13327=DIRECTION('center_axis',(0.,-1.,0.));
#13328=DIRECTION('ref_axis',(0.,0.,-1.));
#13329=DIRECTION('center_axis',(0.,-1.,0.));
#13330=DIRECTION('ref_axis',(0.,0.,-1.));
#13331=DIRECTION('center_axis',(-0.707106781186548,0.,0.707106781186548));
#13332=DIRECTION('ref_axis',(0.707106781186548,0.,0.707106781186548));
#13333=DIRECTION('center_axis',(0.,1.,0.));
#13334=DIRECTION('ref_axis',(0.,0.,-1.));
#13335=DIRECTION('center_axis',(0.707106781186534,0.,-0.707106781186561));
#13336=DIRECTION('ref_axis',(-0.707106781186561,0.,-0.707106781186534));
#13337=DIRECTION('center_axis',(0.,1.,0.));
#13338=DIRECTION('ref_axis',(0.,0.,1.));
#13339=DIRECTION('center_axis',(-1.47242188377274E-14,1.,-1.47242188377274E-14));
#13340=DIRECTION('ref_axis',(7.97092275109852E-30,1.47242188377274E-14,
1.));
#13341=DIRECTION('',(0.,-1.,0.));
#13342=DIRECTION('center_axis',(2.01169630281381E-14,1.,-1.91353484389564E-14));
#13343=DIRECTION('ref_axis',(1.,-2.01169630281381E-14,-3.99449913460622E-29));
#13344=DIRECTION('',(0.,1.,0.));
#13345=DIRECTION('center_axis',(0.,1.,0.));
#13346=DIRECTION('ref_axis',(0.,0.,1.));
#13347=DIRECTION('center_axis',(1.50877222711036E-14,1.,1.43515113292173E-14));
#13348=DIRECTION('ref_axis',(-1.,1.50877222711036E-14,-2.55233473732763E-30));
#13349=DIRECTION('',(0.,-1.,0.));
#13350=DIRECTION('center_axis',(-1.9632291783637E-14,1.,1.9632291783637E-14));
#13351=DIRECTION('ref_axis',(5.04975666092008E-29,1.9632291783637E-14,-1.));
#13352=DIRECTION('',(0.,1.,0.));
#13353=DIRECTION('center_axis',(0.,-1.,0.));
#13354=DIRECTION('ref_axis',(0.,0.,-1.));
#13355=DIRECTION('center_axis',(0.,1.,0.));
#13356=DIRECTION('ref_axis',(0.,0.,-1.));
#13357=DIRECTION('',(0.,1.,0.));
#13358=DIRECTION('center_axis',(0.,1.,0.));
#13359=DIRECTION('ref_axis',(0.,0.,1.));
#13360=DIRECTION('',(0.,-1.,0.));
#13361=DIRECTION('center_axis',(0.,-1.,0.));
#13362=DIRECTION('ref_axis',(0.,0.,-1.));
#13363=DIRECTION('center_axis',(-0.456384763068618,0.,-0.8897825285084));
#13364=DIRECTION('ref_axis',(-0.8897825285084,0.,0.456384763068618));
#13365=DIRECTION('center_axis',(0.,-1.,0.));
#13366=DIRECTION('ref_axis',(0.,0.,-1.));
#13367=DIRECTION('center_axis',(-0.313163806483749,0.,0.949699126201877));
#13368=DIRECTION('ref_axis',(-0.949699126201877,0.,-0.313163806483749));
#13369=DIRECTION('center_axis',(0.,-1.,0.));
#13370=DIRECTION('ref_axis',(0.,0.,-1.));
#13371=DIRECTION('center_axis',(0.,-1.,0.));
#13372=DIRECTION('ref_axis',(2.22044604925031E-14,0.,1.));
#13373=DIRECTION('',(0.,1.,0.));
#13374=DIRECTION('center_axis',(0.,-1.,0.));
#13375=DIRECTION('ref_axis',(0.,0.,-1.));
#13376=DIRECTION('',(0.,-1.,0.));
#13377=DIRECTION('center_axis',(0.,-1.,0.));
#13378=DIRECTION('ref_axis',(0.,0.,-1.));
#13379=DIRECTION('center_axis',(0.,-1.,0.));
#13380=DIRECTION('ref_axis',(0.,0.,-1.));
#13381=DIRECTION('',(0.,1.,0.));
#13382=DIRECTION('center_axis',(0.,-1.,0.));
#13383=DIRECTION('ref_axis',(2.22044604925031E-14,0.,1.));
#13384=DIRECTION('',(0.,-1.,0.));
#13385=DIRECTION('center_axis',(0.,-1.,0.));
#13386=DIRECTION('ref_axis',(0.,0.,-1.));
#13387=DIRECTION('center_axis',(0.,-1.,0.));
#13388=DIRECTION('ref_axis',(0.,0.,1.));
#13389=DIRECTION('',(0.,1.,0.));
#13390=DIRECTION('center_axis',(0.,-1.,0.));
#13391=DIRECTION('ref_axis',(0.,0.,-1.));
#13392=DIRECTION('',(0.,-1.,0.));
#13393=DIRECTION('center_axis',(0.,-1.,0.));
#13394=DIRECTION('ref_axis',(0.,0.,-1.));
#13395=DIRECTION('center_axis',(0.,-1.,0.));
#13396=DIRECTION('ref_axis',(0.,0.,-1.));
#13397=DIRECTION('',(0.,1.,0.));
#13398=DIRECTION('center_axis',(0.,-1.,0.));
#13399=DIRECTION('ref_axis',(0.,0.,1.));
#13400=DIRECTION('',(0.,-1.,0.));
#13401=DIRECTION('center_axis',(0.,1.,0.));
#13402=DIRECTION('ref_axis',(0.,0.,1.));
#13403=DIRECTION('center_axis',(0.,-1.,0.));
#13404=DIRECTION('ref_axis',(0.,0.,1.));
#13405=DIRECTION('center_axis',(-0.313163806483745,0.,0.949699126201878));
#13406=DIRECTION('ref_axis',(0.949699126201878,0.,0.313163806483745));
#13407=DIRECTION('center_axis',(0.,1.,0.));
#13408=DIRECTION('ref_axis',(0.,0.,1.));
#13409=DIRECTION('center_axis',(0.456384763068627,0.,0.889782528508396));
#13410=DIRECTION('ref_axis',(0.889782528508395,0.,-0.456384763068626));
#13411=DIRECTION('center_axis',(0.,1.,0.));
#13412=DIRECTION('ref_axis',(0.,0.,1.));
#13413=DIRECTION('center_axis',(0.,1.,0.));
#13414=DIRECTION('ref_axis',(0.,0.,1.));
#13415=DIRECTION('center_axis',(0.,0.,1.));
#13416=DIRECTION('ref_axis',(1.,0.,0.));
#13417=DIRECTION('center_axis',(0.,-1.,0.));
#13418=DIRECTION('ref_axis',(-1.48029736616687E-14,0.,1.));
#13419=DIRECTION('center_axis',(0.808689828521621,0.,-0.588235294117645));
#13420=DIRECTION('ref_axis',(-0.588235294117644,0.,-0.808689828521621));
#13421=DIRECTION('center_axis',(0.,1.,0.));
#13422=DIRECTION('ref_axis',(0.,0.,1.));
#13423=DIRECTION('center_axis',(0.,-1.,0.));
#13424=DIRECTION('ref_axis',(0.,0.,1.));
#13425=DIRECTION('center_axis',(-0.808689828521621,0.,0.588235294117645));
#13426=DIRECTION('ref_axis',(0.588235294117644,0.,0.808689828521621));
#13427=DIRECTION('center_axis',(0.,1.,0.));
#13428=DIRECTION('ref_axis',(0.,0.,1.));
#13429=DIRECTION('center_axis',(0.,0.,-1.));
#13430=DIRECTION('ref_axis',(-1.,0.,0.));
#13431=DIRECTION('center_axis',(0.,1.,0.));
#13432=DIRECTION('ref_axis',(1.,0.,7.40148683083437E-15));
#13433=DIRECTION('center_axis',(0.,-1.,0.));
#13434=DIRECTION('ref_axis',(0.,0.,1.));
#13435=DIRECTION('',(0.,-1.,0.));
#13436=DIRECTION('center_axis',(0.,1.,0.));
#13437=DIRECTION('ref_axis',(0.,0.,1.));
#13438=DIRECTION('',(0.,1.,0.));
#13439=DIRECTION('center_axis',(0.,1.,0.));
#13440=DIRECTION('ref_axis',(1.,0.,1.11022302462516E-14));
#13441=DIRECTION('center_axis',(0.,1.,0.));
#13442=DIRECTION('ref_axis',(0.,0.,1.));
#13443=DIRECTION('',(0.,1.,0.));
#13444=DIRECTION('center_axis',(0.,-1.,0.));
#13445=DIRECTION('ref_axis',(-3.1720657846433E-15,0.,1.));
#13446=DIRECTION('',(0.,-1.,0.));
#13447=DIRECTION('center_axis',(0.,-1.,0.));
#13448=DIRECTION('ref_axis',(-1.,0.,-9.86864910777916E-15));
#13449=DIRECTION('',(0.,-1.,0.));
#13450=DIRECTION('center_axis',(0.,-1.,0.));
#13451=DIRECTION('ref_axis',(-1.,0.,-9.86864910777916E-15));
#13452=DIRECTION('',(0.,-1.,0.));
#13453=DIRECTION('center_axis',(0.,-1.,0.));
#13454=DIRECTION('ref_axis',(-1.,0.,-7.40148683083437E-15));
#13455=DIRECTION('',(0.,1.,0.));
#13456=DIRECTION('center_axis',(0.,1.,0.));
#13457=DIRECTION('ref_axis',(0.,0.,-1.));
#13458=DIRECTION('',(0.,-1.,0.));
#13459=DIRECTION('center_axis',(0.,1.,0.));
#13460=DIRECTION('ref_axis',(0.,0.,-1.));
#13461=DIRECTION('center_axis',(0.,-1.,0.));
#13462=DIRECTION('ref_axis',(0.,0.,1.));
#13463=DIRECTION('',(0.,-1.,0.));
#13464=DIRECTION('center_axis',(0.,1.,0.));
#13465=DIRECTION('ref_axis',(0.,0.,1.));
#13466=DIRECTION('',(0.,1.,0.));
#13467=DIRECTION('center_axis',(0.,1.,0.));
#13468=DIRECTION('ref_axis',(0.,0.,-1.));
#13469=DIRECTION('center_axis',(0.,1.,0.));
#13470=DIRECTION('ref_axis',(0.,0.,1.));
#13471=DIRECTION('',(0.,1.,0.));
#13472=DIRECTION('center_axis',(0.,-1.,0.));
#13473=DIRECTION('ref_axis',(0.,0.,1.));
#13474=DIRECTION('',(0.,-1.,0.));
#13475=DIRECTION('center_axis',(0.,-1.,0.));
#13476=DIRECTION('ref_axis',(0.,0.,1.));
#13477=DIRECTION('',(0.,-1.,0.));
#13478=DIRECTION('center_axis',(0.,-1.,0.));
#13479=DIRECTION('ref_axis',(0.,0.,1.));
#13480=DIRECTION('',(0.,-1.,0.));
#13481=DIRECTION('center_axis',(0.,-1.,0.));
#13482=DIRECTION('ref_axis',(0.,0.,1.));
#13483=DIRECTION('center_axis',(0.,1.,0.));
#13484=DIRECTION('ref_axis',(3.55274999902112E-15,0.,-1.));
#13485=DIRECTION('center_axis',(0.,1.,0.));
#13486=DIRECTION('ref_axis',(0.,0.,-1.));
#13487=DIRECTION('center_axis',(0.,-1.,0.));
#13488=DIRECTION('ref_axis',(0.,0.,1.));
#13489=DIRECTION('',(0.,1.,0.));
#13490=DIRECTION('center_axis',(0.,1.,0.));
#13491=DIRECTION('ref_axis',(0.,0.,-1.));
#13492=DIRECTION('',(0.,-1.,0.));
#13493=DIRECTION('center_axis',(0.,1.,0.));
#13494=DIRECTION('ref_axis',(-1.,0.,0.));
#13495=DIRECTION('center_axis',(0.,-1.,0.));
#13496=DIRECTION('ref_axis',(0.,0.,1.));
#13497=DIRECTION('',(0.,-1.,0.));
#13498=DIRECTION('center_axis',(0.,1.,0.));
#13499=DIRECTION('ref_axis',(0.,0.,1.));
#13500=DIRECTION('',(0.,1.,0.));
#13501=DIRECTION('center_axis',(0.,1.,0.));
#13502=DIRECTION('ref_axis',(-1.,0.,-3.1720657846433E-15));
#13503=DIRECTION('',(0.,1.,0.));
#13504=DIRECTION('',(0.,-1.,0.));
#13505=DIRECTION('center_axis',(0.,-1.,0.));
#13506=DIRECTION('ref_axis',(1.,0.,2.46716227694479E-15));
#13507=DIRECTION('',(0.,-1.,0.));
#13508=DIRECTION('center_axis',(0.,-1.,0.));
#13509=DIRECTION('ref_axis',(1.,0.,2.46716227694479E-15));
#13510=DIRECTION('',(0.,-1.,0.));
#13511=DIRECTION('center_axis',(0.,-1.,0.));
#13512=DIRECTION('ref_axis',(1.,0.,3.49157860180481E-15));
#13513=DIRECTION('center_axis',(0.,-1.,0.));
#13514=DIRECTION('ref_axis',(0.,0.,-1.));
#13515=DIRECTION('center_axis',(0.,1.,0.));
#13516=DIRECTION('ref_axis',(1.77625045523519E-15,0.,-1.));
#13517=DIRECTION('center_axis',(0.,1.,0.));
#13518=DIRECTION('ref_axis',(-5.32900045425631E-15,0.,-1.));
#13519=DIRECTION('center_axis',(0.,-1.,0.));
#13520=DIRECTION('ref_axis',(1.,0.,0.));
#13521=DIRECTION('center_axis',(0.,-1.,0.));
#13522=DIRECTION('ref_axis',(0.,0.,1.));
#13523=DIRECTION('',(0.,1.,0.));
#13524=DIRECTION('',(0.,-1.,0.));
#13525=DIRECTION('center_axis',(0.,1.,0.));
#13526=DIRECTION('ref_axis',(0.,0.,1.));
#13527=DIRECTION('',(0.,-1.,0.));
#13528=DIRECTION('',(0.,1.,0.));
#13529=DIRECTION('center_axis',(0.,1.,0.));
#13530=DIRECTION('ref_axis',(0.,0.,1.));
#13531=DIRECTION('',(0.,1.,0.));
#13532=DIRECTION('',(0.,-1.,0.));
#13533=DIRECTION('center_axis',(0.,-1.,0.));
#13534=DIRECTION('ref_axis',(0.,0.,-1.));
#13535=DIRECTION('center_axis',(0.,-1.,0.));
#13536=DIRECTION('ref_axis',(9.28647839630166E-15,0.,-1.));
#13537=DIRECTION('center_axis',(0.,1.,0.));
#13538=DIRECTION('ref_axis',(0.,0.,1.));
#13539=DIRECTION('center_axis',(0.,-1.,0.));
#13540=DIRECTION('ref_axis',(-0.996210606090467,0.,-0.086973721967411));
#13541=DIRECTION('center_axis',(0.,-1.,0.));
#13542=DIRECTION('ref_axis',(-1.,0.,-9.25030661388722E-15));
#13543=DIRECTION('center_axis',(0.,1.,0.));
#13544=DIRECTION('ref_axis',(0.,0.,1.));
#13545=DIRECTION('center_axis',(-4.73766340797087E-15,-1.,7.24463663858484E-14));
#13546=DIRECTION('ref_axis',(-0.0869737219674231,7.25670419811831E-14,0.996210606090466));
#13547=DIRECTION('',(0.,-1.,0.));
#13548=DIRECTION('center_axis',(2.63036692491839E-16,1.,-1.20858413416517E-14));
#13549=DIRECTION('ref_axis',(-1.28631872178907E-14,1.20792265079216E-14,
1.));
#13550=DIRECTION('center_axis',(0.,-1.,0.));
#13551=DIRECTION('ref_axis',(0.,0.,1.));
#13552=DIRECTION('',(0.,-1.,0.));
#13553=DIRECTION('center_axis',(0.,-1.,0.));
#13554=DIRECTION('ref_axis',(0.,0.,-1.));
#13555=DIRECTION('',(0.,1.,0.));
#13556=DIRECTION('center_axis',(0.,-1.,0.));
#13557=DIRECTION('ref_axis',(0.,0.,-1.));
#13558=DIRECTION('',(0.,-1.,0.));
#13559=DIRECTION('center_axis',(0.,-1.,0.));
#13560=DIRECTION('ref_axis',(0.,0.,-1.));
#13561=DIRECTION('center_axis',(0.,-1.,0.));
#13562=DIRECTION('ref_axis',(0.,0.,1.));
#13563=DIRECTION('center_axis',(-4.57877760372757E-17,1.,-2.10629550201326E-15));
#13564=DIRECTION('ref_axis',(-0.996210606090468,1.37524400469719E-16,0.0869737219674006));
#13565=DIRECTION('center_axis',(-7.24349194418465E-14,1.,-5.26423728347428E-15));
#13566=DIRECTION('ref_axis',(-1.,-7.24295175807043E-14,-2.03897830519296E-14));
#13567=DIRECTION('center_axis',(0.,-1.,0.));
#13568=DIRECTION('ref_axis',(8.88066502056514E-16,0.,1.));
#13569=DIRECTION('',(0.,-1.,0.));
#13570=DIRECTION('center_axis',(0.,-1.,0.));
#13571=DIRECTION('ref_axis',(0.,0.,-1.));
#13572=DIRECTION('center_axis',(0.,-1.,0.));
#13573=DIRECTION('ref_axis',(0.,0.,-1.));
#13574=DIRECTION('',(0.,-1.,0.));
#13575=DIRECTION('center_axis',(0.,-1.,0.));
#13576=DIRECTION('ref_axis',(0.,0.,-1.));
#13577=DIRECTION('',(0.,1.,0.));
#13578=DIRECTION('center_axis',(0.,-1.,0.));
#13579=DIRECTION('ref_axis',(0.,0.,1.));
#13580=DIRECTION('center_axis',(0.,1.,0.));
#13581=DIRECTION('ref_axis',(-0.0869737219674249,0.,-0.996210606090466));
#13582=DIRECTION('center_axis',(-2.63036692491925E-16,1.,1.20858413416538E-14));
#13583=DIRECTION('ref_axis',(1.108575596911E-14,1.20792265079196E-14,-1.));
#13584=DIRECTION('center_axis',(0.,-1.,0.));
#13585=DIRECTION('ref_axis',(0.,0.,1.));
#13586=DIRECTION('',(0.,-1.,0.));
#13587=DIRECTION('center_axis',(0.,-1.,0.));
#13588=DIRECTION('ref_axis',(0.,0.,-1.));
#13589=DIRECTION('',(0.,1.,0.));
#13590=DIRECTION('center_axis',(0.,-1.,0.));
#13591=DIRECTION('ref_axis',(0.,0.,-1.));
#13592=DIRECTION('center_axis',(0.,-1.,0.));
#13593=DIRECTION('ref_axis',(0.,0.,-1.));
#13594=DIRECTION('',(0.,1.,0.));
#13595=DIRECTION('center_axis',(0.,-1.,0.));
#13596=DIRECTION('ref_axis',(-2.66447930027857E-15,0.,1.));
#13597=DIRECTION('center_axis',(-1.20629474536324E-14,1.,1.31618444349839E-15));
#13598=DIRECTION('ref_axis',(0.996210606090468,1.21250679747461E-14,-0.0869737219674049));
#13599=DIRECTION('center_axis',(-1.21087352296684E-14,1.,7.90111058514839E-16));
#13600=DIRECTION('ref_axis',(1.,1.21021472413359E-14,-7.38620634189485E-15));
#13601=DIRECTION('center_axis',(0.,-1.,0.));
#13602=DIRECTION('ref_axis',(-1.77641279822206E-15,0.,1.));
#13603=DIRECTION('center_axis',(0.,-1.,0.));
#13604=DIRECTION('ref_axis',(0.,0.,-1.));
#13605=DIRECTION('',(0.,1.,0.));
#13606=DIRECTION('center_axis',(0.,-1.,0.));
#13607=DIRECTION('ref_axis',(0.,0.,-1.));
#13608=DIRECTION('',(0.,-1.,0.));
#13609=DIRECTION('center_axis',(0.,-1.,0.));
#13610=DIRECTION('ref_axis',(0.,0.,-1.));
#13611=DIRECTION('',(0.,1.,0.));
#13612=DIRECTION('center_axis',(0.,-1.,0.));
#13613=DIRECTION('ref_axis',(1.77641279822206E-15,0.,1.));
#13614=DIRECTION('center_axis',(5.26073384983703E-16,1.,2.4171682683304E-14));
#13615=DIRECTION('ref_axis',(0.086973721967389,-2.41355322824308E-14,0.996210606090469));
#13616=DIRECTION('center_axis',(-7.36903131392929E-15,-1.,-1.44938520547765E-13));
#13617=DIRECTION('ref_axis',(1.04987703118978E-14,-1.44950718095046E-13,
1.));
#13618=DIRECTION('center_axis',(0.,1.,0.));
#13619=DIRECTION('ref_axis',(0.,0.,1.));
#13620=DIRECTION('center_axis',(-1.4493852054775E-13,-1.,-7.36903131392888E-15));
#13621=DIRECTION('ref_axis',(0.996210606090468,-1.45042401028705E-13,0.0869737219673961));
#13622=DIRECTION('center_axis',(7.24463663858355E-14,-1.,-4.73766340796999E-15));
#13623=DIRECTION('ref_axis',(1.,7.24295175807267E-14,1.93479640910857E-14));
#13624=DIRECTION('center_axis',(0.,1.,0.));
#13625=DIRECTION('ref_axis',(0.,0.,1.));
#13626=DIRECTION('center_axis',(0.,-1.,0.));
#13627=DIRECTION('ref_axis',(0.0869737219673973,0.,-0.996210606090468));
#13628=DIRECTION('center_axis',(0.,-1.,0.));
#13629=DIRECTION('ref_axis',(0.,0.,-1.));
#13630=DIRECTION('',(0.,-1.,0.));
#13631=DIRECTION('center_axis',(0.,-1.,0.));
#13632=DIRECTION('ref_axis',(0.,0.,-1.));
#13633=DIRECTION('',(0.,-1.,0.));
#13634=DIRECTION('center_axis',(0.,-1.,0.));
#13635=DIRECTION('ref_axis',(0.,0.,-1.));
#13636=DIRECTION('center_axis',(0.,-1.,0.));
#13637=DIRECTION('ref_axis',(0.,0.,-1.));
#13638=DIRECTION('center_axis',(0.,1.,0.));
#13639=DIRECTION('ref_axis',(0.,0.,-1.));
#13640=DIRECTION('center_axis',(0.,1.,0.));
#13641=DIRECTION('ref_axis',(0.,0.,-1.));
#13642=DIRECTION('center_axis',(0.,-1.,0.));
#13643=DIRECTION('ref_axis',(0.,0.,-1.));
#13644=DIRECTION('center_axis',(0.,-1.,0.));
#13645=DIRECTION('ref_axis',(0.,0.,1.));
#13646=DIRECTION('',(0.,1.,0.));
#13647=DIRECTION('',(0.,-1.,0.));
#13648=DIRECTION('center_axis',(0.,1.,0.));
#13649=DIRECTION('ref_axis',(0.,0.,1.));
#13650=DIRECTION('center_axis',(0.,1.,0.));
#13651=DIRECTION('ref_axis',(0.,0.,-1.));
#13652=DIRECTION('',(0.,1.,0.));
#13653=DIRECTION('center_axis',(0.,1.,0.));
#13654=DIRECTION('ref_axis',(0.,0.,1.));
#13655=DIRECTION('',(0.,1.,0.));
#13656=DIRECTION('center_axis',(0.,1.,0.));
#13657=DIRECTION('ref_axis',(0.,0.,1.));
#13658=DIRECTION('',(3.29601953873307E-15,0.,-1.));
#13659=DIRECTION('',(1.,0.,0.));
#13660=DIRECTION('',(-3.46944695195362E-15,0.,-1.));
#13661=DIRECTION('',(0.,0.,1.));
#13662=DIRECTION('center_axis',(0.,1.,0.));
#13663=DIRECTION('ref_axis',(0.,0.,1.));
#13664=DIRECTION('center_axis',(0.,-1.,0.));
#13665=DIRECTION('ref_axis',(1.11022302462516E-14,0.,1.));
#13666=DIRECTION('',(-1.,0.,-1.03892784411108E-15));
#13667=DIRECTION('center_axis',(0.,-1.,0.));
#13668=DIRECTION('ref_axis',(0.,0.,1.));
#13669=DIRECTION('center_axis',(0.,1.,0.));
#13670=DIRECTION('ref_axis',(0.,0.,1.));
#13671=DIRECTION('center_axis',(0.,-1.,0.));
#13672=DIRECTION('ref_axis',(5.55111512312578E-15,0.,1.));
#13673=DIRECTION('',(0.,0.,1.));
#13674=DIRECTION('',(-3.46944695195362E-15,0.,-1.));
#13675=DIRECTION('',(1.,0.,0.));
#13676=DIRECTION('',(3.29601953873307E-15,0.,-1.));
#13677=DIRECTION('center_axis',(0.,1.,0.));
#13678=DIRECTION('ref_axis',(0.,0.,1.));
#13679=DIRECTION('',(-1.,0.,1.95461800110063E-16));
#13680=DIRECTION('center_axis',(0.,1.,0.));
#13681=DIRECTION('ref_axis',(0.,0.,1.));
#13682=DIRECTION('',(0.,0.,1.));
#13683=DIRECTION('center_axis',(0.,1.,0.));
#13684=DIRECTION('ref_axis',(0.,0.,1.));
#13685=DIRECTION('',(1.,0.,-1.95461800110063E-16));
#13686=DIRECTION('center_axis',(0.,1.,0.));
#13687=DIRECTION('ref_axis',(0.,0.,1.));
#13688=DIRECTION('center_axis',(0.,1.,0.));
#13689=DIRECTION('ref_axis',(0.,0.,1.));
#13690=DIRECTION('center_axis',(0.,-1.,0.));
#13691=DIRECTION('ref_axis',(1.38777878078144E-14,0.,1.));
#13692=DIRECTION('',(-1.,0.,-1.04744440165294E-14));
#13693=DIRECTION('center_axis',(0.,-1.,0.));
#13694=DIRECTION('ref_axis',(-5.55111512312578E-15,0.,1.));
#13695=DIRECTION('center_axis',(0.,1.,0.));
#13696=DIRECTION('ref_axis',(0.,0.,1.));
#13697=DIRECTION('',(1.15133718606405E-14,0.,-1.));
#13698=DIRECTION('center_axis',(0.,-1.,0.));
#13699=DIRECTION('ref_axis',(0.,0.,1.));
#13700=DIRECTION('center_axis',(0.,1.,0.));
#13701=DIRECTION('ref_axis',(0.,0.,1.));
#13702=DIRECTION('center_axis',(0.,-1.,0.));
#13703=DIRECTION('ref_axis',(0.,0.,1.));
#13704=DIRECTION('',(1.,0.,3.49148133884313E-15));
#13705=DIRECTION('center_axis',(0.,-1.,0.));
#13706=DIRECTION('ref_axis',(0.,0.,1.));
#13707=DIRECTION('center_axis',(0.,-1.,0.));
#13708=DIRECTION('ref_axis',(0.,0.,1.));
#13709=DIRECTION('',(-4.53040918295421E-15,0.,1.));
#13710=DIRECTION('center_axis',(0.,1.,0.));
#13711=DIRECTION('ref_axis',(0.,0.,1.));
#13712=DIRECTION('',(0.,0.,-1.));
#13713=DIRECTION('center_axis',(0.,-1.,0.));
#13714=DIRECTION('ref_axis',(0.,0.,1.));
#13715=DIRECTION('center_axis',(0.,-1.,0.));
#13716=DIRECTION('ref_axis',(5.55111512312578E-15,0.,1.));
#13717=DIRECTION('',(1.,0.,1.03892784411108E-15));
#13718=DIRECTION('center_axis',(0.,-1.,0.));
#13719=DIRECTION('ref_axis',(0.,0.,1.));
#13720=DIRECTION('center_axis',(0.,-1.,0.));
#13721=DIRECTION('ref_axis',(-3.55264982748976E-15,0.,1.));
#13722=DIRECTION('',(-1.,0.,0.));
#13723=DIRECTION('center_axis',(0.,-1.,0.));
#13724=DIRECTION('ref_axis',(0.,0.,1.));
#13725=DIRECTION('',(0.,0.,-1.));
#13726=DIRECTION('center_axis',(0.,-1.,0.));
#13727=DIRECTION('ref_axis',(1.77632491374488E-15,0.,1.));
#13728=DIRECTION('',(1.,0.,0.));
#13729=DIRECTION('center_axis',(0.,-1.,0.));
#13730=DIRECTION('ref_axis',(0.,0.,1.));
#13731=DIRECTION('',(-3.49148133884313E-15,0.,1.));
#13732=DIRECTION('center_axis',(-1.,0.,-3.29601953873307E-15));
#13733=DIRECTION('ref_axis',(-3.29601953873307E-15,0.,1.));
#13734=DIRECTION('',(0.,-1.,0.));
#13735=DIRECTION('',(-3.29601953873307E-15,0.,1.));
#13736=DIRECTION('',(0.,-1.,0.));
#13737=DIRECTION('',(3.29601953873307E-15,0.,-1.));
#13738=DIRECTION('center_axis',(-1.,0.,-3.29601953873307E-15));
#13739=DIRECTION('ref_axis',(-3.29601953873307E-15,0.,1.));
#13740=DIRECTION('',(0.,-1.,0.));
#13741=DIRECTION('',(-3.29601953873307E-15,0.,1.));
#13742=DIRECTION('',(0.,-1.,0.));
#13743=DIRECTION('',(3.29601953873307E-15,0.,-1.));
#13744=DIRECTION('center_axis',(0.,-1.,0.));
#13745=DIRECTION('ref_axis',(0.,0.,1.));
#13746=DIRECTION('',(-3.46944695195362E-15,0.,-1.));
#13747=DIRECTION('',(0.949699126201879,0.,0.313163806483743));
#13748=DIRECTION('',(-0.313163806483745,0.,0.949699126201879));
#13749=DIRECTION('',(-0.949699126201879,0.,-0.313163806483744));
#13750=DIRECTION('',(-3.46944695195362E-15,0.,-1.));
#13751=DIRECTION('',(1.,0.,0.));
#13752=DIRECTION('',(3.29601953873307E-15,0.,-1.));
#13753=DIRECTION('center_axis',(0.,-1.,0.));
#13754=DIRECTION('ref_axis',(0.,0.,-1.));
#13755=DIRECTION('',(0.707106781186547,0.,0.707106781186548));
#13756=DIRECTION('center_axis',(0.,-1.,0.));
#13757=DIRECTION('ref_axis',(0.,0.,-1.));
#13758=DIRECTION('',(-0.707106781186548,0.,-0.707106781186547));
#13759=DIRECTION('center_axis',(0.,-1.,0.));
#13760=DIRECTION('ref_axis',(0.,0.,-1.));
#13761=DIRECTION('',(1.,0.,-1.95461800110063E-16));
#13762=DIRECTION('center_axis',(0.,1.,0.));
#13763=DIRECTION('ref_axis',(0.,0.,-1.));
#13764=DIRECTION('',(3.29601953873307E-15,0.,-1.));
#13765=DIRECTION('',(1.,0.,0.));
#13766=DIRECTION('',(-3.46944695195362E-15,0.,-1.));
#13767=DIRECTION('',(1.,0.,0.));
#13768=DIRECTION('center_axis',(0.,1.,0.));
#13769=DIRECTION('ref_axis',(0.,0.,-1.));
#13770=DIRECTION('',(-1.,0.,0.));
#13771=DIRECTION('',(-3.29601953873307E-15,0.,1.));
#13772=DIRECTION('center_axis',(0.,-1.,0.));
#13773=DIRECTION('ref_axis',(2.35106052273563E-14,0.,1.));
#13774=DIRECTION('',(-1.,0.,1.95461800110063E-16));
#13775=DIRECTION('center_axis',(0.,1.,0.));
#13776=DIRECTION('ref_axis',(0.,0.,1.));
#13777=DIRECTION('',(0.707106781186548,0.,0.707106781186547));
#13778=DIRECTION('',(-0.707106781186547,0.,-0.707106781186548));
#13779=DIRECTION('center_axis',(0.,1.,0.));
#13780=DIRECTION('ref_axis',(0.,0.,1.));
#13781=DIRECTION('',(-3.29601953873307E-15,0.,1.));
#13782=DIRECTION('',(-1.,0.,0.));
#13783=DIRECTION('',(3.46944695195362E-15,0.,1.));
#13784=DIRECTION('',(-1.,0.,0.));
#13785=DIRECTION('',(3.46944695195362E-15,0.,1.));
#13786=DIRECTION('',(-1.,0.,0.));
#13787=DIRECTION('',(3.46944695195362E-15,0.,1.));
#13788=DIRECTION('center_axis',(1.,0.,0.));
#13789=DIRECTION('ref_axis',(0.,0.,-1.));
#13790=DIRECTION('',(0.,1.,0.));
#13791=DIRECTION('',(0.,0.,1.));
#13792=DIRECTION('',(0.,1.,0.));
#13793=DIRECTION('',(0.,0.,-1.));
#13794=DIRECTION('center_axis',(3.29601953873307E-15,0.,-1.));
#13795=DIRECTION('ref_axis',(-1.,0.,-3.29601953873307E-15));
#13796=DIRECTION('center_axis',(0.,0.,1.));
#13797=DIRECTION('ref_axis',(-1.,0.,0.));
#13798=DIRECTION('center_axis',(0.,0.,1.));
#13799=DIRECTION('ref_axis',(1.,0.,0.));
#13800=DIRECTION('center_axis',(-3.29601953873307E-15,0.,1.));
#13801=DIRECTION('ref_axis',(1.,0.,3.29601953873307E-15));
#13802=DIRECTION('center_axis',(0.,0.,1.));
#13803=DIRECTION('ref_axis',(-1.,0.,0.));
#13804=DIRECTION('center_axis',(0.,0.,1.));
#13805=DIRECTION('ref_axis',(1.,0.,0.));
#13806=DIRECTION('center_axis',(3.29601953873307E-15,0.,-1.));
#13807=DIRECTION('ref_axis',(-1.,0.,-3.29601953873307E-15));
#13808=DIRECTION('',(-3.29601953873307E-15,0.,1.));
#13809=DIRECTION('center_axis',(0.,0.,1.));
#13810=DIRECTION('ref_axis',(-1.,0.,0.));
#13811=DIRECTION('center_axis',(0.,0.,1.));
#13812=DIRECTION('ref_axis',(1.,0.,0.));
#13813=DIRECTION('center_axis',(-3.29601953873307E-15,0.,1.));
#13814=DIRECTION('ref_axis',(1.,0.,3.29601953873307E-15));
#13815=DIRECTION('center_axis',(0.,0.,1.));
#13816=DIRECTION('ref_axis',(-1.,0.,0.));
#13817=DIRECTION('center_axis',(0.,0.,1.));
#13818=DIRECTION('ref_axis',(1.,0.,0.));
#13819=DIRECTION('center_axis',(0.,0.,1.));
#13820=DIRECTION('ref_axis',(1.,0.,0.));
#13821=DIRECTION('center_axis',(0.,0.,1.));
#13822=DIRECTION('ref_axis',(-1.,0.,0.));
#13823=DIRECTION('center_axis',(0.,0.,-1.));
#13824=DIRECTION('ref_axis',(-1.,0.,0.));
#13825=DIRECTION('center_axis',(0.,0.,1.));
#13826=DIRECTION('ref_axis',(-1.,0.,0.));
#13827=DIRECTION('',(0.,0.,-1.));
#13828=DIRECTION('center_axis',(-0.313163806483744,0.,0.949699126201879));
#13829=DIRECTION('ref_axis',(0.949699126201879,0.,0.313163806483744));
#13830=DIRECTION('',(0.949699126201879,0.,0.313163806483744));
#13831=DIRECTION('',(0.,-1.,0.));
#13832=DIRECTION('',(-0.949699126201879,0.,-0.313163806483744));
#13833=DIRECTION('',(0.,1.,0.));
#13834=DIRECTION('center_axis',(-0.949699126201879,0.,-0.313163806483744));
#13835=DIRECTION('ref_axis',(-0.313163806483744,0.,0.949699126201879));
#13836=DIRECTION('center_axis',(0.949699126201879,0.,0.313163806483743));
#13837=DIRECTION('ref_axis',(-0.313163806483743,-5.55111512312581E-15,0.949699126201879));
#13838=DIRECTION('',(0.949699126201879,0.,0.313163806483744));
#13839=DIRECTION('center_axis',(-0.949699126201878,0.,-0.313163806483745));
#13840=DIRECTION('ref_axis',(-0.313163806483745,0.,0.949699126201878));
#13841=DIRECTION('center_axis',(-0.949699126201879,0.,-0.313163806483744));
#13842=DIRECTION('ref_axis',(-0.313163806483744,0.,0.949699126201879));
#13843=DIRECTION('center_axis',(0.949699126201879,0.,0.313163806483743));
#13844=DIRECTION('ref_axis',(-0.313163806483743,0.,0.949699126201879));
#13845=DIRECTION('center_axis',(0.949699126201877,0.,0.313163806483749));
#13846=DIRECTION('ref_axis',(-0.313163806483749,0.,0.949699126201877));
#13847=DIRECTION('',(-0.949699126201879,0.,-0.313163806483744));
#13848=DIRECTION('center_axis',(0.,1.,0.));
#13849=DIRECTION('ref_axis',(0.,0.,1.));
#13850=DIRECTION('',(-0.949699126201879,0.,-0.313163806483743));
#13851=DIRECTION('center_axis',(0.,-1.,0.));
#13852=DIRECTION('ref_axis',(0.,0.,1.));
#13853=DIRECTION('center_axis',(0.,1.,0.));
#13854=DIRECTION('ref_axis',(0.,0.,1.));
#13855=DIRECTION('',(-0.949699126201879,0.,-0.313163806483743));
#13856=DIRECTION('',(-0.313163806483742,0.,0.949699126201879));
#13857=DIRECTION('center_axis',(0.,0.,1.));
#13858=DIRECTION('ref_axis',(1.,0.,0.));
#13859=DIRECTION('center_axis',(3.53117861454706E-12,8.1303226733511E-11,
-1.));
#13860=DIRECTION('ref_axis',(6.36382861148608E-5,0.999999997975084,8.13034512870338E-11));
#13861=DIRECTION('center_axis',(-3.61565657182522E-12,8.32482800044714E-11,
-1.));
#13862=DIRECTION('ref_axis',(-6.36384976265908E-5,0.999999997975071,8.32485099308517E-11));
#13863=DIRECTION('',(1.,0.,0.));
#13864=DIRECTION('center_axis',(-1.,0.,-3.49148133884313E-15));
#13865=DIRECTION('ref_axis',(-3.49148133884313E-15,0.,1.));
#13866=DIRECTION('center_axis',(1.,8.24701670271546E-11,3.58608928678165E-12));
#13867=DIRECTION('ref_axis',(-8.24703950728649E-11,0.999999997975082,6.36383222378267E-5));
#13868=DIRECTION('center_axis',(1.,8.30538663463606E-11,-3.60298487823237E-12));
#13869=DIRECTION('ref_axis',(-8.30540954665947E-11,0.999999997975073,-6.36384608246681E-5));
#13870=DIRECTION('',(-3.49148133884313E-15,0.,1.));
#13871=DIRECTION('center_axis',(1.,0.,0.));
#13872=DIRECTION('ref_axis',(0.,0.,-1.));
#13873=DIRECTION('center_axis',(-1.,-8.28592693501252E-11,3.59876098036562E-12));
#13874=DIRECTION('ref_axis',(-8.28594982030728E-11,0.999999997975053,-6.36387730413301E-5));
#13875=DIRECTION('center_axis',(-1.,0.,0.));
#13876=DIRECTION('ref_axis',(0.,0.999999997975064,6.3638598276304E-5));
#13877=DIRECTION('',(0.,0.,1.));
#13878=DIRECTION('center_axis',(0.,0.,-1.));
#13879=DIRECTION('ref_axis',(-1.,0.,0.));
#13880=DIRECTION('center_axis',(-3.58186538891853E-12,8.2470258696193E-11,
1.));
#13881=DIRECTION('ref_axis',(6.3638285669282E-5,-0.999999997975084,8.24704864729705E-11));
#13882=DIRECTION('center_axis',(3.61565657182547E-12,8.32482800044776E-11,
1.));
#13883=DIRECTION('ref_axis',(-6.36385026828668E-5,-0.99999999797507,8.32485099308762E-11));
#13884=DIRECTION('',(-1.,0.,0.));
#13885=DIRECTION('center_axis',(0.,-1.,0.));
#13886=DIRECTION('ref_axis',(0.,0.,-1.));
#13887=DIRECTION('center_axis',(0.,1.,0.));
#13888=DIRECTION('ref_axis',(3.5527735616222E-15,0.,-1.));
#13889=DIRECTION('center_axis',(0.285050819318021,0.0292578032183599,-0.958065765674237));
#13890=DIRECTION('ref_axis',(0.665144932848858,0.713664621963304,0.219693025978211));
#13891=DIRECTION('center_axis',(0.,1.,0.));
#13892=DIRECTION('ref_axis',(0.,0.,1.));
#13893=DIRECTION('center_axis',(0.,-1.,0.));
#13894=DIRECTION('ref_axis',(0.,0.,-1.));
#13895=DIRECTION('center_axis',(0.289353946523101,0.0248003127138381,-0.956900850726345));
#13896=DIRECTION('ref_axis',(-0.668092365814573,0.72113931848567,-0.183332141410909));
#13897=DIRECTION('center_axis',(0.,-1.,0.));
#13898=DIRECTION('ref_axis',(0.,0.,-1.));
#13899=DIRECTION('',(-0.949699126201879,0.,-0.313163806483743));
#13900=DIRECTION('',(-0.313163806483743,0.,0.949699126201879));
#13901=DIRECTION('center_axis',(0.,-1.,0.));
#13902=DIRECTION('ref_axis',(0.,0.,-1.));
#13903=DIRECTION('center_axis',(0.,1.,0.));
#13904=DIRECTION('ref_axis',(-1.7762059938806E-15,0.,-1.));
#13905=DIRECTION('',(0.313163806483747,0.,-0.949699126201878));
#13906=DIRECTION('center_axis',(0.,1.,0.));
#13907=DIRECTION('ref_axis',(-5.32920569145862E-15,0.,-1.));
#13908=DIRECTION('',(-0.313163806483747,0.,0.949699126201878));
#13909=DIRECTION('center_axis',(0.,-1.,0.));
#13910=DIRECTION('ref_axis',(0.,0.,-1.));
#13911=DIRECTION('center_axis',(0.,1.,0.));
#13912=DIRECTION('ref_axis',(-1.7762059938806E-15,0.,-1.));
#13913=DIRECTION('',(-0.949699126201879,0.,-0.313163806483744));
#13914=DIRECTION('center_axis',(0.,1.,0.));
#13915=DIRECTION('ref_axis',(0.,0.,-1.));
#13916=DIRECTION('',(0.949699126201879,0.,0.313163806483744));
#13917=DIRECTION('center_axis',(0.,-1.,0.));
#13918=DIRECTION('ref_axis',(0.,0.,-1.));
#13919=DIRECTION('center_axis',(0.,1.,0.));
#13920=DIRECTION('ref_axis',(0.,0.,-1.));
#13921=DIRECTION('',(-0.313163806483754,0.,0.949699126201876));
#13922=DIRECTION('center_axis',(0.,1.,0.));
#13923=DIRECTION('ref_axis',(8.88172787481047E-15,0.,-1.));
#13924=DIRECTION('',(0.313163806483754,0.,-0.949699126201876));
#13925=DIRECTION('center_axis',(0.,1.,0.));
#13926=DIRECTION('ref_axis',(-1.7762059938806E-15,0.,-1.));
#13927=DIRECTION('',(0.949699126201879,0.,0.313163806483744));
#13928=DIRECTION('center_axis',(0.,1.,0.));
#13929=DIRECTION('ref_axis',(0.,0.,-1.));
#13930=DIRECTION('',(-0.949699126201879,0.,-0.313163806483744));
#13931=DIRECTION('',(0.313163806483743,0.,-0.949699126201879));
#13932=DIRECTION('',(-0.949699126201879,0.,-0.313163806483743));
#13933=DIRECTION('center_axis',(0.,1.,0.));
#13934=DIRECTION('ref_axis',(0.,0.,1.));
#13935=DIRECTION('center_axis',(0.,1.,0.));
#13936=DIRECTION('ref_axis',(0.,0.,-1.));
#13937=DIRECTION('center_axis',(0.313163806483744,0.,-0.949699126201879));
#13938=DIRECTION('ref_axis',(-0.949699126201879,0.,-0.313163806483744));
#13939=DIRECTION('',(0.,1.,0.));
#13940=DIRECTION('',(-0.949699126201879,0.,-0.313163806483744));
#13941=DIRECTION('',(-0.949699126201879,0.,-0.313163806483744));
#13942=DIRECTION('center_axis',(-0.313163806461999,-2.38433636067788E-11,
0.949699126209049));
#13943=DIRECTION('ref_axis',(-0.658107038058548,0.720972457655595,-0.217011155841942));
#13944=DIRECTION('',(0.949699126201879,0.,0.313163806483744));
#13945=DIRECTION('center_axis',(0.313163806483744,0.,-0.949699126201879));
#13946=DIRECTION('ref_axis',(-0.949699126201879,0.,-0.313163806483744));
#13947=DIRECTION('',(0.,1.,0.));
#13948=DIRECTION('',(0.949699126201879,0.,0.313163806483744));
#13949=DIRECTION('',(0.,-1.,0.));
#13950=DIRECTION('',(-0.949699126201879,0.,-0.313163806483744));
#13951=DIRECTION('center_axis',(0.313163806494915,-1.26989761058302E-11,
-0.949699126198195));
#13952=DIRECTION('ref_axis',(-0.641714392326136,0.737174116651431,-0.211605671995528));
#13953=DIRECTION('',(0.949699126201879,0.,0.313163806483744));
#13954=DIRECTION('center_axis',(0.,-1.,0.));
#13955=DIRECTION('ref_axis',(0.,0.,-1.));
#13956=DIRECTION('center_axis',(0.,1.,0.));
#13957=DIRECTION('ref_axis',(0.,0.,1.));
#13958=DIRECTION('center_axis',(0.,1.,0.));
#13959=DIRECTION('ref_axis',(-2.66445855087016E-15,0.,-1.));
#13960=DIRECTION('center_axis',(-0.298581522051401,-0.0150877415291002,
0.954264866137814));
#13961=DIRECTION('ref_axis',(-0.649648952678908,0.73568412721389,-0.191637948352447));
#13962=DIRECTION('center_axis',(0.,-1.,0.));
#13963=DIRECTION('ref_axis',(0.,0.,-1.));
#13964=DIRECTION('center_axis',(0.,-1.,0.));
#13965=DIRECTION('ref_axis',(0.,0.,-1.));
#13966=DIRECTION('center_axis',(0.,-1.,0.));
#13967=DIRECTION('ref_axis',(0.,0.,-1.));
#13968=DIRECTION('center_axis',(0.,1.,0.));
#13969=DIRECTION('ref_axis',(0.,0.,-1.));
#13970=DIRECTION('center_axis',(0.,1.,0.));
#13971=DIRECTION('ref_axis',(-8.88249771892961E-16,0.,-1.));
#13972=DIRECTION('center_axis',(0.,1.,0.));
#13973=DIRECTION('ref_axis',(0.,0.,1.));
#13974=DIRECTION('',(0.,1.,0.));
#13975=DIRECTION('center_axis',(0.,-1.,0.));
#13976=DIRECTION('ref_axis',(0.,0.,1.));
#13977=DIRECTION('',(0.,-1.,0.));
#13978=DIRECTION('center_axis',(0.,1.,0.));
#13979=DIRECTION('ref_axis',(0.,0.,1.));
#13980=DIRECTION('center_axis',(0.,1.,0.));
#13981=DIRECTION('ref_axis',(1.65389215948552E-15,0.,-1.));
#13982=DIRECTION('center_axis',(0.,-1.,0.));
#13983=DIRECTION('ref_axis',(1.77645503129512E-15,0.,1.));
#13984=DIRECTION('center_axis',(0.,1.,0.));
#13985=DIRECTION('ref_axis',(0.,0.,1.));
#13986=DIRECTION('center_axis',(0.,1.,0.));
#13987=DIRECTION('ref_axis',(0.,0.,1.));
#13988=DIRECTION('',(0.500130397801055,-0.706999113223839,0.500021838619139));
#13989=DIRECTION('center_axis',(0.,1.,0.));
#13990=DIRECTION('ref_axis',(0.,0.,1.));
#13991=DIRECTION('',(-0.500130397801063,0.706999113223845,0.500021838619122));
#13992=DIRECTION('center_axis',(0.,-1.,0.));
#13993=DIRECTION('ref_axis',(0.,0.,1.));
#13994=DIRECTION('center_axis',(0.,-1.,0.));
#13995=DIRECTION('ref_axis',(0.,0.,1.));
#13996=DIRECTION('center_axis',(0.,1.,0.));
#13997=DIRECTION('ref_axis',(4.56335677841536E-15,0.,-1.));
#13998=DIRECTION('',(-0.500021838619135,-0.706999113223842,0.500130397801054));
#13999=DIRECTION('center_axis',(0.,1.,0.));
#14000=DIRECTION('ref_axis',(0.,0.,1.));
#14001=DIRECTION('',(-0.500021838619135,0.706999113223842,-0.500130397801054));
#14002=DIRECTION('center_axis',(0.,-1.,0.));
#14003=DIRECTION('ref_axis',(0.,0.,1.));
#14004=DIRECTION('center_axis',(0.,-1.,0.));
#14005=DIRECTION('ref_axis',(0.,0.,1.));
#14006=DIRECTION('center_axis',(0.,-1.,0.));
#14007=DIRECTION('ref_axis',(0.,0.,-1.));
#14008=DIRECTION('',(-1.,0.,1.95461800110063E-16));
#14009=DIRECTION('center_axis',(0.,1.,0.));
#14010=DIRECTION('ref_axis',(0.,0.,-1.));
#14011=DIRECTION('',(0.,0.,1.));
#14012=DIRECTION('center_axis',(0.,-1.,0.));
#14013=DIRECTION('ref_axis',(0.,0.,-1.));
#14014=DIRECTION('',(-0.707106781186547,0.,-0.707106781186548));
#14015=DIRECTION('',(0.707106781186548,0.,0.707106781186547));
#14016=DIRECTION('center_axis',(0.,-1.,0.));
#14017=DIRECTION('ref_axis',(0.,0.,-1.));
#14018=DIRECTION('center_axis',(0.,1.,0.));
#14019=DIRECTION('ref_axis',(0.,0.,1.));
#14020=DIRECTION('',(0.,0.,-1.));
#14021=DIRECTION('center_axis',(0.,-1.,0.));
#14022=DIRECTION('ref_axis',(0.,0.,1.));
#14023=DIRECTION('',(1.,0.,-1.95461800110063E-16));
#14024=DIRECTION('center_axis',(0.,1.,0.));
#14025=DIRECTION('ref_axis',(0.,0.,1.));
#14026=DIRECTION('',(-0.707106781186548,0.,-0.707106781186547));
#14027=DIRECTION('center_axis',(0.,1.,0.));
#14028=DIRECTION('ref_axis',(0.,0.,1.));
#14029=DIRECTION('',(0.707106781186547,0.,0.707106781186548));
#14030=DIRECTION('center_axis',(0.,1.,0.));
#14031=DIRECTION('ref_axis',(0.,0.,1.));
#14032=DIRECTION('center_axis',(1.95461800110063E-16,0.,1.));
#14033=DIRECTION('ref_axis',(1.,0.,-1.95461800110063E-16));
#14034=DIRECTION('',(1.,0.,-1.95461800110063E-16));
#14035=DIRECTION('',(0.,-1.,0.));
#14036=DIRECTION('',(-1.,0.,1.95461800110063E-16));
#14037=DIRECTION('',(0.,-1.,0.));
#14038=DIRECTION('',(1.,0.,-1.95461800110063E-16));
#14039=DIRECTION('center_axis',(1.,0.,0.));
#14040=DIRECTION('ref_axis',(0.,0.,-1.));
#14041=DIRECTION('',(0.,-1.,0.));
#14042=DIRECTION('',(0.,0.,-1.));
#14043=DIRECTION('',(0.,0.,-1.));
#14044=DIRECTION('',(0.,-1.,0.));
#14045=DIRECTION('',(0.,0.,1.));
#14046=DIRECTION('center_axis',(0.,-1.,0.));
#14047=DIRECTION('ref_axis',(0.,0.,-1.));
#14048=DIRECTION('center_axis',(0.,-1.,0.));
#14049=DIRECTION('ref_axis',(0.,0.,-1.));
#14050=DIRECTION('center_axis',(0.,1.,0.));
#14051=DIRECTION('ref_axis',(0.,0.,1.));
#14052=DIRECTION('center_axis',(1.95461800110063E-16,0.,1.));
#14053=DIRECTION('ref_axis',(1.,0.,-1.95461800110063E-16));
#14054=DIRECTION('',(0.,-1.,0.));
#14055=DIRECTION('',(-1.,0.,1.95461800110063E-16));
#14056=DIRECTION('',(-1.,0.,1.95461800110063E-16));
#14057=DIRECTION('',(0.,-1.,0.));
#14058=DIRECTION('',(1.,0.,-1.95461800110063E-16));
#14059=DIRECTION('center_axis',(1.,0.,0.));
#14060=DIRECTION('ref_axis',(0.,0.,-1.));
#14061=DIRECTION('',(0.,0.,1.));
#14062=DIRECTION('',(0.,-1.,0.));
#14063=DIRECTION('',(0.,0.,-1.));
#14064=DIRECTION('',(0.,-1.,0.));
#14065=DIRECTION('',(0.,0.,1.));
#14066=DIRECTION('center_axis',(0.,1.,0.));
#14067=DIRECTION('ref_axis',(0.,0.,1.));
#14068=DIRECTION('',(-3.29601953873307E-15,0.,1.));
#14069=DIRECTION('',(1.,0.,0.));
#14070=DIRECTION('',(0.,0.,1.));
#14071=DIRECTION('',(0.949699126201879,0.,0.313163806483743));
#14072=DIRECTION('',(0.313163806483743,0.,-0.949699126201879));
#14073=DIRECTION('',(0.949699126201879,0.,0.313163806483744));
#14074=DIRECTION('center_axis',(0.,1.,0.));
#14075=DIRECTION('ref_axis',(0.,0.,1.));
#14076=DIRECTION('',(3.49148133884313E-15,0.,-1.));
#14077=DIRECTION('center_axis',(0.,1.,0.));
#14078=DIRECTION('ref_axis',(0.,0.,1.));
#14079=DIRECTION('',(-0.313163806483747,0.,0.949699126201878));
#14080=DIRECTION('center_axis',(0.,-1.,0.));
#14081=DIRECTION('ref_axis',(-1.7762059938806E-15,0.,1.));
#14082=DIRECTION('center_axis',(0.,1.,0.));
#14083=DIRECTION('ref_axis',(0.,0.,1.));
#14084=DIRECTION('',(-0.313163806483743,0.,0.949699126201879));
#14085=DIRECTION('',(0.949699126201879,0.,0.313163806483743));
#14086=DIRECTION('',(-3.46944695195362E-15,0.,-1.));
#14087=DIRECTION('',(1.,0.,0.));
#14088=DIRECTION('',(-3.46944695195362E-15,0.,-1.));
#14089=DIRECTION('',(1.,0.,0.));
#14090=DIRECTION('center_axis',(0.,-1.,0.));
#14091=DIRECTION('ref_axis',(2.35106052273563E-14,0.,1.));
#14092=DIRECTION('',(-1.,0.,1.95461800110063E-16));
#14093=DIRECTION('center_axis',(0.,-1.,0.));
#14094=DIRECTION('ref_axis',(-1.30614473485313E-15,0.,1.));
#14095=DIRECTION('',(0.,0.,-1.));
#14096=DIRECTION('center_axis',(0.,-1.,0.));
#14097=DIRECTION('ref_axis',(0.,0.,1.));
#14098=DIRECTION('',(1.,0.,-1.95461800110063E-16));
#14099=DIRECTION('center_axis',(0.,-1.,0.));
#14100=DIRECTION('ref_axis',(0.,0.,1.));
#14101=DIRECTION('center_axis',(0.,1.,0.));
#14102=DIRECTION('ref_axis',(0.,0.,1.));
#14103=DIRECTION('',(-0.949699126201879,0.,-0.313163806483744));
#14104=DIRECTION('center_axis',(0.,-1.,0.));
#14105=DIRECTION('ref_axis',(0.,0.,1.));
#14106=DIRECTION('center_axis',(0.,1.,0.));
#14107=DIRECTION('ref_axis',(0.,0.,1.));
#14108=DIRECTION('',(-0.313163806483754,0.,0.949699126201876));
#14109=DIRECTION('center_axis',(0.,1.,0.));
#14110=DIRECTION('ref_axis',(0.,0.,1.));
#14111=DIRECTION('',(1.,0.,0.));
#14112=DIRECTION('center_axis',(0.,1.,0.));
#14113=DIRECTION('ref_axis',(0.,0.,1.));
#14114=DIRECTION('',(0.949699126201879,0.,0.313163806483744));
#14115=DIRECTION('center_axis',(0.,-1.,0.));
#14116=DIRECTION('ref_axis',(0.,0.,1.));
#14117=DIRECTION('',(0.313163806483747,0.,-0.949699126201878));
#14118=DIRECTION('center_axis',(0.,1.,0.));
#14119=DIRECTION('ref_axis',(0.,0.,1.));
#14120=DIRECTION('',(-1.,0.,0.));
#14121=DIRECTION('center_axis',(0.,-1.,0.));
#14122=DIRECTION('ref_axis',(0.,0.,1.));
#14123=DIRECTION('center_axis',(0.,1.,0.));
#14124=DIRECTION('ref_axis',(0.,0.,1.));
#14125=DIRECTION('',(-0.949699126201879,0.,-0.313163806483744));
#14126=DIRECTION('center_axis',(0.,1.,0.));
#14127=DIRECTION('ref_axis',(0.,0.,1.));
#14128=DIRECTION('',(0.,0.,1.));
#14129=DIRECTION('center_axis',(0.,1.,0.));
#14130=DIRECTION('ref_axis',(0.,0.,1.));
#14131=DIRECTION('',(0.313163806483754,0.,-0.949699126201876));
#14132=DIRECTION('center_axis',(0.,-1.,0.));
#14133=DIRECTION('ref_axis',(0.,0.,-1.));
#14134=DIRECTION('center_axis',(0.,1.,0.));
#14135=DIRECTION('ref_axis',(0.,0.,1.));
#14136=DIRECTION('center_axis',(0.,-1.,0.));
#14137=DIRECTION('ref_axis',(0.,0.,1.));
#14138=DIRECTION('center_axis',(0.,1.,0.));
#14139=DIRECTION('ref_axis',(0.,0.,1.));
#14140=DIRECTION('center_axis',(0.,-1.,0.));
#14141=DIRECTION('ref_axis',(0.,0.,-1.));
#14142=DIRECTION('center_axis',(0.,1.,0.));
#14143=DIRECTION('ref_axis',(0.,0.,-1.));
#14144=DIRECTION('center_axis',(0.,0.,1.));
#14145=DIRECTION('ref_axis',(1.,0.,0.));
#14146=DIRECTION('center_axis',(0.,0.,-1.));
#14147=DIRECTION('ref_axis',(-6.36384622448961E-5,0.999999997975073,0.));
#14148=DIRECTION('',(-1.,0.,0.));
#14149=DIRECTION('center_axis',(-3.53117861453752E-12,-8.13032267332511E-11,
-1.));
#14150=DIRECTION('ref_axis',(6.36387635293006E-5,0.999999997975054,-8.13034512884572E-11));
#14151=DIRECTION('center_axis',(1.,0.,0.));
#14152=DIRECTION('ref_axis',(0.,0.,-1.));
#14153=DIRECTION('center_axis',(-1.,8.324828000444E-11,3.61565657182464E-12));
#14154=DIRECTION('ref_axis',(8.32485099311225E-11,0.999999997975066,6.36385813081935E-5));
#14155=DIRECTION('',(0.,0.,-1.));
#14156=DIRECTION('center_axis',(-1.,8.28592693503832E-11,-3.59876098037523E-12));
#14157=DIRECTION('ref_axis',(8.28594982014715E-11,0.999999997975086,-6.36382556169485E-5));
#14158=DIRECTION('center_axis',(-0.707106781186547,0.,0.707106781186548));
#14159=DIRECTION('ref_axis',(0.707106781186548,0.,0.707106781186547));
#14160=DIRECTION('',(-0.707106781186548,0.,-0.707106781186547));
#14161=DIRECTION('',(0.707106781186548,0.,0.707106781186547));
#14162=DIRECTION('',(0.500076792314969,-0.706998163771264,0.500076792314972));
#14163=DIRECTION('center_axis',(0.707106781186548,0.,-0.707106781186547));
#14164=DIRECTION('ref_axis',(-0.707106781186547,0.,-0.707106781186548));
#14165=DIRECTION('',(0.707106781186547,0.,0.707106781186548));
#14166=DIRECTION('',(0.,1.,0.));
#14167=DIRECTION('',(-0.500076792314964,0.706998163771268,-0.500076792314971));
#14168=DIRECTION('',(-0.707106781186547,0.,-0.707106781186548));
#14169=DIRECTION('center_axis',(0.,-1.,0.));
#14170=DIRECTION('ref_axis',(0.,0.,-1.));
#14171=DIRECTION('',(0.,-1.,0.));
#14172=DIRECTION('center_axis',(0.,1.,0.));
#14173=DIRECTION('ref_axis',(0.,0.,1.));
#14174=DIRECTION('',(0.,-1.,0.));
#14175=DIRECTION('center_axis',(0.,-1.,0.));
#14176=DIRECTION('ref_axis',(0.,0.,-1.));
#14177=DIRECTION('center_axis',(0.,-1.,0.));
#14178=DIRECTION('ref_axis',(0.,0.,-1.));
#14179=DIRECTION('',(-0.949699126201879,0.,-0.313163806483744));
#14180=DIRECTION('center_axis',(0.,-1.,0.));
#14181=DIRECTION('ref_axis',(0.,0.,-1.));
#14182=DIRECTION('',(0.949699126201879,0.,0.313163806483744));
#14183=DIRECTION('center_axis',(0.,1.,0.));
#14184=DIRECTION('ref_axis',(0.,0.,-1.));
#14185=DIRECTION('center_axis',(0.313163806483744,0.,-0.949699126201879));
#14186=DIRECTION('ref_axis',(-0.949699126201879,0.,-0.313163806483744));
#14187=DIRECTION('',(-0.949699126201879,0.,-0.313163806483744));
#14188=DIRECTION('',(0.,-1.,0.));
#14189=DIRECTION('center_axis',(0.,-1.,0.));
#14190=DIRECTION('ref_axis',(0.,0.,-1.));
#14191=DIRECTION('',(-0.949699126201879,0.,-0.313163806483744));
#14192=DIRECTION('center_axis',(0.,-1.,0.));
#14193=DIRECTION('ref_axis',(0.,0.,-1.));
#14194=DIRECTION('',(0.949699126201879,0.,0.313163806483744));
#14195=DIRECTION('center_axis',(0.,1.,0.));
#14196=DIRECTION('ref_axis',(0.,0.,-1.));
#14197=DIRECTION('center_axis',(0.313163806483744,0.,-0.949699126201879));
#14198=DIRECTION('ref_axis',(-0.949699126201879,0.,-0.313163806483744));
#14199=DIRECTION('',(0.,1.,0.));
#14200=DIRECTION('',(0.949699126201879,0.,0.313163806483744));
#14201=DIRECTION('center_axis',(0.,1.,0.));
#14202=DIRECTION('ref_axis',(0.,0.,1.));
#14203=DIRECTION('center_axis',(0.,-1.,0.));
#14204=DIRECTION('ref_axis',(0.,0.,1.));
#14205=DIRECTION('',(0.,-1.,0.));
#14206=DIRECTION('center_axis',(0.,1.,0.));
#14207=DIRECTION('ref_axis',(0.,0.,1.));
#14208=DIRECTION('center_axis',(-1.,0.,0.));
#14209=DIRECTION('ref_axis',(0.,0.,1.));
#14210=DIRECTION('',(0.,1.,0.));
#14211=DIRECTION('',(0.,0.,1.));
#14212=DIRECTION('',(0.,0.,-1.));
#14213=DIRECTION('center_axis',(1.03892784411108E-15,0.,-1.));
#14214=DIRECTION('ref_axis',(-1.,0.,-1.03892784411108E-15));
#14215=DIRECTION('',(0.,1.,0.));
#14216=DIRECTION('',(-1.,0.,-1.03892784411108E-15));
#14217=DIRECTION('',(0.,-1.,0.));
#14218=DIRECTION('',(1.,0.,1.03892784411108E-15));
#14219=DIRECTION('center_axis',(0.,1.,0.));
#14220=DIRECTION('ref_axis',(0.,0.,1.));
#14221=DIRECTION('center_axis',(0.,1.,0.));
#14222=DIRECTION('ref_axis',(0.,0.,1.));
#14223=DIRECTION('',(0.,0.,1.));
#14224=DIRECTION('center_axis',(0.,-1.,0.));
#14225=DIRECTION('ref_axis',(0.,0.,1.));
#14226=DIRECTION('center_axis',(0.,1.,0.));
#14227=DIRECTION('ref_axis',(0.,0.,1.));
#14228=DIRECTION('',(-1.,0.,-1.03892784411108E-15));
#14229=DIRECTION('center_axis',(0.,1.,0.));
#14230=DIRECTION('ref_axis',(0.,0.,1.));
#14231=DIRECTION('center_axis',(0.,1.,0.));
#14232=DIRECTION('ref_axis',(0.,0.,1.));
#14233=DIRECTION('center_axis',(0.,-1.,0.));
#14234=DIRECTION('ref_axis',(-3.70074341541718E-15,0.,1.));
#14235=DIRECTION('center_axis',(0.,1.,0.));
#14236=DIRECTION('ref_axis',(0.,0.,1.));
#14237=DIRECTION('center_axis',(0.,1.,0.));
#14238=DIRECTION('ref_axis',(-0.453742606486518,0.,-0.891132788679005));
#14239=DIRECTION('center_axis',(0.,-1.,0.));
#14240=DIRECTION('ref_axis',(0.,0.,1.));
#14241=DIRECTION('center_axis',(0.,1.,0.));
#14242=DIRECTION('ref_axis',(0.,0.,1.));
#14243=DIRECTION('center_axis',(0.,1.,0.));
#14244=DIRECTION('ref_axis',(0.,0.,1.));
#14245=DIRECTION('center_axis',(0.,-1.,0.));
#14246=DIRECTION('ref_axis',(7.40148683083437E-15,0.,1.));
#14247=DIRECTION('center_axis',(0.,1.,0.));
#14248=DIRECTION('ref_axis',(0.,0.,1.));
#14249=DIRECTION('center_axis',(0.,-1.,0.));
#14250=DIRECTION('ref_axis',(1.,0.,3.49155068656687E-15));
#14251=DIRECTION('center_axis',(0.,1.,0.));
#14252=DIRECTION('ref_axis',(-2.22044698990993E-14,0.,-1.));
#14253=DIRECTION('center_axis',(0.958065765674362,0.0292578032189066,0.285050819317542));
#14254=DIRECTION('ref_axis',(0.219693026012008,-0.713664621834887,-0.665144932975479));
#14255=DIRECTION('center_axis',(0.,1.,0.));
#14256=DIRECTION('ref_axis',(0.,0.,1.));
#14257=DIRECTION('center_axis',(0.,-1.,0.));
#14258=DIRECTION('ref_axis',(0.,0.,-1.));
#14259=DIRECTION('center_axis',(0.956900850725464,0.0248003127102221,0.289353946526324));
#14260=DIRECTION('ref_axis',(0.183332141415881,0.721139318485221,-0.668092365813694));
#14261=DIRECTION('center_axis',(0.949699126201878,0.,0.313163806483747));
#14262=DIRECTION('ref_axis',(0.313163806483747,0.,-0.949699126201878));
#14263=DIRECTION('',(0.,1.,0.));
#14264=DIRECTION('',(0.313163806483747,0.,-0.949699126201878));
#14265=DIRECTION('',(0.,-1.,0.));
#14266=DIRECTION('',(0.313163806483747,0.,-0.949699126201878));
#14267=DIRECTION('center_axis',(-0.949699126194824,2.35739471213281E-11,
-0.313163806505138));
#14268=DIRECTION('ref_axis',(0.21701115590481,0.72097245765419,-0.658107038039357));
#14269=DIRECTION('',(-0.313163806483747,0.,0.949699126201878));
#14270=DIRECTION('center_axis',(0.949699126201878,0.,0.313163806483747));
#14271=DIRECTION('ref_axis',(0.313163806483747,0.,-0.949699126201878));
#14272=DIRECTION('',(-0.313163806483747,0.,0.949699126201878));
#14273=DIRECTION('',(0.,-1.,0.));
#14274=DIRECTION('',(0.313163806483747,0.,-0.949699126201878));
#14275=DIRECTION('center_axis',(0.949699126207133,1.83236368242976E-11,
0.31316380646781));
#14276=DIRECTION('ref_axis',(0.211605671956001,0.737174116650109,-0.64171439234069));
#14277=DIRECTION('',(-0.313163806483747,0.,0.949699126201878));
#14278=DIRECTION('center_axis',(0.,-1.,0.));
#14279=DIRECTION('ref_axis',(1.,0.,3.49155068656687E-15));
#14280=DIRECTION('center_axis',(0.,1.,0.));
#14281=DIRECTION('ref_axis',(0.,0.,1.));
#14282=DIRECTION('center_axis',(0.,1.,0.));
#14283=DIRECTION('ref_axis',(-1.95400113482291E-14,0.,-1.));
#14284=DIRECTION('center_axis',(-0.954264865962622,-0.0150877408549486,
-0.29858152264538));
#14285=DIRECTION('ref_axis',(0.191637949226221,0.735684127227363,-0.649648952405898));
#14286=DIRECTION('center_axis',(0.,-1.,0.));
#14287=DIRECTION('ref_axis',(0.,0.,-1.));
#14288=DIRECTION('center_axis',(0.,1.,0.));
#14289=DIRECTION('ref_axis',(1.,0.,1.59271860898362E-15));
#14290=DIRECTION('',(0.,1.,0.));
#14291=DIRECTION('center_axis',(0.,-1.,0.));
#14292=DIRECTION('ref_axis',(0.,0.,1.));
#14293=DIRECTION('',(0.,-1.,0.));
#14294=DIRECTION('center_axis',(0.,1.,0.));
#14295=DIRECTION('ref_axis',(0.,0.,1.));
#14296=DIRECTION('center_axis',(0.,1.,0.));
#14297=DIRECTION('ref_axis',(1.,0.,5.39036164761359E-15));
#14298=DIRECTION('',(-0.500130397801065,-0.706999113223837,-0.500021838619131));
#14299=DIRECTION('center_axis',(0.,1.,0.));
#14300=DIRECTION('ref_axis',(0.,0.,1.));
#14301=DIRECTION('',(0.500130397801061,0.706999113223842,-0.500021838619127));
#14302=DIRECTION('center_axis',(0.,-1.,0.));
#14303=DIRECTION('ref_axis',(3.55276338872479E-15,0.,1.));
#14304=DIRECTION('center_axis',(0.,-1.,0.));
#14305=DIRECTION('ref_axis',(-1.7763816943624E-15,0.,1.));
#14306=DIRECTION('center_axis',(0.,-1.,0.));
#14307=DIRECTION('ref_axis',(1.,0.,3.49148133884313E-15));
#14308=DIRECTION('',(3.29601953873307E-15,0.,-1.));
#14309=DIRECTION('center_axis',(0.,1.,0.));
#14310=DIRECTION('ref_axis',(1.56737368182375E-14,0.,-1.));
#14311=DIRECTION('',(-1.,0.,1.95461800110063E-16));
#14312=DIRECTION('center_axis',(0.,-1.,0.));
#14313=DIRECTION('ref_axis',(0.,0.,-1.));
#14314=DIRECTION('',(0.707106781186551,0.,-0.707106781186544));
#14315=DIRECTION('',(-0.707106781186549,0.,0.707106781186546));
#14316=DIRECTION('center_axis',(0.,-1.,0.));
#14317=DIRECTION('ref_axis',(0.,0.,-1.));
#14318=DIRECTION('center_axis',(0.,1.,0.));
#14319=DIRECTION('ref_axis',(-1.,0.,-3.49148133884313E-15));
#14320=DIRECTION('',(1.,0.,-1.95461800110063E-16));
#14321=DIRECTION('center_axis',(0.,-1.,0.));
#14322=DIRECTION('ref_axis',(0.,0.,1.));
#14323=DIRECTION('',(-3.29601953873307E-15,0.,1.));
#14324=DIRECTION('center_axis',(0.,1.,0.));
#14325=DIRECTION('ref_axis',(0.,0.,1.));
#14326=DIRECTION('',(0.707106781186549,0.,-0.707106781186546));
#14327=DIRECTION('center_axis',(0.,1.,0.));
#14328=DIRECTION('ref_axis',(0.,0.,1.));
#14329=DIRECTION('',(-0.707106781186551,0.,0.707106781186544));
#14330=DIRECTION('center_axis',(0.,1.,0.));
#14331=DIRECTION('ref_axis',(0.,0.,1.));
#14332=DIRECTION('center_axis',(-1.,0.,-3.29601953873307E-15));
#14333=DIRECTION('ref_axis',(-3.29601953873307E-15,0.,1.));
#14334=DIRECTION('',(-3.29601953873307E-15,0.,1.));
#14335=DIRECTION('',(0.,-1.,0.));
#14336=DIRECTION('',(3.29601953873307E-15,0.,-1.));
#14337=DIRECTION('',(0.,-1.,0.));
#14338=DIRECTION('',(-3.29601953873307E-15,0.,1.));
#14339=DIRECTION('center_axis',(0.,-1.,0.));
#14340=DIRECTION('ref_axis',(1.,0.,3.70074341541719E-15));
#14341=DIRECTION('center_axis',(0.,-1.,0.));
#14342=DIRECTION('ref_axis',(0.,0.,-1.));
#14343=DIRECTION('center_axis',(0.,1.,0.));
#14344=DIRECTION('ref_axis',(0.,0.,1.));
#14345=DIRECTION('center_axis',(-1.,0.,-3.29601953873307E-15));
#14346=DIRECTION('ref_axis',(-3.29601953873307E-15,0.,1.));
#14347=DIRECTION('',(-3.29601953873307E-15,0.,1.));
#14348=DIRECTION('',(0.,-1.,0.));
#14349=DIRECTION('',(3.29601953873307E-15,0.,-1.));
#14350=DIRECTION('',(3.29601953873307E-15,0.,-1.));
#14351=DIRECTION('',(0.,-1.,0.));
#14352=DIRECTION('center_axis',(0.,-1.,0.));
#14353=DIRECTION('ref_axis',(1.,0.,3.70074341541719E-15));
#14354=DIRECTION('center_axis',(0.,1.,0.));
#14355=DIRECTION('ref_axis',(0.,0.,1.));
#14356=DIRECTION('center_axis',(0.,-1.,0.));
#14357=DIRECTION('ref_axis',(0.,0.,1.));
#14358=DIRECTION('center_axis',(0.,1.,0.));
#14359=DIRECTION('ref_axis',(-1.,0.,-3.49151141721823E-15));
#14360=DIRECTION('center_axis',(0.,-1.,0.));
#14361=DIRECTION('ref_axis',(0.,0.,-1.));
#14362=DIRECTION('center_axis',(0.,1.,0.));
#14363=DIRECTION('ref_axis',(1.77631540548237E-15,0.,-1.));
#14364=DIRECTION('center_axis',(-1.,0.,-3.49148133884313E-15));
#14365=DIRECTION('ref_axis',(-3.49148133884313E-15,0.,1.));
#14366=DIRECTION('center_axis',(1.,-1.94413658113135E-13,1.26716935928603E-14));
#14367=DIRECTION('ref_axis',(1.94414464126846E-13,0.999999997975072,-6.36384851394666E-5));
#14368=DIRECTION('',(3.49148133884313E-15,0.,-1.));
#14369=DIRECTION('center_axis',(1.,-8.26648556920426E-11,-3.58608928677283E-12));
#14370=DIRECTION('ref_axis',(8.26650837388721E-11,0.999999997975055,6.36387448952208E-5));
#14371=DIRECTION('center_axis',(-0.707106781186546,0.,-0.707106781186549));
#14372=DIRECTION('ref_axis',(-0.707106781186549,0.,0.707106781186546));
#14373=DIRECTION('',(0.707106781186549,0.,-0.707106781186546));
#14374=DIRECTION('',(-0.707106781186549,0.,0.707106781186546));
#14375=DIRECTION('',(-0.50007679231497,-0.706998163771266,0.50007679231497));
#14376=DIRECTION('',(0.,-1.,0.));
#14377=DIRECTION('center_axis',(0.707106781186544,0.,0.707106781186551));
#14378=DIRECTION('ref_axis',(0.707106781186551,0.,-0.707106781186544));
#14379=DIRECTION('',(-0.707106781186551,0.,0.707106781186544));
#14380=DIRECTION('',(0.50007679231497,0.70699816377127,-0.500076792314963));
#14381=DIRECTION('',(0.707106781186551,0.,-0.707106781186544));
#14382=DIRECTION('center_axis',(0.,-1.,0.));
#14383=DIRECTION('ref_axis',(1.,0.,3.49175053950189E-15));
#14384=DIRECTION('',(0.,-1.,0.));
#14385=DIRECTION('center_axis',(0.,1.,0.));
#14386=DIRECTION('ref_axis',(0.,0.,1.));
#14387=DIRECTION('center_axis',(0.,-1.,0.));
#14388=DIRECTION('ref_axis',(0.,0.,-1.));
#14389=DIRECTION('center_axis',(0.,-1.,0.));
#14390=DIRECTION('ref_axis',(1.,0.,3.49148133884313E-15));
#14391=DIRECTION('',(0.313163806483747,0.,-0.949699126201878));
#14392=DIRECTION('center_axis',(0.,-1.,0.));
#14393=DIRECTION('ref_axis',(0.,0.,-1.));
#14394=DIRECTION('',(-0.313163806483747,0.,0.949699126201878));
#14395=DIRECTION('center_axis',(0.,1.,0.));
#14396=DIRECTION('ref_axis',(6.75015932572764E-14,0.,-1.));
#14397=DIRECTION('center_axis',(0.949699126201878,0.,0.313163806483747));
#14398=DIRECTION('ref_axis',(0.313163806483747,0.,-0.949699126201878));
#14399=DIRECTION('',(0.313163806483747,0.,-0.949699126201878));
#14400=DIRECTION('',(0.,-1.,0.));
#14401=DIRECTION('center_axis',(0.,-1.,0.));
#14402=DIRECTION('ref_axis',(1.,0.,3.49148133884313E-15));
#14403=DIRECTION('',(0.313163806483747,0.,-0.949699126201878));
#14404=DIRECTION('center_axis',(0.,-1.,0.));
#14405=DIRECTION('ref_axis',(0.,0.,-1.));
#14406=DIRECTION('',(-0.313163806483747,0.,0.949699126201878));
#14407=DIRECTION('center_axis',(0.,1.,0.));
#14408=DIRECTION('ref_axis',(3.73035047474275E-14,0.,-1.));
#14409=DIRECTION('center_axis',(0.949699126201878,0.,0.313163806483747));
#14410=DIRECTION('ref_axis',(0.313163806483747,0.,-0.949699126201878));
#14411=DIRECTION('',(0.,1.,0.));
#14412=DIRECTION('',(-0.313163806483747,0.,0.949699126201878));
#14413=DIRECTION('center_axis',(0.,1.,0.));
#14414=DIRECTION('ref_axis',(-1.,0.,-3.49137740498798E-15));
#14415=DIRECTION('center_axis',(0.,-1.,0.));
#14416=DIRECTION('ref_axis',(-3.55273339156727E-15,0.,1.));
#14417=DIRECTION('',(0.,-1.,0.));
#14418=DIRECTION('center_axis',(0.,1.,0.));
#14419=DIRECTION('ref_axis',(0.,0.,1.));
#14420=DIRECTION('center_axis',(3.49148133884313E-15,0.,-1.));
#14421=DIRECTION('ref_axis',(-1.,0.,-3.49148133884313E-15));
#14422=DIRECTION('',(0.,1.,0.));
#14423=DIRECTION('',(-1.,0.,-3.49148133884313E-15));
#14424=DIRECTION('',(1.,0.,3.49148133884313E-15));
#14425=DIRECTION('center_axis',(1.,0.,4.53040918295421E-15));
#14426=DIRECTION('ref_axis',(4.53040918295421E-15,0.,-1.));
#14427=DIRECTION('',(0.,1.,0.));
#14428=DIRECTION('',(4.53040918295421E-15,0.,-1.));
#14429=DIRECTION('',(0.,-1.,0.));
#14430=DIRECTION('',(-4.53040918295421E-15,0.,1.));
#14431=DIRECTION('center_axis',(0.,1.,0.));
#14432=DIRECTION('ref_axis',(-1.,0.,-3.49148133884313E-15));
#14433=DIRECTION('center_axis',(0.,1.,0.));
#14434=DIRECTION('ref_axis',(0.,0.,1.));
#14435=DIRECTION('',(-1.,0.,-3.49148133884313E-15));
#14436=DIRECTION('center_axis',(0.,1.,0.));
#14437=DIRECTION('ref_axis',(0.,0.,1.));
#14438=DIRECTION('center_axis',(0.,-1.,0.));
#14439=DIRECTION('ref_axis',(-3.55275288159092E-15,0.,1.));
#14440=DIRECTION('',(4.53040918295421E-15,0.,-1.));
#14441=DIRECTION('center_axis',(0.,1.,0.));
#14442=DIRECTION('ref_axis',(0.,0.,1.));
#14443=DIRECTION('center_axis',(0.,1.,0.));
#14444=DIRECTION('ref_axis',(-1.,0.,-3.70074341541718E-15));
#14445=DIRECTION('center_axis',(0.,1.,0.));
#14446=DIRECTION('ref_axis',(0.891132788679008,0.,-0.453742606486513));
#14447=DIRECTION('center_axis',(0.,-1.,0.));
#14448=DIRECTION('ref_axis',(0.,0.,1.));
#14449=DIRECTION('center_axis',(0.,1.,0.));
#14450=DIRECTION('ref_axis',(0.,0.,1.));
#14451=DIRECTION('center_axis',(0.,1.,0.));
#14452=DIRECTION('ref_axis',(-1.,0.,0.));
#14453=DIRECTION('center_axis',(0.,-1.,0.));
#14454=DIRECTION('ref_axis',(0.,0.,1.));
#14455=DIRECTION('center_axis',(0.,1.,0.));
#14456=DIRECTION('ref_axis',(0.,0.,1.));
#14457=DIRECTION('center_axis',(0.,-1.,0.));
#14458=DIRECTION('ref_axis',(0.,0.,1.));
#14459=DIRECTION('center_axis',(0.,1.,0.));
#14460=DIRECTION('ref_axis',(0.,0.,-1.));
#14461=DIRECTION('center_axis',(-0.285050819317539,0.0292578032188915,0.958065765674363));
#14462=DIRECTION('ref_axis',(0.665144932827453,-0.713664621985,0.219693025972537));
#14463=DIRECTION('center_axis',(0.,1.,0.));
#14464=DIRECTION('ref_axis',(0.,0.,1.));
#14465=DIRECTION('center_axis',(0.,-1.,0.));
#14466=DIRECTION('ref_axis',(0.,0.,-1.));
#14467=DIRECTION('center_axis',(-0.289353946523101,0.0248003127138381,0.956900850726345));
#14468=DIRECTION('ref_axis',(0.668092365814573,0.72113931848567,0.183332141410909));
#14469=DIRECTION('center_axis',(-0.313163806483744,0.,0.949699126201879));
#14470=DIRECTION('ref_axis',(0.949699126201879,0.,0.313163806483744));
#14471=DIRECTION('',(-0.949699126201879,0.,-0.313163806483744));
#14472=DIRECTION('',(0.,1.,0.));
#14473=DIRECTION('',(0.949699126201879,0.,0.313163806483744));
#14474=DIRECTION('',(0.,-1.,0.));
#14475=DIRECTION('',(0.949699126201879,0.,0.313163806483744));
#14476=DIRECTION('center_axis',(0.313163806486104,2.55945706169953E-12,
-0.949699126201101));
#14477=DIRECTION('ref_axis',(0.658107038053724,0.720972457648934,0.217011155878702));
#14478=DIRECTION('center_axis',(-0.313163806483744,0.,0.949699126201879));
#14479=DIRECTION('ref_axis',(0.949699126201879,0.,0.313163806483744));
#14480=DIRECTION('',(0.,1.,0.));
#14481=DIRECTION('',(-0.949699126201879,0.,-0.313163806483744));
#14482=DIRECTION('',(0.,-1.,0.));
#14483=DIRECTION('',(0.949699126201879,0.,0.313163806483744));
#14484=DIRECTION('center_axis',(-0.313163806482752,1.15972384695759E-12,
0.949699126202206));
#14485=DIRECTION('ref_axis',(0.641714392333106,0.737174116650406,0.211605671977966));
#14486=DIRECTION('',(-0.949699126201879,0.,-0.313163806483744));
#14487=DIRECTION('center_axis',(0.,-1.,0.));
#14488=DIRECTION('ref_axis',(0.,0.,1.));
#14489=DIRECTION('center_axis',(0.,1.,0.));
#14490=DIRECTION('ref_axis',(0.,0.,1.));
#14491=DIRECTION('center_axis',(0.,1.,0.));
#14492=DIRECTION('ref_axis',(0.,0.,-1.));
#14493=DIRECTION('center_axis',(0.298581521665074,-0.0150877419673539,-0.954264866251763));
#14494=DIRECTION('ref_axis',(0.649648952857147,0.735684127204403,0.191637947784642));
#14495=DIRECTION('center_axis',(0.,-1.,0.));
#14496=DIRECTION('ref_axis',(0.,0.,-1.));
#14497=DIRECTION('center_axis',(0.,1.,0.));
#14498=DIRECTION('ref_axis',(-5.20660583828602E-15,0.,1.));
#14499=DIRECTION('',(0.,1.,0.));
#14500=DIRECTION('',(0.,-1.,0.));
#14501=DIRECTION('center_axis',(0.,1.,0.));
#14502=DIRECTION('ref_axis',(-1.12246949261663E-14,0.,1.));
#14503=DIRECTION('',(0.500021838619129,-0.706999113223846,-0.500130397801055));
#14504=DIRECTION('',(0.500021838619127,0.706999113223842,0.500130397801061));
#14505=DIRECTION('center_axis',(0.,-1.,0.));
#14506=DIRECTION('ref_axis',(3.55276338872479E-15,0.,1.));
#14507=DIRECTION('center_axis',(0.,-1.,0.));
#14508=DIRECTION('ref_axis',(0.,0.,1.));
#14509=DIRECTION('center_axis',(-1.95461800110063E-16,0.,-1.));
#14510=DIRECTION('ref_axis',(-1.,0.,1.95461800110063E-16));
#14511=DIRECTION('',(-1.,0.,1.95461800110063E-16));
#14512=DIRECTION('',(0.,-1.,0.));
#14513=DIRECTION('',(1.,0.,-1.95461800110063E-16));
#14514=DIRECTION('',(0.,-1.,0.));
#14515=DIRECTION('',(-1.,0.,1.95461800110063E-16));
#14516=DIRECTION('center_axis',(0.,-1.,0.));
#14517=DIRECTION('ref_axis',(0.,0.,1.));
#14518=DIRECTION('center_axis',(0.,-1.,0.));
#14519=DIRECTION('ref_axis',(0.,0.,-1.));
#14520=DIRECTION('center_axis',(0.,1.,0.));
#14521=DIRECTION('ref_axis',(0.,0.,1.));
#14522=DIRECTION('center_axis',(-1.95461800110063E-16,0.,-1.));
#14523=DIRECTION('ref_axis',(-1.,0.,1.95461800110063E-16));
#14524=DIRECTION('',(0.,-1.,0.));
#14525=DIRECTION('',(1.,0.,-1.95461800110063E-16));
#14526=DIRECTION('',(1.,0.,-1.95461800110063E-16));
#14527=DIRECTION('',(0.,-1.,0.));
#14528=DIRECTION('',(-1.,0.,1.95461800110063E-16));
#14529=DIRECTION('center_axis',(0.,-1.,0.));
#14530=DIRECTION('ref_axis',(0.,0.,1.));
#14531=DIRECTION('center_axis',(0.,1.,0.));
#14532=DIRECTION('ref_axis',(0.,0.,1.));
#14533=DIRECTION('center_axis',(0.,-1.,0.));
#14534=DIRECTION('ref_axis',(2.34380416309755E-14,0.,1.));
#14535=DIRECTION('center_axis',(0.,1.,0.));
#14536=DIRECTION('ref_axis',(0.,0.,-1.));
#14537=DIRECTION('center_axis',(0.,-1.,0.));
#14538=DIRECTION('ref_axis',(0.,0.,-1.));
#14539=DIRECTION('center_axis',(0.,1.,0.));
#14540=DIRECTION('ref_axis',(-1.77631540548237E-15,0.,-1.));
#14541=DIRECTION('center_axis',(0.,0.,-1.));
#14542=DIRECTION('ref_axis',(-1.,0.,0.));
#14543=DIRECTION('center_axis',(-3.61565657183125E-12,-8.32482800045515E-11,
1.));
#14544=DIRECTION('ref_axis',(-6.3638448448845E-5,-0.999999997975074,-8.32485099307542E-11));
#14545=DIRECTION('',(1.,0.,0.));
#14546=DIRECTION('center_axis',(3.58186538890928E-12,-8.24702586959293E-11,
1.));
#14547=DIRECTION('ref_axis',(6.36387679980598E-5,-0.999999997975054,-8.2470486474432E-11));
#14548=DIRECTION('center_axis',(0.707106781186547,0.,-0.707106781186548));
#14549=DIRECTION('ref_axis',(-0.707106781186548,0.,-0.707106781186547));
#14550=DIRECTION('',(0.707106781186548,0.,0.707106781186547));
#14551=DIRECTION('',(-0.707106781186548,0.,-0.707106781186547));
#14552=DIRECTION('',(-0.500076792314973,-0.706998163771266,-0.500076792314966));
#14553=DIRECTION('',(0.,-1.,0.));
#14554=DIRECTION('center_axis',(-0.707106781186548,0.,0.707106781186547));
#14555=DIRECTION('ref_axis',(0.707106781186547,0.,0.707106781186548));
#14556=DIRECTION('',(-0.707106781186547,0.,-0.707106781186548));
#14557=DIRECTION('',(0.,1.,0.));
#14558=DIRECTION('',(0.500076792314966,0.706998163771266,0.500076792314973));
#14559=DIRECTION('',(0.707106781186547,0.,0.707106781186548));
#14560=DIRECTION('center_axis',(0.,-1.,0.));
#14561=DIRECTION('ref_axis',(0.,0.,1.));
#14562=DIRECTION('',(0.,-1.,0.));
#14563=DIRECTION('center_axis',(0.,1.,0.));
#14564=DIRECTION('ref_axis',(0.,0.,1.));
#14565=DIRECTION('center_axis',(0.,-1.,0.));
#14566=DIRECTION('ref_axis',(0.,0.,-1.));
#14567=DIRECTION('center_axis',(0.,-1.,0.));
#14568=DIRECTION('ref_axis',(0.,0.,1.));
#14569=DIRECTION('',(0.949699126201879,0.,0.313163806483744));
#14570=DIRECTION('center_axis',(0.,-1.,0.));
#14571=DIRECTION('ref_axis',(0.,0.,-1.));
#14572=DIRECTION('',(-0.949699126201879,0.,-0.313163806483744));
#14573=DIRECTION('center_axis',(0.,1.,0.));
#14574=DIRECTION('ref_axis',(0.,0.,-1.));
#14575=DIRECTION('center_axis',(-0.313163806483744,0.,0.949699126201879));
#14576=DIRECTION('ref_axis',(0.949699126201879,0.,0.313163806483744));
#14577=DIRECTION('',(0.949699126201879,0.,0.313163806483744));
#14578=DIRECTION('',(0.,-1.,0.));
#14579=DIRECTION('center_axis',(0.,-1.,0.));
#14580=DIRECTION('ref_axis',(0.,0.,1.));
#14581=DIRECTION('',(0.949699126201879,0.,0.313163806483744));
#14582=DIRECTION('center_axis',(0.,-1.,0.));
#14583=DIRECTION('ref_axis',(0.,0.,-1.));
#14584=DIRECTION('',(-0.949699126201879,0.,-0.313163806483744));
#14585=DIRECTION('center_axis',(0.,1.,0.));
#14586=DIRECTION('ref_axis',(-5.50671843416529E-14,0.,-1.));
#14587=DIRECTION('center_axis',(-0.313163806483744,0.,0.949699126201879));
#14588=DIRECTION('ref_axis',(0.949699126201879,0.,0.313163806483744));
#14589=DIRECTION('',(-0.949699126201879,0.,-0.313163806483744));
#14590=DIRECTION('center_axis',(0.,1.,0.));
#14591=DIRECTION('ref_axis',(0.,0.,-1.));
#14592=DIRECTION('center_axis',(0.,-1.,0.));
#14593=DIRECTION('ref_axis',(1.77636669578364E-15,0.,1.));
#14594=DIRECTION('',(0.,-1.,0.));
#14595=DIRECTION('center_axis',(0.,1.,0.));
#14596=DIRECTION('ref_axis',(0.,0.,1.));
#14597=DIRECTION('center_axis',(1.,0.,0.));
#14598=DIRECTION('ref_axis',(0.,0.,-1.));
#14599=DIRECTION('',(0.,0.,1.));
#14600=DIRECTION('',(0.,1.,0.));
#14601=DIRECTION('',(0.,0.,-1.));
#14602=DIRECTION('center_axis',(-1.03892784411108E-15,0.,1.));
#14603=DIRECTION('ref_axis',(1.,0.,1.03892784411108E-15));
#14604=DIRECTION('',(0.,1.,0.));
#14605=DIRECTION('',(1.,0.,1.03892784411108E-15));
#14606=DIRECTION('',(0.,-1.,0.));
#14607=DIRECTION('',(-1.,0.,-1.03892784411108E-15));
#14608=DIRECTION('center_axis',(0.,1.,0.));
#14609=DIRECTION('ref_axis',(0.,0.,-1.));
#14610=DIRECTION('',(-1.,0.,0.));
#14611=DIRECTION('',(0.,0.,-1.));
#14612=DIRECTION('center_axis',(0.,1.,0.));
#14613=DIRECTION('ref_axis',(0.,0.,1.));
#14614=DIRECTION('center_axis',(0.,-1.,0.));
#14615=DIRECTION('ref_axis',(3.55275288159092E-15,0.,1.));
#14616=DIRECTION('center_axis',(0.,1.,0.));
#14617=DIRECTION('ref_axis',(0.,0.,1.));
#14618=DIRECTION('',(1.,0.,1.03892784411108E-15));
#14619=DIRECTION('center_axis',(0.,1.,0.));
#14620=DIRECTION('ref_axis',(0.,0.,1.));
#14621=DIRECTION('center_axis',(0.,-1.,0.));
#14622=DIRECTION('ref_axis',(1.48029736616688E-15,0.,1.));
#14623=DIRECTION('',(-1.,0.,0.));
#14624=DIRECTION('',(3.46944695195362E-15,0.,1.));
#14625=DIRECTION('center_axis',(0.,1.,0.));
#14626=DIRECTION('ref_axis',(0.,0.,-1.));
#14627=DIRECTION('center_axis',(0.,-1.,0.));
#14628=DIRECTION('ref_axis',(0.,0.,1.));
#14629=DIRECTION('center_axis',(0.,1.,0.));
#14630=DIRECTION('ref_axis',(0.,0.,1.));
#14631=DIRECTION('center_axis',(0.,1.,0.));
#14632=DIRECTION('ref_axis',(0.453742606486519,0.,0.891132788679005));
#14633=DIRECTION('center_axis',(0.,1.,0.));
#14634=DIRECTION('ref_axis',(0.,0.,-1.));
#14635=DIRECTION('center_axis',(0.,-1.,0.));
#14636=DIRECTION('ref_axis',(-7.40148683083437E-15,0.,1.));
#14637=DIRECTION('center_axis',(0.,1.,0.));
#14638=DIRECTION('ref_axis',(0.,0.,1.));
#14639=DIRECTION('center_axis',(0.,-1.,0.));
#14640=DIRECTION('ref_axis',(-1.,0.,-1.04743722655916E-14));
#14641=DIRECTION('center_axis',(0.,1.,0.));
#14642=DIRECTION('ref_axis',(3.90797794557653E-14,0.,-1.));
#14643=DIRECTION('center_axis',(-0.958065765673929,0.0292578032171867,-0.285050819319174));
#14644=DIRECTION('ref_axis',(0.219693026019329,0.713664621806868,-0.665144933003125));
#14645=DIRECTION('center_axis',(0.,1.,0.));
#14646=DIRECTION('ref_axis',(0.,0.,1.));
#14647=DIRECTION('center_axis',(0.,-1.,0.));
#14648=DIRECTION('ref_axis',(0.,0.,-1.));
#14649=DIRECTION('center_axis',(-0.956900850717379,0.024800312678508,-0.289353946555781));
#14650=DIRECTION('ref_axis',(-0.183332141458518,0.721139318485025,0.668092365802205));
#14651=DIRECTION('center_axis',(-0.949699126201876,0.,-0.313163806483754));
#14652=DIRECTION('ref_axis',(-0.313163806483754,0.,0.949699126201876));
#14653=DIRECTION('',(-0.313163806483754,0.,0.949699126201876));
#14654=DIRECTION('',(0.,-1.,0.));
#14655=DIRECTION('',(-0.313163806483754,0.,0.949699126201876));
#14656=DIRECTION('center_axis',(0.949699126200346,5.25362244862842E-12,
0.313163806488392));
#14657=DIRECTION('ref_axis',(-0.217011155881437,0.720972457651555,0.65810703804995));
#14658=DIRECTION('',(0.313163806483754,0.,-0.949699126201876));
#14659=DIRECTION('center_axis',(-0.949699126201876,0.,-0.313163806483754));
#14660=DIRECTION('ref_axis',(-0.313163806483754,0.,0.949699126201876));
#14661=DIRECTION('',(0.,1.,0.));
#14662=DIRECTION('',(0.313163806483754,0.,-0.949699126201876));
#14663=DIRECTION('',(-0.313163806483754,0.,0.949699126201876));
#14664=DIRECTION('center_axis',(-0.949699126201081,-2.78333723603669E-12,
-0.313163806486162));
#14665=DIRECTION('ref_axis',(-0.211605671983048,0.737174116650356,0.641714392331488));
#14666=DIRECTION('',(0.313163806483754,0.,-0.949699126201876));
#14667=DIRECTION('center_axis',(0.,-1.,0.));
#14668=DIRECTION('ref_axis',(-1.,0.,-1.04743722655916E-14));
#14669=DIRECTION('center_axis',(0.,1.,0.));
#14670=DIRECTION('ref_axis',(0.,0.,1.));
#14671=DIRECTION('center_axis',(0.,1.,0.));
#14672=DIRECTION('ref_axis',(0.,0.,-1.));
#14673=DIRECTION('center_axis',(0.954264863821462,-0.0150877326158706,0.298581529904847));
#14674=DIRECTION('ref_axis',(-0.191637959901166,0.735684127399272,0.649648949062253));
#14675=DIRECTION('center_axis',(0.,-1.,0.));
#14676=DIRECTION('ref_axis',(0.,0.,-1.));
#14677=DIRECTION('center_axis',(0.,-1.,0.));
#14678=DIRECTION('ref_axis',(-1.,0.,-1.04744440165294E-14));
#14679=DIRECTION('',(0.,0.,1.));
#14680=DIRECTION('center_axis',(0.,1.,0.));
#14681=DIRECTION('ref_axis',(0.,0.,-1.));
#14682=DIRECTION('',(1.,0.,-1.95461800110063E-16));
#14683=DIRECTION('center_axis',(0.,-1.,0.));
#14684=DIRECTION('ref_axis',(0.,0.,-1.));
#14685=DIRECTION('',(-0.707106781186556,0.,0.707106781186539));
#14686=DIRECTION('center_axis',(0.,-1.,0.));
#14687=DIRECTION('ref_axis',(0.,0.,-1.));
#14688=DIRECTION('',(0.707106781186554,0.,-0.707106781186541));
#14689=DIRECTION('center_axis',(0.,-1.,0.));
#14690=DIRECTION('ref_axis',(0.,0.,-1.));
#14691=DIRECTION('center_axis',(0.,1.,0.));
#14692=DIRECTION('ref_axis',(1.,0.,1.04744440165294E-14));
#14693=DIRECTION('',(-1.,0.,1.95461800110063E-16));
#14694=DIRECTION('center_axis',(0.,-1.,0.));
#14695=DIRECTION('ref_axis',(-1.30614473485313E-15,0.,1.));
#14696=DIRECTION('',(0.,0.,-1.));
#14697=DIRECTION('center_axis',(0.,1.,0.));
#14698=DIRECTION('ref_axis',(0.,0.,1.));
#14699=DIRECTION('',(-0.707106781186554,0.,0.707106781186541));
#14700=DIRECTION('',(0.707106781186556,0.,-0.707106781186539));
#14701=DIRECTION('center_axis',(0.,1.,0.));
#14702=DIRECTION('ref_axis',(0.,0.,1.));
#14703=DIRECTION('center_axis',(0.,-1.,0.));
#14704=DIRECTION('ref_axis',(-1.,0.,-9.86864910777917E-15));
#14705=DIRECTION('center_axis',(0.,-1.,0.));
#14706=DIRECTION('ref_axis',(0.,0.,-1.));
#14707=DIRECTION('center_axis',(0.,1.,0.));
#14708=DIRECTION('ref_axis',(0.,0.,1.));
#14709=DIRECTION('center_axis',(0.,-1.,0.));
#14710=DIRECTION('ref_axis',(-1.,0.,-9.86864910777917E-15));
#14711=DIRECTION('center_axis',(0.,1.,0.));
#14712=DIRECTION('ref_axis',(0.,0.,1.));
#14713=DIRECTION('center_axis',(0.,-1.,0.));
#14714=DIRECTION('ref_axis',(-1.2335811384724E-15,0.,1.));
#14715=DIRECTION('center_axis',(0.,1.,0.));
#14716=DIRECTION('ref_axis',(1.,0.,1.04745342516547E-14));
#14717=DIRECTION('center_axis',(0.,-1.,0.));
#14718=DIRECTION('ref_axis',(0.,0.,-1.));
#14719=DIRECTION('center_axis',(0.,1.,0.));
#14720=DIRECTION('ref_axis',(-1.77631540548237E-15,0.,-1.));
#14721=DIRECTION('center_axis',(0.707106781186541,0.,0.707106781186554));
#14722=DIRECTION('ref_axis',(0.707106781186554,0.,-0.707106781186541));
#14723=DIRECTION('',(-0.707106781186554,0.,0.707106781186541));
#14724=DIRECTION('',(0.707106781186554,0.,-0.707106781186541));
#14725=DIRECTION('',(0.500076792314976,-0.706998163771267,-0.500076792314961));
#14726=DIRECTION('',(0.,-1.,0.));
#14727=DIRECTION('center_axis',(-0.707106781186539,0.,-0.707106781186556));
#14728=DIRECTION('ref_axis',(-0.707106781186556,0.,0.707106781186539));
#14729=DIRECTION('',(0.707106781186556,0.,-0.707106781186539));
#14730=DIRECTION('',(0.,1.,0.));
#14731=DIRECTION('',(-0.500076792314971,0.706998163771271,0.50007679231496));
#14732=DIRECTION('',(-0.707106781186556,0.,0.707106781186539));
#14733=DIRECTION('center_axis',(0.,-1.,0.));
#14734=DIRECTION('ref_axis',(-1.,0.,-1.04746320744071E-14));
#14735=DIRECTION('center_axis',(0.,1.,0.));
#14736=DIRECTION('ref_axis',(0.,0.,1.));
#14737=DIRECTION('center_axis',(0.,-1.,0.));
#14738=DIRECTION('ref_axis',(0.,0.,-1.));
#14739=DIRECTION('center_axis',(0.,-1.,0.));
#14740=DIRECTION('ref_axis',(-1.,0.,-1.04744440165294E-14));
#14741=DIRECTION('',(-0.313163806483754,0.,0.949699126201876));
#14742=DIRECTION('center_axis',(0.,-1.,0.));
#14743=DIRECTION('ref_axis',(0.,0.,-1.));
#14744=DIRECTION('',(0.313163806483754,0.,-0.949699126201876));
#14745=DIRECTION('center_axis',(0.,1.,0.));
#14746=DIRECTION('ref_axis',(-2.84216649503149E-14,0.,-1.));
#14747=DIRECTION('center_axis',(-0.949699126201876,0.,-0.313163806483754));
#14748=DIRECTION('ref_axis',(-0.313163806483754,0.,0.949699126201876));
#14749=DIRECTION('',(-0.313163806483754,0.,0.949699126201876));
#14750=DIRECTION('center_axis',(0.,-1.,0.));
#14751=DIRECTION('ref_axis',(-1.,0.,-1.04744440165294E-14));
#14752=DIRECTION('',(-0.313163806483753,0.,0.949699126201876));
#14753=DIRECTION('center_axis',(0.,-1.,0.));
#14754=DIRECTION('ref_axis',(0.,0.,-1.));
#14755=DIRECTION('',(0.313163806483754,0.,-0.949699126201876));
#14756=DIRECTION('center_axis',(0.,1.,0.));
#14757=DIRECTION('ref_axis',(0.,0.,-1.));
#14758=DIRECTION('center_axis',(-0.949699126201876,0.,-0.313163806483753));
#14759=DIRECTION('ref_axis',(-0.313163806483754,0.,0.949699126201876));
#14760=DIRECTION('',(0.,1.,0.));
#14761=DIRECTION('',(0.313163806483753,0.,-0.949699126201876));
#14762=DIRECTION('center_axis',(0.,1.,0.));
#14763=DIRECTION('ref_axis',(1.,0.,1.04743786245486E-14));
#14764=DIRECTION('center_axis',(0.,-1.,0.));
#14765=DIRECTION('ref_axis',(0.,0.,1.));
#14766=DIRECTION('',(0.,-1.,0.));
#14767=DIRECTION('center_axis',(0.,1.,0.));
#14768=DIRECTION('ref_axis',(0.,0.,1.));
#14769=DIRECTION('center_axis',(-1.04744440165294E-14,0.,1.));
#14770=DIRECTION('ref_axis',(1.,0.,1.04744440165294E-14));
#14771=DIRECTION('',(0.,1.,0.));
#14772=DIRECTION('',(1.,0.,1.04744440165294E-14));
#14773=DIRECTION('',(-1.,0.,-1.04744440165294E-14));
#14774=DIRECTION('center_axis',(-1.,0.,-1.15133718606405E-14));
#14775=DIRECTION('ref_axis',(-1.15133718606405E-14,0.,1.));
#14776=DIRECTION('',(0.,1.,0.));
#14777=DIRECTION('',(-1.15133718606405E-14,0.,1.));
#14778=DIRECTION('',(0.,-1.,0.));
#14779=DIRECTION('',(1.15133718606405E-14,0.,-1.));
#14780=DIRECTION('center_axis',(0.,1.,0.));
#14781=DIRECTION('ref_axis',(1.,0.,1.04744440165294E-14));
#14782=DIRECTION('center_axis',(0.,-1.,0.));
#14783=DIRECTION('ref_axis',(0.,0.,1.));
#14784=DIRECTION('center_axis',(0.,1.,0.));
#14785=DIRECTION('ref_axis',(0.,0.,1.));
#14786=DIRECTION('',(1.,0.,1.04744440165294E-14));
#14787=DIRECTION('center_axis',(0.,1.,0.));
#14788=DIRECTION('ref_axis',(0.,0.,1.));
#14789=DIRECTION('center_axis',(0.,-1.,0.));
#14790=DIRECTION('ref_axis',(0.,0.,1.));
#14791=DIRECTION('center_axis',(0.,1.,0.));
#14792=DIRECTION('ref_axis',(0.,0.,1.));
#14793=DIRECTION('',(-1.15133718606405E-14,0.,1.));
#14794=DIRECTION('center_axis',(0.,1.,0.));
#14795=DIRECTION('ref_axis',(1.,0.,1.11022302462516E-14));
#14796=DIRECTION('center_axis',(0.,-1.,0.));
#14797=DIRECTION('ref_axis',(0.,0.,1.));
#14798=DIRECTION('center_axis',(0.,1.,0.));
#14799=DIRECTION('ref_axis',(0.,0.,1.));
#14800=DIRECTION('center_axis',(0.,1.,0.));
#14801=DIRECTION('ref_axis',(-0.891132788679008,0.,0.453742606486513));
#14802=DIRECTION('center_axis',(0.,-1.,0.));
#14803=DIRECTION('ref_axis',(-7.40148683083437E-15,0.,1.));
#14804=DIRECTION('center_axis',(0.,1.,0.));
#14805=DIRECTION('ref_axis',(0.,0.,1.));
#14806=DIRECTION('center_axis',(0.,1.,0.));
#14807=DIRECTION('ref_axis',(1.,0.,7.40148683083437E-15));
#14808=DIRECTION('center_axis',(0.,1.,0.));
#14809=DIRECTION('ref_axis',(0.707106781186556,0.,-0.707106781186539));
#14810=DIRECTION('center_axis',(-0.588235294117663,0.,0.808689828521608));
#14811=DIRECTION('ref_axis',(0.808689828521608,0.,0.588235294117663));
#14812=DIRECTION('center_axis',(0.,1.,0.));
#14813=DIRECTION('ref_axis',(0.,0.,1.));
#14814=DIRECTION('center_axis',(1.,0.,0.));
#14815=DIRECTION('ref_axis',(0.,0.,-1.));
#14816=DIRECTION('center_axis',(-1.,0.,-1.04744440165294E-14));
#14817=DIRECTION('ref_axis',(-1.04744440165294E-14,0.,1.));
#14818=DIRECTION('center_axis',(1.,0.,1.38777878078144E-14));
#14819=DIRECTION('ref_axis',(1.38777878078144E-14,0.,-1.));
#14820=DIRECTION('center_axis',(1.15133718606405E-14,0.,-1.));
#14821=DIRECTION('ref_axis',(-1.,0.,-1.15133718606405E-14));
#14822=DIRECTION('center_axis',(1.38777878078144E-14,0.,-1.));
#14823=DIRECTION('ref_axis',(-1.,0.,-1.38777878078144E-14));
#14824=DIRECTION('center_axis',(0.,1.,0.));
#14825=DIRECTION('ref_axis',(0.,0.,1.));
#14826=DIRECTION('center_axis',(-0.84916201117318,1.46586199943604E-14,
-0.528132444354937));
#14827=DIRECTION('ref_axis',(-0.528132444354937,1.80922966162518E-29,0.84916201117318));
#14828=DIRECTION('center_axis',(0.,1.,0.));
#14829=DIRECTION('ref_axis',(-0.274625188963796,0.,-0.961551353587836));
#14830=DIRECTION('center_axis',(0.528132444354927,0.,0.849162011173186));
#14831=DIRECTION('ref_axis',(0.849162011173186,0.,-0.528132444354927));
#14832=DIRECTION('center_axis',(0.,1.,0.));
#14833=DIRECTION('ref_axis',(0.,0.,1.));
#14834=DIRECTION('center_axis',(0.,1.,0.));
#14835=DIRECTION('ref_axis',(0.707106781186556,0.,-0.707106781186539));
#14836=DIRECTION('center_axis',(0.588235294117663,0.,-0.808689828521608));
#14837=DIRECTION('ref_axis',(-0.808689828521608,0.,-0.588235294117663));
#14838=DIRECTION('center_axis',(0.,1.,0.));
#14839=DIRECTION('ref_axis',(0.,0.,1.));
#14840=DIRECTION('center_axis',(-1.,0.,0.));
#14841=DIRECTION('ref_axis',(0.,0.,1.));
#14842=DIRECTION('center_axis',(1.,0.,1.04744440165294E-14));
#14843=DIRECTION('ref_axis',(1.04744440165294E-14,0.,-1.));
#14844=DIRECTION('center_axis',(-1.,0.,-1.38777878078144E-14));
#14845=DIRECTION('ref_axis',(-1.38777878078144E-14,0.,1.));
#14846=DIRECTION('center_axis',(-1.15133718606405E-14,0.,1.));
#14847=DIRECTION('ref_axis',(1.,0.,1.15133718606405E-14));
#14848=DIRECTION('center_axis',(-1.38777878078144E-14,-3.85185988877446E-28,
1.));
#14849=DIRECTION('ref_axis',(1.,-1.06910588403687E-42,1.38777878078144E-14));
#14850=DIRECTION('center_axis',(0.,1.,0.));
#14851=DIRECTION('ref_axis',(0.,0.,1.));
#14852=DIRECTION('center_axis',(0.84916201117318,0.,0.528132444354937));
#14853=DIRECTION('ref_axis',(0.528132444354937,0.,-0.84916201117318));
#14854=DIRECTION('center_axis',(0.,1.,0.));
#14855=DIRECTION('ref_axis',(-0.274625188963804,0.,-0.961551353587834));
#14856=DIRECTION('center_axis',(-0.528132444354927,0.,-0.849162011173186));
#14857=DIRECTION('ref_axis',(-0.849162011173186,0.,0.528132444354927));
#14858=DIRECTION('center_axis',(0.,1.,0.));
#14859=DIRECTION('ref_axis',(0.,0.,1.));
#14860=DIRECTION('center_axis',(0.0822611166554848,-0.0232075739979077,
0.996340562857763));
#14861=DIRECTION('ref_axis',(0.996607302542249,-0.000737174163025255,-0.0823003104108089));
#14862=DIRECTION('center_axis',(-0.996340562857417,-0.0232075739986902,
0.0822611166594516));
#14863=DIRECTION('ref_axis',(0.0823003104147849,-0.000737174163321746,0.99660730254192));
#14864=DIRECTION('center_axis',(-0.224812648466097,0.696171426497067,0.681765808777984));
#14865=DIRECTION('ref_axis',(3.9236749875465E-16,-0.69967611234192,0.714460172310604));
#14866=DIRECTION('center_axis',(-0.839824053586503,0.,-0.542858691574091));
#14867=DIRECTION('ref_axis',(0.542858691574091,2.77555756156287E-14,-0.839824053586503));
#14868=DIRECTION('center_axis',(-0.825680763412087,3.74339213057468E-15,
-0.564137640058907));
#14869=DIRECTION('ref_axis',(0.564137640058907,-1.66533453693773E-14,-0.825680763412087));
#14870=DIRECTION('center_axis',(0.,-1.,0.));
#14871=DIRECTION('ref_axis',(0.,0.,1.));
#14872=DIRECTION('center_axis',(0.,-1.,0.));
#14873=DIRECTION('ref_axis',(0.,0.,-1.));
#14874=DIRECTION('center_axis',(-0.823608768724453,0.,-0.567158351856156));
#14875=DIRECTION('ref_axis',(-0.567158351856156,0.,0.823608768724453));
#14876=DIRECTION('center_axis',(0.313163806483747,0.,-0.949699126201878));
#14877=DIRECTION('ref_axis',(-0.949699126201878,0.,-0.313163806483747));
#14878=DIRECTION('center_axis',(-0.313163806483745,3.07054667648618E-14,
0.949699126201878));
#14879=DIRECTION('ref_axis',(0.949699126201878,1.07892897725893E-28,0.313163806483745));
#14880=DIRECTION('center_axis',(0.,-1.,0.));
#14881=DIRECTION('ref_axis',(0.,0.,-1.));
#14882=DIRECTION('center_axis',(0.,-1.,0.));
#14883=DIRECTION('ref_axis',(0.,0.,-1.));
#14884=DIRECTION('center_axis',(0.,1.,0.));
#14885=DIRECTION('ref_axis',(0.,0.,1.));
#14886=DIRECTION('center_axis',(1.,0.,0.));
#14887=DIRECTION('ref_axis',(0.,0.,-1.));
#14888=DIRECTION('center_axis',(-1.,0.,0.));
#14889=DIRECTION('ref_axis',(0.,0.,1.));
#14890=DIRECTION('center_axis',(1.,0.,0.));
#14891=DIRECTION('ref_axis',(0.,0.,-1.));
#14892=DIRECTION('center_axis',(0.846153846153842,0.,0.532938710021199));
#14893=DIRECTION('ref_axis',(-0.532938710021199,0.,0.846153846153842));
#14894=DIRECTION('center_axis',(0.,1.,0.));
#14895=DIRECTION('ref_axis',(1.,0.,0.));
#14896=DIRECTION('center_axis',(0.313163806483745,6.14109335297236E-14,
-0.949699126201878));
#14897=DIRECTION('ref_axis',(0.949699126201878,3.88578058618798E-14,0.313163806483745));
#14898=DIRECTION('center_axis',(-0.225935650513581,0.692454480471778,0.68517141964735));
#14899=DIRECTION('ref_axis',(2.12986048996937E-14,0.703358708234097,-0.710835091671241));
#14900=DIRECTION('center_axis',(0.72431261840463,0.,0.689471704147334));
#14901=DIRECTION('ref_axis',(-0.689471704147334,-9.99200722162653E-14,0.72431261840463));
#14902=DIRECTION('center_axis',(0.233246104178629,-0.667281700967051,-0.707341067972171));
#14903=DIRECTION('ref_axis',(-1.1771509218523E-15,-0.727404531188479,0.68620889531284));
#14904=DIRECTION('center_axis',(0.,1.,0.));
#14905=DIRECTION('ref_axis',(-0.948898229383528,0.,0.315582240109938));
#14906=DIRECTION('center_axis',(0.819571610992504,0.,0.572976766069229));
#14907=DIRECTION('ref_axis',(-0.572976766069229,0.,0.819571610992504));
#14908=DIRECTION('center_axis',(-0.846153846153842,0.,0.532938710021199));
#14909=DIRECTION('ref_axis',(-0.532938710021199,0.,-0.846153846153842));
#14910=DIRECTION('center_axis',(0.,1.,0.));
#14911=DIRECTION('ref_axis',(0.,0.,1.));
#14912=DIRECTION('center_axis',(0.827607008689209,0.,0.561307971766392));
#14913=DIRECTION('ref_axis',(0.561307971766392,0.,-0.827607008689208));
#14914=DIRECTION('center_axis',(-0.313163806483747,0.,0.949699126201878));
#14915=DIRECTION('ref_axis',(0.949699126201878,0.,0.313163806483747));
#14916=DIRECTION('center_axis',(0.313163806483745,0.,-0.949699126201878));
#14917=DIRECTION('ref_axis',(-0.949699126201878,0.,-0.313163806483745));
#14918=DIRECTION('center_axis',(0.,-1.,0.));
#14919=DIRECTION('ref_axis',(0.,0.,-1.));
#14920=DIRECTION('center_axis',(0.,-1.,0.));
#14921=DIRECTION('ref_axis',(0.210852528929983,0.,0.977517882723294));
#14922=DIRECTION('center_axis',(0.,-1.,0.));
#14923=DIRECTION('ref_axis',(0.,0.,-1.));
#14924=DIRECTION('center_axis',(0.,1.,0.));
#14925=DIRECTION('ref_axis',(0.,0.,1.));
#14926=DIRECTION('center_axis',(-0.313163806483747,0.,0.949699126201878));
#14927=DIRECTION('ref_axis',(0.949699126201878,0.,0.313163806483747));
#14928=DIRECTION('center_axis',(-0.313163806483725,0.,0.949699126201885));
#14929=DIRECTION('ref_axis',(0.949699126201885,0.,0.313163806483725));
#14930=DIRECTION('center_axis',(0.,-1.,0.));
#14931=DIRECTION('ref_axis',(0.,0.,-1.));
#14932=DIRECTION('center_axis',(0.74528868282298,0.,0.666741913528756));
#14933=DIRECTION('ref_axis',(0.666741913528756,0.,-0.74528868282298));
#14934=DIRECTION('center_axis',(0.661925770683741,-7.41191641853799E-15,
0.749569392454585));
#14935=DIRECTION('ref_axis',(-0.749569392454585,-3.03668228410464E-29,0.661925770683741));
#14936=DIRECTION('center_axis',(0.,1.,0.));
#14937=DIRECTION('ref_axis',(0.,0.,1.));
#14938=DIRECTION('center_axis',(-0.749569392454584,-4.86640976974696E-15,
0.661925770683743));
#14939=DIRECTION('ref_axis',(0.661925770683743,3.23979850088036E-29,0.749569392454583));
#14940=DIRECTION('center_axis',(0.707341067972173,0.66728170096705,0.233246104178626));
#14941=DIRECTION('ref_axis',(-0.686208895312839,0.727404531188481,-7.51299950387033E-16));
#14942=DIRECTION('center_axis',(0.,1.,0.));
#14943=DIRECTION('ref_axis',(0.,0.,1.));
#14944=DIRECTION('center_axis',(-0.658838329408371,0.,0.752284557665773));
#14945=DIRECTION('ref_axis',(0.752284557665773,0.,0.658838329408371));
#14946=DIRECTION('center_axis',(-0.949699126201879,0.,-0.313163806483744));
#14947=DIRECTION('ref_axis',(0.221440263540013,-0.707106741740204,-0.671538729686443));
#14948=DIRECTION('center_axis',(0.94969912620188,0.,0.313163806483739));
#14949=DIRECTION('ref_axis',(0.313163806483739,0.,-0.94969912620188));
#14950=DIRECTION('center_axis',(-0.949699126201878,0.,-0.313163806483745));
#14951=DIRECTION('ref_axis',(-0.313163806483745,0.,0.949699126201878));
#14952=DIRECTION('center_axis',(-0.313163806483749,0.,0.949699126201877));
#14953=DIRECTION('ref_axis',(-0.949699126201877,-3.33066907387545E-14,-0.31316380648375));
#14954=DIRECTION('center_axis',(0.,-1.,0.));
#14955=DIRECTION('ref_axis',(2.22044604925031E-14,0.,1.));
#14956=DIRECTION('center_axis',(0.,1.,0.));
#14957=DIRECTION('ref_axis',(1.,0.,0.));
#14958=DIRECTION('center_axis',(-0.676807035378407,-2.98251420004092E-14,
-0.736160469505319));
#14959=DIRECTION('ref_axis',(0.736160469505319,9.88665375602713E-29,-0.676807035378407));
#14960=DIRECTION('center_axis',(0.,1.,0.));
#14961=DIRECTION('ref_axis',(1.,0.,0.));
#14962=DIRECTION('center_axis',(-0.230857726232391,0.675697700970532,0.70009808394392));
#14963=DIRECTION('ref_axis',(-4.57530847286819E-14,0.719534496560286,-0.694456700061088));
#14964=DIRECTION('center_axis',(0.313163806483745,0.,-0.949699126201878));
#14965=DIRECTION('ref_axis',(0.949699126201878,0.,0.313163806483745));
#14966=DIRECTION('center_axis',(-0.532938710021185,0.,-0.846153846153851));
#14967=DIRECTION('ref_axis',(0.846153846153851,0.,-0.532938710021185));
#14968=DIRECTION('center_axis',(0.,0.,1.));
#14969=DIRECTION('ref_axis',(-1.,0.,0.));
#14970=DIRECTION('center_axis',(-3.49148133884313E-15,0.,1.));
#14971=DIRECTION('ref_axis',(1.,0.,3.49148133884313E-15));
#14972=DIRECTION('center_axis',(0.,0.,1.));
#14973=DIRECTION('ref_axis',(1.,0.,0.));
#14974=DIRECTION('center_axis',(0.,1.,0.));
#14975=DIRECTION('ref_axis',(0.,0.,1.));
#14976=DIRECTION('center_axis',(0.,-1.,0.));
#14977=DIRECTION('ref_axis',(2.22044604925031E-14,0.,1.));
#14978=DIRECTION('center_axis',(0.689471704147334,0.,-0.72431261840463));
#14979=DIRECTION('ref_axis',(0.72431261840463,-9.99200722162653E-14,0.689471704147334));
#14980=DIRECTION('center_axis',(0.,1.,0.));
#14981=DIRECTION('ref_axis',(0.,0.,1.));
#14982=DIRECTION('center_axis',(-0.313163806483747,0.,0.949699126201878));
#14983=DIRECTION('ref_axis',(-0.671538702807596,-0.707106770042692,-0.221440254676701));
#14984=DIRECTION('center_axis',(0.,-1.,0.));
#14985=DIRECTION('ref_axis',(0.,0.,-1.));
#14986=DIRECTION('center_axis',(0.,-1.,0.));
#14987=DIRECTION('ref_axis',(0.,0.,-1.));
#14988=DIRECTION('center_axis',(0.,-1.,0.));
#14989=DIRECTION('ref_axis',(0.,0.,-1.));
#14990=DIRECTION('center_axis',(0.313163806483747,0.,-0.949699126201878));
#14991=DIRECTION('ref_axis',(-0.949699126201878,0.,-0.313163806483747));
#14992=DIRECTION('center_axis',(0.313163806483745,0.,-0.949699126201878));
#14993=DIRECTION('ref_axis',(-0.949699126201878,0.,-0.313163806483745));
#14994=DIRECTION('center_axis',(0.,1.,0.));
#14995=DIRECTION('ref_axis',(0.,0.,1.));
#14996=DIRECTION('center_axis',(-0.75228455766577,0.,-0.658838329408374));
#14997=DIRECTION('ref_axis',(-0.658838329408373,0.,0.75228455766577));
#14998=DIRECTION('center_axis',(-0.532938710021199,0.,0.846153846153842));
#14999=DIRECTION('ref_axis',(-0.846153846153842,2.22044604925029E-14,-0.532938710021199));
#15000=DIRECTION('center_axis',(-0.0822611166573683,-0.0232075739980745,
0.996340562857604));
#15001=DIRECTION('ref_axis',(-0.920256040566064,-0.382000889613719,-0.0848772062216844));
#15002=DIRECTION('center_axis',(0.,-1.,0.));
#15003=DIRECTION('ref_axis',(0.,0.,-1.));
#15004=DIRECTION('center_axis',(0.,-1.,0.));
#15005=DIRECTION('ref_axis',(0.,0.,-1.));
#15006=DIRECTION('center_axis',(0.949699126201879,0.,0.313163806483744));
#15007=DIRECTION('ref_axis',(0.313163806483744,0.,-0.949699126201879));
#15008=DIRECTION('center_axis',(0.94969912620188,0.,0.313163806483741));
#15009=DIRECTION('ref_axis',(0.313163806483741,0.,-0.94969912620188));
#15010=DIRECTION('center_axis',(0.,-1.,0.));
#15011=DIRECTION('ref_axis',(0.,0.,-1.));
#15012=DIRECTION('center_axis',(0.666741913528764,1.03429581957828E-14,
-0.745288682822973));
#15013=DIRECTION('ref_axis',(-0.745288682822973,7.03701836569442E-29,-0.666741913528764));
#15014=DIRECTION('center_axis',(-0.700098083943913,-0.675697700970539,-0.230857726232389));
#15015=DIRECTION('ref_axis',(0.694456700061088,-0.719534496560286,-1.51950613122166E-15));
#15016=DIRECTION('center_axis',(-0.788816507333645,0.,-0.614628764180419));
#15017=DIRECTION('ref_axis',(0.614628764180419,0.,-0.788816507333645));
#15018=DIRECTION('center_axis',(-0.313163806483745,4.34602085546888E-15,
0.949699126201878));
#15019=DIRECTION('ref_axis',(-0.949699126201878,-3.01782747192566E-29,-0.313163806483745));
#15020=DIRECTION('center_axis',(0.,1.,0.));
#15021=DIRECTION('ref_axis',(0.,0.,1.));
#15022=DIRECTION('center_axis',(-0.561307971766392,0.,0.827607008689209));
#15023=DIRECTION('ref_axis',(0.827607008689208,0.,0.561307971766392));
#15024=DIRECTION('center_axis',(-0.68176580877798,0.69617142649707,-0.224812648466096));
#15025=DIRECTION('ref_axis',(-0.714460172310607,-0.699676112341916,-6.69170701730011E-16));
#15026=DIRECTION('center_axis',(0.68176580877798,0.69617142649707,0.224812648466096));
#15027=DIRECTION('ref_axis',(-0.714460172310607,0.699676112341916,-6.69170701730011E-16));
#15028=DIRECTION('center_axis',(0.,1.,0.));
#15029=DIRECTION('ref_axis',(0.,0.,1.));
#15030=DIRECTION('center_axis',(-0.564137640058907,-1.99148461346573E-14,
0.825680763412087));
#15031=DIRECTION('ref_axis',(0.825680763412087,-1.41167664996661E-28,0.564137640058907));
#15032=DIRECTION('center_axis',(0.,1.,0.));
#15033=DIRECTION('ref_axis',(1.,0.,0.));
#15034=DIRECTION('center_axis',(-0.736160469505319,-2.04325575765918E-14,
0.676807035378407));
#15035=DIRECTION('ref_axis',(-0.676807035378407,6.6818274548834E-29,-0.736160469505319));
#15036=DIRECTION('center_axis',(0.,1.,0.));
#15037=DIRECTION('ref_axis',(-0.966074959183014,0.,0.258261830783294));
#15038=DIRECTION('center_axis',(-0.949699126201878,0.,-0.313163806483745));
#15039=DIRECTION('ref_axis',(0.313163806483745,0.,-0.949699126201878));
#15040=DIRECTION('center_axis',(0.,-1.,0.));
#15041=DIRECTION('ref_axis',(0.0776244824205716,0.,0.996982667717417));
#15042=DIRECTION('center_axis',(0.,-1.,0.));
#15043=DIRECTION('ref_axis',(0.,0.,-1.));
#15044=DIRECTION('center_axis',(-0.313163806483747,0.,0.949699126201878));
#15045=DIRECTION('ref_axis',(0.949699126201878,0.,0.313163806483747));
#15046=DIRECTION('center_axis',(-0.313163806483745,0.,0.949699126201878));
#15047=DIRECTION('ref_axis',(0.949699126201878,0.,0.313163806483745));
#15048=DIRECTION('center_axis',(0.,-1.,0.));
#15049=DIRECTION('ref_axis',(0.,0.,-1.));
#15050=DIRECTION('center_axis',(-0.708724510210478,-9.83552836689824E-15,
-0.705485342602465));
#15051=DIRECTION('ref_axis',(-0.705485342602465,5.77298571474757E-29,0.708724510210478));
#15052=DIRECTION('center_axis',(0.313163806483747,0.,-0.949699126201878));
#15053=DIRECTION('ref_axis',(0.671538729685915,-0.707106741740759,0.221440263539842));
#15054=DIRECTION('center_axis',(-0.313163806483747,0.,0.949699126201878));
#15055=DIRECTION('ref_axis',(0.949699126201878,0.,0.313163806483747));
#15056=DIRECTION('center_axis',(-0.949699126201878,0.,-0.313163806483745));
#15057=DIRECTION('ref_axis',(0.313163806483745,-3.33066907387545E-14,-0.949699126201878));
#15058=DIRECTION('center_axis',(0.542858691574087,-1.16549000115722E-14,
-0.839824053586506));
#15059=DIRECTION('ref_axis',(0.839824053586506,4.4408920985006E-14,0.542858691574087));
#15060=DIRECTION('center_axis',(-0.542858691574087,-1.16549000115722E-14,
0.839824053586506));
#15061=DIRECTION('ref_axis',(-0.839824053586506,-2.22044604925029E-14,-0.542858691574087));
#15062=DIRECTION('center_axis',(-0.564137640058907,9.65795169688271E-15,
0.825680763412087));
#15063=DIRECTION('ref_axis',(-0.825680763412087,3.33066907387545E-14,-0.564137640058907));
#15064=DIRECTION('center_axis',(0.,-1.,0.));
#15065=DIRECTION('ref_axis',(0.,0.,1.));
#15066=DIRECTION('center_axis',(0.,-1.,0.));
#15067=DIRECTION('ref_axis',(0.,0.,-1.));
#15068=DIRECTION('center_axis',(-0.567158351856161,0.,0.823608768724449));
#15069=DIRECTION('ref_axis',(0.823608768724449,0.,0.567158351856161));
#15070=DIRECTION('center_axis',(-0.949699126201879,0.,-0.313163806483744));
#15071=DIRECTION('ref_axis',(-0.313163806483744,0.,0.949699126201879));
#15072=DIRECTION('center_axis',(0.949699126201878,4.34602085546888E-15,
0.313163806483745));
#15073=DIRECTION('ref_axis',(0.313163806483745,1.5175460366485E-29,-0.949699126201878));
#15074=DIRECTION('center_axis',(0.,-1.,0.));
#15075=DIRECTION('ref_axis',(0.315582053959229,0.,0.948898291293052));
#15076=DIRECTION('center_axis',(0.,-1.,0.));
#15077=DIRECTION('ref_axis',(0.,0.,-1.));
#15078=DIRECTION('center_axis',(0.,-1.,0.));
#15079=DIRECTION('ref_axis',(0.,0.,-1.));
#15080=DIRECTION('center_axis',(-0.949699126201879,0.,-0.313163806483744));
#15081=DIRECTION('ref_axis',(-0.313163806483744,0.,0.949699126201879));
#15082=DIRECTION('center_axis',(-0.949699126201878,0.,-0.313163806483745));
#15083=DIRECTION('ref_axis',(-0.313163806483745,0.,0.949699126201878));
#15084=DIRECTION('center_axis',(0.,-1.,0.));
#15085=DIRECTION('ref_axis',(0.0776244824205756,0.,0.996982667717417));
#15086=DIRECTION('center_axis',(-0.456384763068626,1.59504337716007E-16,
-0.889782528508396));
#15087=DIRECTION('ref_axis',(0.889782528508396,6.01132322447566E-31,-0.456384763068626));
#15088=DIRECTION('center_axis',(0.,1.,0.));
#15089=DIRECTION('ref_axis',(0.,0.,1.));
#15090=DIRECTION('center_axis',(-0.889782528508396,0.,0.456384763068626));
#15091=DIRECTION('ref_axis',(0.456384763068626,0.,0.889782528508396));
#15092=DIRECTION('center_axis',(-0.949699126201879,0.,-0.313163806483744));
#15093=DIRECTION('ref_axis',(0.221440254677041,-0.707106770041599,-0.671538702808635));
#15094=DIRECTION('center_axis',(-0.949699126201879,0.,-0.313163806483743));
#15095=DIRECTION('ref_axis',(0.313163806483743,-3.33066907387549E-14,-0.949699126201879));
#15096=DIRECTION('center_axis',(0.685171419647361,-0.692454480471773,0.225935650513563));
#15097=DIRECTION('ref_axis',(0.710835091671237,0.703358708234102,-1.55285432707423E-15));
#15098=DIRECTION('center_axis',(0.,-1.,0.));
#15099=DIRECTION('ref_axis',(0.,0.,-1.));
#15100=DIRECTION('center_axis',(0.567158351856161,0.,-0.823608768724449));
#15101=DIRECTION('ref_axis',(-0.823608768724449,0.,-0.567158351856161));
#15102=DIRECTION('center_axis',(0.949699126201879,0.,0.313163806483744));
#15103=DIRECTION('ref_axis',(0.313163806483744,0.,-0.949699126201879));
#15104=DIRECTION('center_axis',(-0.949699126201878,4.34602085546888E-15,
-0.313163806483745));
#15105=DIRECTION('ref_axis',(-0.313163806483745,1.5175460366485E-29,0.949699126201878));
#15106=DIRECTION('center_axis',(0.,1.,0.));
#15107=DIRECTION('ref_axis',(0.,0.,1.));
#15108=DIRECTION('center_axis',(0.,0.,-1.));
#15109=DIRECTION('ref_axis',(-1.,0.,0.));
#15110=DIRECTION('center_axis',(0.,0.,1.));
#15111=DIRECTION('ref_axis',(1.,0.,0.));
#15112=DIRECTION('center_axis',(0.,0.,-1.));
#15113=DIRECTION('ref_axis',(-1.,0.,0.));
#15114=DIRECTION('center_axis',(0.532938710021199,0.,-0.846153846153842));
#15115=DIRECTION('ref_axis',(0.846153846153842,0.,0.532938710021199));
#15116=DIRECTION('center_axis',(0.,1.,0.));
#15117=DIRECTION('ref_axis',(1.,0.,0.));
#15118=DIRECTION('center_axis',(-0.949699126201878,6.14109335297236E-14,
-0.313163806483745));
#15119=DIRECTION('ref_axis',(0.313163806483745,6.66133814775086E-14,-0.949699126201878));
#15120=DIRECTION('center_axis',(0.685171419647361,0.692454480471773,0.225935650513563));
#15121=DIRECTION('ref_axis',(0.71083509167124,-0.703358708234099,-2.35087979245205E-14));
#15122=DIRECTION('center_axis',(0.,1.,0.));
#15123=DIRECTION('ref_axis',(1.,0.,0.));
#15124=DIRECTION('center_axis',(0.57297676606922,0.,-0.81957161099251));
#15125=DIRECTION('ref_axis',(0.81957161099251,0.,0.57297676606922));
#15126=DIRECTION('center_axis',(0.,-1.,0.));
#15127=DIRECTION('ref_axis',(0.,0.,1.));
#15128=DIRECTION('center_axis',(0.,-1.,0.));
#15129=DIRECTION('ref_axis',(0.,0.,-1.));
#15130=DIRECTION('center_axis',(-0.949699126201879,0.,-0.313163806483742));
#15131=DIRECTION('ref_axis',(-0.313163806483742,0.,0.949699126201879));
#15132=DIRECTION('center_axis',(0.313163806483747,0.,-0.949699126201878));
#15133=DIRECTION('ref_axis',(-0.949699126201878,0.,-0.313163806483747));
#15134=DIRECTION('center_axis',(-0.313163806483745,3.29493073867411E-15,
0.949699126201878));
#15135=DIRECTION('ref_axis',(0.949699126201878,-5.77669955272155E-30,0.313163806483745));
#15136=DIRECTION('center_axis',(0.,1.,0.));
#15137=DIRECTION('ref_axis',(0.,0.,1.));
#15138=DIRECTION('center_axis',(0.,-1.,0.));
#15139=DIRECTION('ref_axis',(0.,0.,1.));
#15140=DIRECTION('center_axis',(0.,1.,0.));
#15141=DIRECTION('ref_axis',(1.,0.,0.));
#15142=DIRECTION('center_axis',(0.949699126201878,6.14109335297236E-14,
0.313163806483745));
#15143=DIRECTION('ref_axis',(-0.313163806483745,9.43689570931373E-14,0.949699126201878));
#15144=DIRECTION('center_axis',(0.,1.,0.));
#15145=DIRECTION('ref_axis',(1.,0.,0.));
#15146=DIRECTION('center_axis',(-0.57297676606922,0.,0.81957161099251));
#15147=DIRECTION('ref_axis',(-0.81957161099251,0.,-0.57297676606922));
#15148=DIRECTION('center_axis',(0.532938710021199,0.,0.846153846153842));
#15149=DIRECTION('ref_axis',(-0.846153846153842,0.,0.532938710021199));
#15150=DIRECTION('center_axis',(0.,1.,0.));
#15151=DIRECTION('ref_axis',(0.,0.,1.));
#15152=DIRECTION('center_axis',(0.561307971766392,0.,-0.827607008689209));
#15153=DIRECTION('ref_axis',(-0.827607008689208,0.,-0.561307971766392));
#15154=DIRECTION('center_axis',(0.949699126201879,0.,0.313163806483744));
#15155=DIRECTION('ref_axis',(0.313163806483744,0.,-0.949699126201879));
#15156=DIRECTION('center_axis',(-0.949699126201878,0.,-0.313163806483745));
#15157=DIRECTION('ref_axis',(-0.313163806483745,0.,0.949699126201878));
#15158=DIRECTION('center_axis',(0.,-1.,0.));
#15159=DIRECTION('ref_axis',(0.,0.,-1.));
#15160=DIRECTION('center_axis',(0.,-1.,0.));
#15161=DIRECTION('ref_axis',(0.,0.,-1.));
#15162=DIRECTION('center_axis',(0.,-1.,0.));
#15163=DIRECTION('ref_axis',(0.,0.,-1.));
#15164=DIRECTION('center_axis',(-0.949699126201879,0.,-0.313163806483744));
#15165=DIRECTION('ref_axis',(-0.313163806483744,0.,0.949699126201879));
#15166=DIRECTION('center_axis',(0.,-1.,0.));
#15167=DIRECTION('ref_axis',(0.,0.,-1.));
#15168=DIRECTION('center_axis',(-0.889782528508396,0.,0.456384763068626));
#15169=DIRECTION('ref_axis',(0.456384763068626,0.,0.889782528508396));
#15170=DIRECTION('center_axis',(0.,-1.,0.));
#15171=DIRECTION('ref_axis',(0.,0.,-1.));
#15172=DIRECTION('center_axis',(0.,-1.,0.));
#15173=DIRECTION('ref_axis',(0.,0.,-1.));
#15174=DIRECTION('center_axis',(-0.949699126201879,0.,-0.313163806483744));
#15175=DIRECTION('ref_axis',(-0.313163806483744,0.,0.949699126201879));
#15176=DIRECTION('center_axis',(0.949699126201878,0.,0.313163806483745));
#15177=DIRECTION('ref_axis',(0.313163806483745,0.,-0.949699126201878));
#15178=DIRECTION('center_axis',(0.,-1.,0.));
#15179=DIRECTION('ref_axis',(0.,0.,-1.));
#15180=DIRECTION('center_axis',(0.,1.,0.));
#15181=DIRECTION('ref_axis',(0.,0.,1.));
#15182=DIRECTION('center_axis',(0.661925770683734,-1.7968282226759E-15,
0.749569392454591));
#15183=DIRECTION('ref_axis',(0.749569392454591,-9.3759599088471E-30,-0.661925770683734));
#15184=DIRECTION('center_axis',(0.233246104178643,0.667281700967055,-0.707341067972163));
#15185=DIRECTION('ref_axis',(1.28973797951009E-15,0.727404531188473,0.686208895312847));
#15186=DIRECTION('center_axis',(0.,1.,0.));
#15187=DIRECTION('ref_axis',(0.,0.,1.));
#15188=DIRECTION('center_axis',(0.75228455766577,0.,0.658838329408374));
#15189=DIRECTION('ref_axis',(0.658838329408373,0.,-0.75228455766577));
#15190=DIRECTION('center_axis',(-0.313163806483754,0.,0.949699126201876));
#15191=DIRECTION('ref_axis',(-0.671538729686488,-0.707106741740154,-0.221440263540036));
#15192=DIRECTION('center_axis',(0.313163806483747,0.,-0.949699126201878));
#15193=DIRECTION('ref_axis',(-0.949699126201878,0.,-0.313163806483747));
#15194=DIRECTION('center_axis',(-0.313163806483745,-8.69204171093777E-15,
0.949699126201878));
#15195=DIRECTION('ref_axis',(0.949699126201878,-6.03565494385133E-29,0.313163806483745));
#15196=DIRECTION('center_axis',(0.949699126201878,0.,0.313163806483745));
#15197=DIRECTION('ref_axis',(-0.313163806483745,-3.33066907387545E-14,0.949699126201878));
#15198=DIRECTION('center_axis',(0.705485342602465,9.83552836689824E-15,
-0.708724510210478));
#15199=DIRECTION('ref_axis',(0.708724510210478,5.71963539909091E-29,0.705485342602465));
#15200=DIRECTION('center_axis',(0.,-1.,0.));
#15201=DIRECTION('ref_axis',(0.,0.,-1.));
#15202=DIRECTION('center_axis',(0.,-1.,0.));
#15203=DIRECTION('ref_axis',(-2.22044604925031E-14,0.,1.));
#15204=DIRECTION('center_axis',(-0.724312618404621,0.,-0.689471704147344));
#15205=DIRECTION('ref_axis',(0.689471704147344,-5.55111512312576E-15,-0.724312618404621));
#15206=DIRECTION('center_axis',(0.,1.,0.));
#15207=DIRECTION('ref_axis',(0.,0.,1.));
#15208=DIRECTION('center_axis',(0.889782528508396,0.,-0.456384763068626));
#15209=DIRECTION('ref_axis',(-0.456384763068626,0.,-0.889782528508396));
#15210=DIRECTION('center_axis',(0.949699126201879,0.,0.313163806483744));
#15211=DIRECTION('ref_axis',(-0.221440254676618,-0.707106770042951,0.671538702807351));
#15212=DIRECTION('center_axis',(0.949699126201878,0.,0.313163806483745));
#15213=DIRECTION('ref_axis',(0.313163806483745,0.,-0.949699126201878));
#15214=DIRECTION('center_axis',(0.,-1.,0.));
#15215=DIRECTION('ref_axis',(0.,0.,-1.));
#15216=DIRECTION('center_axis',(0.614628764180404,0.,-0.788816507333657));
#15217=DIRECTION('ref_axis',(-0.788816507333657,0.,-0.614628764180404));
#15218=DIRECTION('center_axis',(-0.949699126201879,0.,-0.313163806483744));
#15219=DIRECTION('ref_axis',(-0.313163806483744,0.,0.949699126201879));
#15220=DIRECTION('center_axis',(-0.949699126201879,0.,-0.313163806483743));
#15221=DIRECTION('ref_axis',(0.313163806483743,0.,-0.949699126201879));
#15222=DIRECTION('center_axis',(0.,-1.,0.));
#15223=DIRECTION('ref_axis',(0.297486285481071,0.,0.954726091583693));
#15224=DIRECTION('center_axis',(0.,-1.,0.));
#15225=DIRECTION('ref_axis',(0.,0.,-1.));
#15226=DIRECTION('center_axis',(0.313163806483754,0.,-0.949699126201876));
#15227=DIRECTION('ref_axis',(-0.949699126201876,0.,-0.313163806483754));
#15228=DIRECTION('center_axis',(0.313163806483745,0.,-0.949699126201878));
#15229=DIRECTION('ref_axis',(-0.949699126201878,0.,-0.313163806483745));
#15230=DIRECTION('center_axis',(0.,-1.,0.));
#15231=DIRECTION('ref_axis',(0.,0.,-1.));
#15232=DIRECTION('center_axis',(-0.745288682822956,1.03429581957826E-14,
-0.666741913528783));
#15233=DIRECTION('ref_axis',(-0.666741913528783,1.71777308129412E-29,0.745288682822956));
#15234=DIRECTION('center_axis',(-0.230857726232396,-0.675697700970517,0.700098083943933));
#15235=DIRECTION('ref_axis',(-1.21960194499758E-15,-0.719534496560307,-0.694456700061066));
#15236=DIRECTION('center_axis',(0.,1.,0.));
#15237=DIRECTION('ref_axis',(0.,0.,1.));
#15238=DIRECTION('center_axis',(0.,-1.,0.));
#15239=DIRECTION('ref_axis',(-5.55111512312578E-15,0.,1.));
#15240=DIRECTION('center_axis',(0.614628764180404,0.,-0.788816507333657));
#15241=DIRECTION('ref_axis',(0.788816507333657,0.,0.614628764180404));
#15242=DIRECTION('center_axis',(0.,1.,0.));
#15243=DIRECTION('ref_axis',(1.,0.,0.));
#15244=DIRECTION('center_axis',(0.676807035378399,-2.98251420004093E-14,
0.736160469505326));
#15245=DIRECTION('ref_axis',(-0.736160469505326,-4.54993050005069E-29,0.676807035378399));
#15246=DIRECTION('center_axis',(0.,1.,0.));
#15247=DIRECTION('ref_axis',(1.,0.,0.));
#15248=DIRECTION('center_axis',(-0.313163806483749,0.,0.949699126201877));
#15249=DIRECTION('ref_axis',(-0.949699126201877,0.,-0.31316380648375));
#15250=DIRECTION('center_axis',(0.,-1.,0.));
#15251=DIRECTION('ref_axis',(0.,0.,-1.));
#15252=DIRECTION('center_axis',(0.,-1.,0.));
#15253=DIRECTION('ref_axis',(0.,0.,-1.));
#15254=DIRECTION('center_axis',(0.949699126201879,0.,0.313163806483744));
#15255=DIRECTION('ref_axis',(0.313163806483744,0.,-0.949699126201879));
#15256=DIRECTION('center_axis',(0.949699126201877,0.,0.313163806483749));
#15257=DIRECTION('ref_axis',(0.313163806483749,0.,-0.949699126201877));
#15258=DIRECTION('center_axis',(0.,-1.,0.));
#15259=DIRECTION('ref_axis',(0.,0.,-1.));
#15260=DIRECTION('center_axis',(0.705485342602465,-9.83552836689824E-15,
-0.708724510210478));
#15261=DIRECTION('ref_axis',(-0.708724510210478,5.71963539909091E-29,-0.705485342602465));
#15262=DIRECTION('center_axis',(0.,-1.,0.));
#15263=DIRECTION('ref_axis',(0.,0.,-1.));
#15264=DIRECTION('center_axis',(0.,-1.,0.));
#15265=DIRECTION('ref_axis',(0.,0.,-1.));
#15266=DIRECTION('center_axis',(0.,1.,0.));
#15267=DIRECTION('ref_axis',(0.,0.,1.));
#15268=DIRECTION('center_axis',(0.949699126201879,0.,0.313163806483744));
#15269=DIRECTION('ref_axis',(0.313163806483744,0.,-0.949699126201879));
#15270=DIRECTION('center_axis',(0.949699126201878,0.,0.313163806483745));
#15271=DIRECTION('ref_axis',(0.313163806483745,0.,-0.949699126201878));
#15272=DIRECTION('center_axis',(-0.949699126201878,0.,-0.313163806483745));
#15273=DIRECTION('ref_axis',(-0.313163806483745,0.,0.949699126201878));
#15274=DIRECTION('center_axis',(0.,-1.,0.));
#15275=DIRECTION('ref_axis',(0.,0.,-1.));
#15276=DIRECTION('center_axis',(-0.313163806483754,0.,0.949699126201876));
#15277=DIRECTION('ref_axis',(0.949699126201876,0.,0.313163806483754));
#15278=DIRECTION('center_axis',(-0.313163806483758,0.,0.949699126201874));
#15279=DIRECTION('ref_axis',(0.949699126201874,0.,0.313163806483758));
#15280=DIRECTION('center_axis',(0.,-1.,0.));
#15281=DIRECTION('ref_axis',(0.,0.,-1.));
#15282=DIRECTION('center_axis',(-0.889782528508396,0.,0.456384763068626));
#15283=DIRECTION('ref_axis',(-0.456384763068626,0.,-0.889782528508396));
#15284=DIRECTION('center_axis',(0.,1.,0.));
#15285=DIRECTION('ref_axis',(1.,0.,0.));
#15286=DIRECTION('center_axis',(-0.700098083943913,0.675697700970539,-0.230857726232389));
#15287=DIRECTION('ref_axis',(0.69445670006108,0.719534496560294,4.50025703477272E-14));
#15288=DIRECTION('center_axis',(0.666741913528764,-1.03429581957828E-14,
-0.745288682822973));
#15289=DIRECTION('ref_axis',(0.745288682822973,5.55111512312587E-15,0.666741913528764));
#15290=DIRECTION('center_axis',(0.,-1.,0.));
#15291=DIRECTION('ref_axis',(0.,0.,-1.));
#15292=DIRECTION('center_axis',(0.689471704147334,0.,-0.72431261840463));
#15293=DIRECTION('ref_axis',(-0.72431261840463,0.,-0.689471704147334));
#15294=DIRECTION('center_axis',(-0.949699126201879,0.,-0.313163806483744));
#15295=DIRECTION('ref_axis',(-0.313163806483744,0.,0.949699126201879));
#15296=DIRECTION('center_axis',(-0.94969912620188,0.,-0.313163806483741));
#15297=DIRECTION('ref_axis',(-0.313163806483741,0.,0.94969912620188));
#15298=DIRECTION('center_axis',(0.,-1.,0.));
#15299=DIRECTION('ref_axis',(0.,0.,-1.));
#15300=DIRECTION('center_axis',(-0.736160469505319,2.04325575765918E-14,
0.676807035378407));
#15301=DIRECTION('ref_axis',(0.676807035378407,6.6818274548834E-29,0.736160469505319));
#15302=DIRECTION('center_axis',(0.,-1.,0.));
#15303=DIRECTION('ref_axis',(0.,0.,1.));
#15304=DIRECTION('center_axis',(0.,-1.,0.));
#15305=DIRECTION('ref_axis',(0.,0.,-1.));
#15306=DIRECTION('center_axis',(-0.313163806483752,0.,0.949699126201876));
#15307=DIRECTION('ref_axis',(0.949699126201876,0.,0.313163806483752));
#15308=DIRECTION('center_axis',(0.949699126201879,0.,0.313163806483744));
#15309=DIRECTION('ref_axis',(0.313163806483744,0.,-0.949699126201879));
#15310=DIRECTION('center_axis',(-0.949699126201879,0.,-0.313163806483742));
#15311=DIRECTION('ref_axis',(-0.313163806483742,0.,0.949699126201879));
#15312=DIRECTION('center_axis',(0.707341067972173,-0.66728170096705,0.233246104178626));
#15313=DIRECTION('ref_axis',(-0.686208895312839,-0.727404531188481,-7.51299950387033E-16));
#15314=DIRECTION('center_axis',(0.,1.,0.));
#15315=DIRECTION('ref_axis',(-0.977517882722095,0.,0.210852528935538));
#15316=DIRECTION('center_axis',(0.,1.,0.));
#15317=DIRECTION('ref_axis',(0.,0.,-1.));
#15318=DIRECTION('center_axis',(0.,-1.,0.));
#15319=DIRECTION('ref_axis',(0.225340727186267,0.,0.974280019640742));
#15320=DIRECTION('center_axis',(0.,-1.,0.));
#15321=DIRECTION('ref_axis',(0.,0.,-1.));
#15322=DIRECTION('center_axis',(-0.313163806483754,0.,0.949699126201876));
#15323=DIRECTION('ref_axis',(0.949699126201876,0.,0.313163806483754));
#15324=DIRECTION('center_axis',(0.,-1.,0.));
#15325=DIRECTION('ref_axis',(0.,0.,-1.));
#15326=DIRECTION('center_axis',(-0.949699126201878,4.34602085546888E-15,
-0.313163806483745));
#15327=DIRECTION('ref_axis',(0.313163806483745,-3.02285113016155E-29,-0.949699126201878));
#15328=DIRECTION('center_axis',(-0.658838329408371,0.,0.752284557665773));
#15329=DIRECTION('ref_axis',(-0.752284557665773,-2.77555756156289E-14,-0.658838329408371));
#15330=DIRECTION('center_axis',(0.,1.,0.));
#15331=DIRECTION('ref_axis',(0.,0.,1.));
#15332=DIRECTION('center_axis',(-0.846153846153842,0.,0.532938710021199));
#15333=DIRECTION('ref_axis',(0.532938710021199,0.,0.846153846153842));
#15334=DIRECTION('center_axis',(0.,-1.,0.));
#15335=DIRECTION('ref_axis',(0.,0.,-1.));
#15336=DIRECTION('center_axis',(0.,1.,0.));
#15337=DIRECTION('ref_axis',(0.,0.,1.));
#15338=DIRECTION('center_axis',(-0.708724510210478,-9.83552836689824E-15,
-0.705485342602465));
#15339=DIRECTION('ref_axis',(0.705485342602465,-5.77298571474757E-29,-0.708724510210478));
#15340=DIRECTION('center_axis',(0.949699126201879,0.,0.313163806483744));
#15341=DIRECTION('ref_axis',(-0.221440263539776,-0.707106741740963,0.671538729685723));
#15342=DIRECTION('center_axis',(-0.949699126201879,0.,-0.313163806483744));
#15343=DIRECTION('ref_axis',(-0.313163806483744,0.,0.949699126201879));
#15344=DIRECTION('center_axis',(-1.,0.,0.));
#15345=DIRECTION('ref_axis',(0.,0.,-1.));
#15346=DIRECTION('center_axis',(-0.749569392454584,4.86640976974694E-15,
0.661925770683743));
#15347=DIRECTION('ref_axis',(-0.661925770683743,3.17031459090513E-29,-0.749569392454584));
#15348=DIRECTION('center_axis',(0.,-1.,0.));
#15349=DIRECTION('ref_axis',(0.,0.,-1.));
#15350=DIRECTION('center_axis',(-0.788816507333645,0.,-0.614628764180419));
#15351=DIRECTION('ref_axis',(-0.614628764180419,0.,0.788816507333645));
#15352=DIRECTION('center_axis',(0.313163806483754,0.,-0.949699126201876));
#15353=DIRECTION('ref_axis',(-0.949699126201876,0.,-0.313163806483754));
#15354=DIRECTION('center_axis',(0.,1.,0.));
#15355=DIRECTION('ref_axis',(0.,0.,1.));
#15356=DIRECTION('center_axis',(-0.456384763068618,0.,-0.8897825285084));
#15357=DIRECTION('ref_axis',(-0.8897825285084,0.,0.456384763068618));
#15358=DIRECTION('center_axis',(-1.,0.,0.));
#15359=DIRECTION('ref_axis',(0.,0.,1.));
#15360=DIRECTION('center_axis',(-1.,0.,0.));
#15361=DIRECTION('ref_axis',(0.,0.,1.));
#15362=DIRECTION('center_axis',(0.,1.,0.));
#15363=DIRECTION('ref_axis',(0.,0.,1.));
#15364=DIRECTION('center_axis',(0.,1.,0.));
#15365=DIRECTION('ref_axis',(-1.11022302462516E-14,0.,-1.));
#15366=DIRECTION('center_axis',(0.,1.,0.));
#15367=DIRECTION('ref_axis',(-0.0776244824205643,0.,-0.996982667717418));
#15368=DIRECTION('center_axis',(-0.313163806483752,0.,0.949699126201876));
#15369=DIRECTION('ref_axis',(-0.949699126201876,0.,-0.313163806483752));
#15370=DIRECTION('center_axis',(-0.846153846153842,0.,-0.532938710021199));
#15371=DIRECTION('ref_axis',(0.532938710021199,0.,-0.846153846153842));
#15372=DIRECTION('center_axis',(-0.996340562857841,-0.0232075739972549,
-0.0822611166547301));
#15373=DIRECTION('ref_axis',(0.0848772062189317,-0.382000889613913,-0.920256040566237));
#15374=DIRECTION('center_axis',(0.,-1.,0.));
#15375=DIRECTION('ref_axis',(0.,0.,-1.));
#15376=DIRECTION('center_axis',(0.,1.,0.));
#15377=DIRECTION('ref_axis',(0.,0.,1.));
#15378=DIRECTION('center_axis',(0.313163806483754,0.,-0.949699126201876));
#15379=DIRECTION('ref_axis',(0.671538702806552,-0.70710677004379,0.221440254676362));
#15380=DIRECTION('center_axis',(-0.313163806483745,0.,0.949699126201878));
#15381=DIRECTION('ref_axis',(0.949699126201878,0.,0.313163806483745));
#15382=DIRECTION('center_axis',(0.,1.,0.));
#15383=DIRECTION('ref_axis',(0.,0.,1.));
#15384=DIRECTION('center_axis',(-0.827607008689209,0.,-0.561307971766392));
#15385=DIRECTION('ref_axis',(-0.561307971766392,0.,0.827607008689208));
#15386=DIRECTION('center_axis',(0.,1.,0.));
#15387=DIRECTION('ref_axis',(0.,0.,1.));
#15388=DIRECTION('center_axis',(-0.825680763412081,7.71138778898377E-15,
-0.564137640058916));
#15389=DIRECTION('ref_axis',(-0.564137640058916,-2.44199728449863E-29,0.825680763412081));
#15390=DIRECTION('center_axis',(0.,-1.,0.));
#15391=DIRECTION('ref_axis',(0.,0.,-1.));
#15392=DIRECTION('center_axis',(0.,-1.,0.));
#15393=DIRECTION('ref_axis',(0.,0.,-1.));
#15394=DIRECTION('center_axis',(0.,1.,0.));
#15395=DIRECTION('ref_axis',(0.,0.,1.));
#15396=DIRECTION('center_axis',(0.,-1.,0.));
#15397=DIRECTION('ref_axis',(0.,0.,-1.));
#15398=DIRECTION('center_axis',(0.819571610992504,0.,0.572976766069229));
#15399=DIRECTION('ref_axis',(0.572976766069229,0.,-0.819571610992504));
#15400=DIRECTION('center_axis',(0.313163806483758,0.,-0.949699126201874));
#15401=DIRECTION('ref_axis',(0.949699126201874,5.55111512312577E-15,0.313163806483758));
#15402=DIRECTION('center_axis',(0.,1.,0.));
#15403=DIRECTION('ref_axis',(1.,0.,0.));
#15404=DIRECTION('center_axis',(-0.313163806483745,-4.34602085546888E-15,
0.949699126201878));
#15405=DIRECTION('ref_axis',(-0.949699126201878,1.50881680010028E-29,-0.313163806483745));
#15406=DIRECTION('center_axis',(0.313163806483754,0.,-0.949699126201876));
#15407=DIRECTION('ref_axis',(-0.949699126201876,0.,-0.313163806483754));
#15408=DIRECTION('center_axis',(0.313163806483745,-5.70649126742547E-14,
-0.949699126201878));
#15409=DIRECTION('ref_axis',(-0.949699126201878,-3.98789244989641E-28,-0.313163806483745));
#15410=DIRECTION('center_axis',(-0.225935650513579,-0.692454480471764,0.685171419647365));
#15411=DIRECTION('ref_axis',(5.0708331257006E-16,-0.70335870823411,-0.710835091671229));
#15412=DIRECTION('center_axis',(0.224812648466099,0.69617142649706,-0.68176580877799));
#15413=DIRECTION('ref_axis',(1.59296345262975E-15,0.699676112341926,0.714460172310597));
#15414=DIRECTION('center_axis',(-0.313163806483753,0.,0.949699126201876));
#15415=DIRECTION('ref_axis',(0.949699126201876,0.,0.313163806483754));
#15416=DIRECTION('center_axis',(0.,1.,0.));
#15417=DIRECTION('ref_axis',(-0.947774827752477,0.,0.318940238726257));
#15418=DIRECTION('center_axis',(-0.823608768724459,0.,-0.567158351856147));
#15419=DIRECTION('ref_axis',(0.567158351856147,4.44089209850067E-14,-0.823608768724459));
#15420=DIRECTION('center_axis',(0.839824053586503,0.,0.542858691574091));
#15421=DIRECTION('ref_axis',(-0.542858691574091,6.66133814775089E-14,0.839824053586503));
#15422=DIRECTION('center_axis',(0.,-1.,0.));
#15423=DIRECTION('ref_axis',(0.,0.,-1.));
#15424=DIRECTION('center_axis',(0.500078040677557,0.706998150315573,-0.500075562972692));
#15425=DIRECTION('ref_axis',(-0.487455410628725,0.707106781187,0.512237467048381));
#15426=DIRECTION('center_axis',(0.500078143315287,0.706996252576076,-0.500078143315344));
#15427=DIRECTION('ref_axis',(2.88606387015194E-15,0.57747058809669,0.816411489313608));
#15428=DIRECTION('center_axis',(-0.500075464669955,-0.707000041916729,0.500075464669955));
#15429=DIRECTION('ref_axis',(2.20421081150854E-15,-0.577466463418735,-0.816414406797589));
#15430=DIRECTION('center_axis',(0.,1.,0.));
#15431=DIRECTION('ref_axis',(1.,0.,0.));
#15432=DIRECTION('center_axis',(0.724563445309596,1.40751544109608E-14,
0.689208106250273));
#15433=DIRECTION('ref_axis',(-0.689208106250273,5.95362936016406E-29,0.724563445309596));
#15434=DIRECTION('center_axis',(0.,1.,0.));
#15435=DIRECTION('ref_axis',(1.,0.,0.));
#15436=DIRECTION('center_axis',(-0.707106781186534,0.,0.707106781186561));
#15437=DIRECTION('ref_axis',(-0.707106781186561,0.,-0.707106781186534));
#15438=DIRECTION('center_axis',(0.724265465251865,-1.96202318550286E-14,
0.68952123668782));
#15439=DIRECTION('ref_axis',(-0.68952123668782,-2.7755575615629E-14,0.724265465251865));
#15440=DIRECTION('center_axis',(0.,1.,0.));
#15441=DIRECTION('ref_axis',(-7.65709097232158E-16,0.,-1.));
#15442=DIRECTION('center_axis',(0.724563445309603,-9.43334816904809E-15,
-0.689208106250266));
#15443=DIRECTION('ref_axis',(-0.689208106250266,2.1657800856212E-29,-0.724563445309603));
#15444=DIRECTION('center_axis',(0.,1.,0.));
#15445=DIRECTION('ref_axis',(0.,0.,1.));
#15446=DIRECTION('center_axis',(0.707106781186551,0.,-0.707106781186544));
#15447=DIRECTION('ref_axis',(-0.707106781186544,0.,-0.707106781186551));
#15448=DIRECTION('center_axis',(-0.707106781186548,0.,0.707106781186548));
#15449=DIRECTION('ref_axis',(0.707106781186548,0.,0.707106781186548));
#15450=DIRECTION('center_axis',(0.,1.,0.));
#15451=DIRECTION('ref_axis',(1.,0.,0.));
#15452=DIRECTION('center_axis',(0.724563445309596,1.49735685222987E-16,
0.689208106250273));
#15453=DIRECTION('ref_axis',(-0.689208106250273,-1.38777878078143E-15,0.724563445309596));
#15454=DIRECTION('center_axis',(-0.500078143315301,0.706996252576096,0.500078143315301));
#15455=DIRECTION('ref_axis',(-6.82379179808067E-16,0.577470588096647,-0.816411489313638));
#15456=DIRECTION('center_axis',(0.,1.,0.));
#15457=DIRECTION('ref_axis',(1.,0.,0.));
#15458=DIRECTION('center_axis',(0.500078143315295,-0.706996252576104,0.500078143315295));
#15459=DIRECTION('ref_axis',(-2.4326062740384E-14,0.577470588096627,0.816411489313652));
#15460=DIRECTION('center_axis',(1.,0.,0.));
#15461=DIRECTION('ref_axis',(0.,0.,1.));
#15462=DIRECTION('center_axis',(-0.985559589508073,-0.169328956556991,-1.055202794374E-16));
#15463=DIRECTION('ref_axis',(-0.169328956556991,0.985559589508073,-2.75791750167464E-32));
#15464=DIRECTION('center_axis',(0.,1.,0.));
#15465=DIRECTION('ref_axis',(0.707106781186548,0.,-0.707106781186548));
#15466=DIRECTION('center_axis',(0.707106781186548,9.81307786677359E-15,
-0.707106781186548));
#15467=DIRECTION('ref_axis',(-0.707106781186548,-3.73353565333889E-32,-0.707106781186548));
#15468=DIRECTION('center_axis',(-0.500065457858295,0.707014197674946,0.500065457858294));
#15469=DIRECTION('ref_axis',(-0.816425305441283,-0.577451054752788,2.42893944196122E-17));
#15470=DIRECTION('center_axis',(0.,1.,0.));
#15471=DIRECTION('ref_axis',(1.89882616186822E-15,0.,-1.));
#15472=DIRECTION('center_axis',(0.724563445309596,1.34013438274573E-14,
-0.689208106250273));
#15473=DIRECTION('ref_axis',(-0.689208106250273,5.6910531650358E-29,-0.724563445309596));
#15474=DIRECTION('center_axis',(-0.500076315109388,0.706998838848565,-0.500076315109401));
#15475=DIRECTION('ref_axis',(-0.707106781188416,-2.6290097559751E-12,0.707106781184679));
#15476=DIRECTION('center_axis',(0.50007546466997,-0.707000041916716,0.50007546466996));
#15477=DIRECTION('ref_axis',(0.816414406797577,0.577466463418752,-1.98804944403104E-15));
#15478=DIRECTION('center_axis',(0.,1.,0.));
#15479=DIRECTION('ref_axis',(0.,0.,1.));
#15480=DIRECTION('center_axis',(0.724265465251897,0.,-0.689521236687785));
#15481=DIRECTION('ref_axis',(-0.689521236687785,0.,-0.724265465251897));
#15482=DIRECTION('center_axis',(-0.985559589508072,0.169328956556993,0.));
#15483=DIRECTION('ref_axis',(-0.169328956556993,-0.985559589508072,0.));
#15484=DIRECTION('center_axis',(-1.,0.,1.95461800110063E-16));
#15485=DIRECTION('ref_axis',(1.95461800110063E-16,0.,1.));
#15486=DIRECTION('center_axis',(1.,0.,0.));
#15487=DIRECTION('ref_axis',(0.,0.,-1.));
#15488=DIRECTION('center_axis',(-0.707106781186549,0.,0.707106781186546));
#15489=DIRECTION('ref_axis',(0.707106781186546,0.,0.707106781186549));
#15490=DIRECTION('center_axis',(0.707106781186548,-9.81307786677359E-15,
-0.707106781186548));
#15491=DIRECTION('ref_axis',(-0.707106781186548,3.73353565333889E-32,-0.707106781186548));
#15492=DIRECTION('center_axis',(0.,1.,0.));
#15493=DIRECTION('ref_axis',(1.,0.,0.));
#15494=DIRECTION('center_axis',(0.723101268110532,0.,0.690742032930486));
#15495=DIRECTION('ref_axis',(-0.690742032930486,-5.55111512312578E-15,0.723101268110532));
#15496=DIRECTION('center_axis',(-0.707106781186548,1.96261557335472E-14,
0.707106781186548));
#15497=DIRECTION('ref_axis',(-0.707106781186548,7.46707130667779E-32,-0.707106781186548));
#15498=DIRECTION('center_axis',(0.,1.,0.));
#15499=DIRECTION('ref_axis',(1.,0.,0.));
#15500=DIRECTION('center_axis',(0.50007814331529,0.706996252576075,0.500078143315342));
#15501=DIRECTION('ref_axis',(2.42101966234701E-15,0.577470588096689,-0.816411489313609));
#15502=DIRECTION('center_axis',(0.,1.,0.));
#15503=DIRECTION('ref_axis',(1.,0.,0.));
#15504=DIRECTION('center_axis',(0.707106781186548,0.,0.707106781186548));
#15505=DIRECTION('ref_axis',(-0.707106781186548,-4.99600361081318E-14,0.707106781186548));
#15506=DIRECTION('center_axis',(-1.,0.,0.));
#15507=DIRECTION('ref_axis',(0.,0.,-1.));
#15508=DIRECTION('center_axis',(0.,1.,0.));
#15509=DIRECTION('ref_axis',(0.,0.,1.));
#15510=DIRECTION('center_axis',(0.,0.,1.));
#15511=DIRECTION('ref_axis',(1.,0.,0.));
#15512=DIRECTION('center_axis',(0.,1.,0.));
#15513=DIRECTION('ref_axis',(-0.999924538176052,0.,-0.0122848668453797));
#15514=DIRECTION('center_axis',(0.50007546466995,0.707000041916716,-0.50007546466998));
#15515=DIRECTION('ref_axis',(1.4509032190736E-15,-0.577466463418761,-0.81641440679757));
#15516=DIRECTION('center_axis',(-0.689521236687775,0.,-0.724265465251907));
#15517=DIRECTION('ref_axis',(0.724265465251907,-6.66133814775095E-14,-0.689521236687775));
#15518=DIRECTION('center_axis',(0.707106781186551,0.,-0.707106781186544));
#15519=DIRECTION('ref_axis',(-0.707106781186544,0.,-0.707106781186551));
#15520=DIRECTION('center_axis',(0.,-1.,0.));
#15521=DIRECTION('ref_axis',(0.,0.,-1.));
#15522=DIRECTION('center_axis',(0.50006545785829,0.707014197674953,0.50006545785829));
#15523=DIRECTION('ref_axis',(1.98508446711413E-15,-0.577451054752781,0.816425305441288));
#15524=DIRECTION('center_axis',(0.707106781186548,0.,0.707106781186547));
#15525=DIRECTION('ref_axis',(0.707106781186547,0.,-0.707106781186548));
#15526=DIRECTION('center_axis',(0.707106781186548,0.,0.707106781186548));
#15527=DIRECTION('ref_axis',(0.707106781186548,0.,-0.707106781186548));
#15528=DIRECTION('center_axis',(-1.,0.,1.95461800110063E-16));
#15529=DIRECTION('ref_axis',(1.95461800110063E-16,0.,1.));
#15530=DIRECTION('center_axis',(-1.,0.,0.));
#15531=DIRECTION('ref_axis',(0.,0.,1.));
#15532=DIRECTION('center_axis',(3.29601953873307E-15,0.,-1.));
#15533=DIRECTION('ref_axis',(-1.,0.,-3.29601953873307E-15));
#15534=DIRECTION('center_axis',(0.,0.,1.));
#15535=DIRECTION('ref_axis',(1.,0.,0.));
#15536=DIRECTION('center_axis',(0.,1.,0.));
#15537=DIRECTION('ref_axis',(0.,0.,1.));
#15538=DIRECTION('center_axis',(0.500076315108452,0.706998838849897,-0.500076315108454));
#15539=DIRECTION('ref_axis',(-0.707106781185304,-1.76214707967051E-12,-0.707106781187791));
#15540=DIRECTION('center_axis',(0.500078143315292,0.706996252576109,-0.500078143315292));
#15541=DIRECTION('ref_axis',(-2.6156794477156E-15,0.577470588096634,0.816411489313647));
#15542=DIRECTION('center_axis',(-0.928799626502546,0.370582317183012,0.));
#15543=DIRECTION('ref_axis',(0.370582317183012,0.928799626502546,0.));
#15544=DIRECTION('center_axis',(1.,0.,0.));
#15545=DIRECTION('ref_axis',(0.,0.,1.));
#15546=DIRECTION('center_axis',(0.,1.,0.));
#15547=DIRECTION('ref_axis',(1.,0.,0.));
#15548=DIRECTION('center_axis',(0.707106781186527,0.,0.707106781186568));
#15549=DIRECTION('ref_axis',(-0.707106781186568,-1.11022302462515E-14,0.707106781186527));
#15550=DIRECTION('center_axis',(-0.723101268110554,1.00350459623997E-14,
0.690742032930463));
#15551=DIRECTION('ref_axis',(-0.690742032930463,-1.66533453693774E-14,-0.723101268110554));
#15552=DIRECTION('center_axis',(0.,1.,0.));
#15553=DIRECTION('ref_axis',(-0.707106781186543,0.,-0.707106781186552));
#15554=DIRECTION('center_axis',(-0.707106781186534,0.,-0.707106781186561));
#15555=DIRECTION('ref_axis',(-0.707106781186561,0.,0.707106781186534));
#15556=DIRECTION('center_axis',(0.,1.,0.));
#15557=DIRECTION('ref_axis',(0.,0.,1.));
#15558=DIRECTION('center_axis',(0.,0.,1.));
#15559=DIRECTION('ref_axis',(1.,0.,0.));
#15560=DIRECTION('center_axis',(-3.41934671378744E-15,-0.16932895655699,
0.985559589508073));
#15561=DIRECTION('ref_axis',(2.22044604925031E-14,0.985559589508073,0.16932895655699));
#15562=DIRECTION('center_axis',(0.,1.,0.));
#15563=DIRECTION('ref_axis',(-0.999921859736202,0.,-0.0125009768296196));
#15564=DIRECTION('center_axis',(1.9135348438956E-14,1.,2.01169630281381E-14));
#15565=DIRECTION('ref_axis',(-3.99449913460614E-29,2.01169630281381E-14,
-1.));
#15566=DIRECTION('center_axis',(-0.689208106250273,-1.49735685222987E-16,
-0.724563445309596));
#15567=DIRECTION('ref_axis',(0.724563445309596,-3.33066907387544E-14,-0.689208106250273));
#15568=DIRECTION('center_axis',(-0.707106781186549,0.,0.707106781186546));
#15569=DIRECTION('ref_axis',(0.707106781186546,0.,0.707106781186549));
#15570=DIRECTION('center_axis',(0.707106781186548,0.,-0.707106781186548));
#15571=DIRECTION('ref_axis',(-0.707106781186548,0.,-0.707106781186548));
#15572=DIRECTION('center_axis',(1.,0.,-1.95461800110063E-16));
#15573=DIRECTION('ref_axis',(-1.95461800110063E-16,0.,-1.));
#15574=DIRECTION('center_axis',(1.,0.,0.));
#15575=DIRECTION('ref_axis',(0.,0.,-1.));
#15576=DIRECTION('center_axis',(-0.928799626502548,-0.370582317183008,0.));
#15577=DIRECTION('ref_axis',(0.370582317183008,-0.928799626502548,0.));
#15578=DIRECTION('center_axis',(0.,-1.,0.));
#15579=DIRECTION('ref_axis',(0.,0.,-1.));
#15580=DIRECTION('center_axis',(0.707106781186548,0.,0.707106781186547));
#15581=DIRECTION('ref_axis',(0.707106781186547,0.,-0.707106781186548));
#15582=DIRECTION('center_axis',(-0.707106781186547,0.,-0.707106781186548));
#15583=DIRECTION('ref_axis',(-0.707106781186548,0.,0.707106781186547));
#15584=DIRECTION('center_axis',(-0.707106781186554,0.,-0.707106781186541));
#15585=DIRECTION('ref_axis',(-0.707106781186541,0.,0.707106781186555));
#15586=DIRECTION('center_axis',(0.,1.,0.));
#15587=DIRECTION('ref_axis',(0.,0.,1.));
#15588=DIRECTION('center_axis',(-0.689521236687795,-4.82173031558679E-16,
0.724265465251888));
#15589=DIRECTION('ref_axis',(0.724265465251888,1.69629386130297E-30,0.689521236687795));
#15590=DIRECTION('center_axis',(0.,0.,1.));
#15591=DIRECTION('ref_axis',(1.,0.,0.));
#15592=DIRECTION('center_axis',(0.,0.,1.));
#15593=DIRECTION('ref_axis',(1.,0.,0.));
#15594=DIRECTION('center_axis',(-2.13887076994181E-15,0.169328956556989,
0.985559589508073));
#15595=DIRECTION('ref_axis',(3.73711604924882E-30,-0.985559589508073,0.169328956556989));
#15596=DIRECTION('center_axis',(0.,1.,0.));
#15597=DIRECTION('ref_axis',(0.,0.,1.));
#15598=DIRECTION('center_axis',(0.689208106250273,-1.34013438274573E-14,
-0.724563445309596));
#15599=DIRECTION('ref_axis',(-0.724563445309596,5.71414998426326E-29,-0.689208106250273));
#15600=DIRECTION('center_axis',(0.,1.,0.));
#15601=DIRECTION('ref_axis',(0.,0.,1.));
#15602=DIRECTION('center_axis',(1.47242188377274E-14,1.,-1.47242188377274E-14));
#15603=DIRECTION('ref_axis',(-7.97092275109852E-30,1.47242188377274E-14,
1.));
#15604=DIRECTION('center_axis',(-0.500065457858282,0.707014197674965,0.500065457858282));
#15605=DIRECTION('ref_axis',(6.38344604276266E-16,-0.577451054752767,0.816425305441298));
#15606=DIRECTION('center_axis',(0.50007814331533,-0.706996252576075,-0.500078143315302));
#15607=DIRECTION('ref_axis',(0.816411489313614,0.577470588096681,1.159905104889E-15));
#15608=DIRECTION('center_axis',(0.,1.,0.));
#15609=DIRECTION('ref_axis',(-0.999934544283097,0.,-0.0114414662240507));
#15610=DIRECTION('center_axis',(-0.690742032930436,0.,-0.72310126811058));
#15611=DIRECTION('ref_axis',(0.72310126811058,2.22044604925031E-14,-0.690742032930436));
#15612=DIRECTION('center_axis',(0.,-1.,0.));
#15613=DIRECTION('ref_axis',(0.,0.,-1.));
#15614=DIRECTION('center_axis',(0.,0.,1.));
#15615=DIRECTION('ref_axis',(1.,0.,0.));
#15616=DIRECTION('center_axis',(-1.,0.,0.));
#15617=DIRECTION('ref_axis',(0.,0.,-1.));
#15618=DIRECTION('center_axis',(0.,1.,0.));
#15619=DIRECTION('ref_axis',(1.,0.,0.));
#15620=DIRECTION('center_axis',(-0.500075464669968,0.707000041916711,-0.500075464669968));
#15621=DIRECTION('ref_axis',(2.74612154635474E-15,-0.577466463418753,-0.816414406797576));
#15622=DIRECTION('center_axis',(-1.17495566440827E-15,-0.16932895655699,
0.985559589508073));
#15623=DIRECTION('ref_axis',(2.22044604925031E-14,0.985559589508073,0.16932895655699));
#15624=DIRECTION('center_axis',(0.,0.,1.));
#15625=DIRECTION('ref_axis',(-1.,0.,0.));
#15626=DIRECTION('center_axis',(0.,1.,0.));
#15627=DIRECTION('ref_axis',(-0.999921859736202,0.,0.0125009768296196));
#15628=DIRECTION('center_axis',(-1.96322917836366E-14,1.,-1.96322917836366E-14));
#15629=DIRECTION('ref_axis',(-5.04975666092073E-29,-1.96322917836366E-14,
-1.));
#15630=DIRECTION('center_axis',(-0.500078143315344,-0.706996252576076,-0.500078143315287));
#15631=DIRECTION('ref_axis',(-0.816411489313608,0.57747058809669,2.88849236575815E-15));
#15632=DIRECTION('center_axis',(0.,1.,0.));
#15633=DIRECTION('ref_axis',(-0.999921859736202,0.,-0.0125009768296196));
#15634=DIRECTION('center_axis',(-0.689208106250266,4.79154192713555E-15,
-0.724563445309603));
#15635=DIRECTION('ref_axis',(0.724563445309603,1.06481884149609E-29,-0.689208106250266));
#15636=DIRECTION('center_axis',(0.,-1.,0.));
#15637=DIRECTION('ref_axis',(0.,0.,-1.));
#15638=DIRECTION('center_axis',(-3.29601953873307E-15,0.,1.));
#15639=DIRECTION('ref_axis',(1.,0.,3.29601953873307E-15));
#15640=DIRECTION('center_axis',(0.,0.,1.));
#15641=DIRECTION('ref_axis',(1.,0.,0.));
#15642=DIRECTION('center_axis',(1.,0.,-1.95461800110063E-16));
#15643=DIRECTION('ref_axis',(-1.95461800110063E-16,0.,-1.));
#15644=DIRECTION('center_axis',(-1.,0.,0.));
#15645=DIRECTION('ref_axis',(0.,0.,1.));
#15646=DIRECTION('center_axis',(-0.707106781186547,0.,-0.707106781186548));
#15647=DIRECTION('ref_axis',(-0.707106781186548,0.,0.707106781186547));
#15648=DIRECTION('center_axis',(-0.707106781186548,-3.92523114670943E-14,
-0.707106781186548));
#15649=DIRECTION('ref_axis',(-0.707106781186548,-1.49341426133556E-31,0.707106781186548));
#15650=DIRECTION('center_axis',(-0.500075562974082,0.706998150315597,-0.500078040676132));
#15651=DIRECTION('ref_axis',(0.512237467050394,0.70710678118697,0.487455410626653));
#15652=DIRECTION('center_axis',(-0.500078143315344,0.706996252576076,-0.500078143315287));
#15653=DIRECTION('ref_axis',(-0.816411489313608,-0.57747058809669,2.88849236575815E-15));
#15654=DIRECTION('center_axis',(0.,0.169328956556991,0.985559589508073));
#15655=DIRECTION('ref_axis',(0.,-0.985559589508073,0.169328956556991));
#15656=DIRECTION('center_axis',(3.29601953873307E-15,0.,-1.));
#15657=DIRECTION('ref_axis',(-1.,0.,-3.29601953873307E-15));
#15658=DIRECTION('center_axis',(0.,0.,1.));
#15659=DIRECTION('ref_axis',(-1.,0.,0.));
#15660=DIRECTION('center_axis',(0.,1.,0.));
#15661=DIRECTION('ref_axis',(0.,0.,1.));
#15662=DIRECTION('center_axis',(0.689521236687795,-4.82173031558679E-16,
-0.724265465251888));
#15663=DIRECTION('ref_axis',(-0.724265465251888,1.69629386130297E-30,-0.689521236687795));
#15664=DIRECTION('center_axis',(0.500075562974512,0.706998150315606,0.500078040675689));
#15665=DIRECTION('ref_axis',(-0.512237467041965,0.707106781187116,-0.487455410635299));
#15666=DIRECTION('center_axis',(-0.500075464669968,-0.707000041916711,-0.500075464669968));
#15667=DIRECTION('ref_axis',(2.74612154635474E-15,0.577466463418753,-0.816414406797576));
#15668=DIRECTION('center_axis',(0.,1.,0.));
#15669=DIRECTION('ref_axis',(0.,0.,1.));
#15670=DIRECTION('center_axis',(-1.43515113292173E-14,1.,1.50877222711036E-14));
#15671=DIRECTION('ref_axis',(-2.55233473732771E-30,-1.50877222711036E-14,
1.));
#15672=DIRECTION('center_axis',(0.,1.,0.));
#15673=DIRECTION('ref_axis',(0.,0.,1.));
#15674=DIRECTION('center_axis',(0.689208106250266,9.43334816904809E-15,
-0.724563445309603));
#15675=DIRECTION('ref_axis',(-0.724563445309603,2.1210382338014E-29,-0.689208106250266));
#15676=DIRECTION('center_axis',(0.,0.370582317183008,0.928799626502548));
#15677=DIRECTION('ref_axis',(-2.22044604925031E-14,0.928799626502548,-0.370582317183008));
#15678=DIRECTION('center_axis',(0.,-1.,0.));
#15679=DIRECTION('ref_axis',(0.,0.,-1.));
#15680=DIRECTION('center_axis',(0.,0.,1.));
#15681=DIRECTION('ref_axis',(1.,0.,0.));
#15682=DIRECTION('center_axis',(0.,1.,0.));
#15683=DIRECTION('ref_axis',(1.,0.,0.));
#15684=DIRECTION('center_axis',(-0.500065457858323,-0.707014197674947,-0.500065457858266));
#15685=DIRECTION('ref_axis',(-0.816425305441277,0.577451054752798,2.3871826158738E-14));
#15686=DIRECTION('center_axis',(0.690742032930456,0.,-0.723101268110561));
#15687=DIRECTION('ref_axis',(0.723101268110561,5.55111512312578E-15,0.690742032930456));
#15688=DIRECTION('center_axis',(0.,1.,0.));
#15689=DIRECTION('ref_axis',(1.,0.,0.));
#15690=DIRECTION('center_axis',(0.689208106250273,1.34013438274573E-14,
-0.724563445309596));
#15691=DIRECTION('ref_axis',(0.724563445309596,-6.10622663543829E-14,0.689208106250273));
#15692=DIRECTION('center_axis',(1.96322917836366E-14,1.,1.96322917836366E-14));
#15693=DIRECTION('ref_axis',(-5.04975666092073E-29,1.96322917836366E-14,
-1.));
#15694=DIRECTION('center_axis',(0.,0.,1.));
#15695=DIRECTION('ref_axis',(-1.,0.,0.));
#15696=DIRECTION('center_axis',(0.,1.,0.));
#15697=DIRECTION('ref_axis',(0.,0.,1.));
#15698=DIRECTION('center_axis',(-1.,0.,0.));
#15699=DIRECTION('ref_axis',(0.,0.,1.));
#15700=DIRECTION('center_axis',(0.,1.,0.));
#15701=DIRECTION('ref_axis',(-0.999924538176025,0.,0.0122848668475855));
#15702=DIRECTION('center_axis',(-0.707106781186554,0.,-0.707106781186541));
#15703=DIRECTION('ref_axis',(0.707106781186541,0.,-0.707106781186555));
#15704=DIRECTION('center_axis',(0.,1.,0.));
#15705=DIRECTION('ref_axis',(-0.999921859736202,0.,0.0125009768296196));
#15706=DIRECTION('center_axis',(-0.500078143315298,0.7069962525761,-0.500078143315298));
#15707=DIRECTION('ref_axis',(-7.12726278488012E-16,-0.577470588096643,-0.816411489313641));
#15708=DIRECTION('center_axis',(0.,-0.370582317183023,0.928799626502542));
#15709=DIRECTION('ref_axis',(0.,-0.928799626502542,-0.370582317183023));
#15710=DIRECTION('center_axis',(0.,0.,-1.));
#15711=DIRECTION('ref_axis',(-1.,0.,0.));
#15712=DIRECTION('center_axis',(0.,0.,1.));
#15713=DIRECTION('ref_axis',(1.,0.,0.));
#15714=DIRECTION('center_axis',(0.,-1.,0.));
#15715=DIRECTION('ref_axis',(0.,0.,-1.));
#15716=DIRECTION('center_axis',(-0.500078143315298,-0.7069962525761,-0.500078143315298));
#15717=DIRECTION('ref_axis',(-2.68615379510983E-16,0.577470588096642,-0.816411489313641));
#15718=DIRECTION('center_axis',(0.,1.,0.));
#15719=DIRECTION('ref_axis',(0.,0.,1.));
#15720=DIRECTION('center_axis',(1.43515113292173E-14,1.,-1.50877222711036E-14));
#15721=DIRECTION('ref_axis',(-2.55233473732771E-30,1.50877222711036E-14,
1.));
#15722=DIRECTION('center_axis',(0.,1.,0.));
#15723=DIRECTION('ref_axis',(0.,0.,1.));
#15724=DIRECTION('center_axis',(-0.689208106250259,-5.54022035325041E-15,
-0.724563445309609));
#15725=DIRECTION('ref_axis',(-0.72456344530961,-4.03502369944906E-29,0.689208106250259));
#15726=DIRECTION('center_axis',(-0.500076315109219,0.706998838848823,0.500076315109206));
#15727=DIRECTION('ref_axis',(0.707106781184693,-2.61479889240196E-12,0.707106781188402));
#15728=DIRECTION('center_axis',(0.500075464669981,-0.707000041916716,-0.500075464669948));
#15729=DIRECTION('ref_axis',(0.816414406797569,0.577466463418763,-2.91626173010388E-15));
#15730=DIRECTION('center_axis',(-0.5000781433153,0.706996252576104,0.50007814331529));
#15731=DIRECTION('ref_axis',(-0.816411489313642,-0.577470588096642,-1.83698748637925E-16));
#15732=DIRECTION('center_axis',(0.,1.,0.));
#15733=DIRECTION('ref_axis',(0.,0.,1.));
#15734=DIRECTION('center_axis',(-0.689521236687795,0.,-0.724265465251888));
#15735=DIRECTION('ref_axis',(-0.724265465251888,0.,0.689521236687795));
#15736=DIRECTION('center_axis',(0.,0.,1.));
#15737=DIRECTION('ref_axis',(1.,0.,0.));
#15738=DIRECTION('center_axis',(0.,2.77555756156289E-14,1.));
#15739=DIRECTION('ref_axis',(0.,-1.,2.77555756156289E-14));
#15740=DIRECTION('center_axis',(1.,0.,-1.95461800110063E-16));
#15741=DIRECTION('ref_axis',(-1.95461800110063E-16,0.,-1.));
#15742=DIRECTION('center_axis',(-1.,0.,0.));
#15743=DIRECTION('ref_axis',(0.,0.,1.));
#15744=DIRECTION('center_axis',(0.707106781186547,0.,0.707106781186548));
#15745=DIRECTION('ref_axis',(0.707106781186548,0.,-0.707106781186547));
#15746=DIRECTION('center_axis',(-0.500065457858323,0.707014197674947,-0.500065457858266));
#15747=DIRECTION('ref_axis',(-0.816425305441268,-0.57745105475281,-2.24141339905632E-15));
#15748=DIRECTION('center_axis',(0.,-1.,0.));
#15749=DIRECTION('ref_axis',(0.,0.,-1.));
#15750=DIRECTION('center_axis',(0.690742032930456,0.,-0.723101268110561));
#15751=DIRECTION('ref_axis',(-0.723101268110561,0.,-0.690742032930456));
#15752=DIRECTION('center_axis',(0.,0.,1.));
#15753=DIRECTION('ref_axis',(-1.,0.,0.));
#15754=DIRECTION('center_axis',(0.,0.370582317183012,0.928799626502546));
#15755=DIRECTION('ref_axis',(2.22044604925031E-14,0.928799626502546,-0.370582317183012));
#15756=DIRECTION('center_axis',(0.,1.,0.));
#15757=DIRECTION('ref_axis',(1.,0.,0.));
#15758=DIRECTION('center_axis',(0.689208106250266,-9.43334816904809E-15,
-0.724563445309603));
#15759=DIRECTION('ref_axis',(0.724563445309603,-1.38777878078143E-15,0.689208106250266));
#15760=DIRECTION('center_axis',(0.,1.,0.));
#15761=DIRECTION('ref_axis',(1.,0.,0.));
#15762=DIRECTION('center_axis',(-1.91353484389562E-14,1.,-2.01169630281383E-14));
#15763=DIRECTION('ref_axis',(-3.99449913460581E-29,-2.01169630281383E-14,
-1.));
#15764=DIRECTION('center_axis',(0.,1.,0.));
#15765=DIRECTION('ref_axis',(1.,0.,0.));
#15766=DIRECTION('center_axis',(0.707106781186554,-3.92523114670943E-14,
-0.707106781186541));
#15767=DIRECTION('ref_axis',(0.707106781186541,-3.33066907387542E-14,0.707106781186555));
#15768=DIRECTION('center_axis',(0.,1.,0.));
#15769=DIRECTION('ref_axis',(0.,0.,1.));
#15770=DIRECTION('center_axis',(1.,0.,0.));
#15771=DIRECTION('ref_axis',(0.,0.,-1.));
#15772=DIRECTION('center_axis',(-0.985559589508072,-0.169328956556993,0.));
#15773=DIRECTION('ref_axis',(-0.169328956556993,0.985559589508072,2.22044604925031E-14));
#15774=DIRECTION('center_axis',(0.,1.,0.));
#15775=DIRECTION('ref_axis',(-0.999934544283124,0.,0.0114414662216631));
#15776=DIRECTION('center_axis',(-0.707106781186548,3.92523114670943E-14,
-0.707106781186548));
#15777=DIRECTION('ref_axis',(0.707106781186548,-1.49341426133556E-31,-0.707106781186548));
#15778=DIRECTION('center_axis',(-3.29601953873307E-15,0.,1.));
#15779=DIRECTION('ref_axis',(1.,0.,3.29601953873307E-15));
#15780=DIRECTION('center_axis',(0.,0.,1.));
#15781=DIRECTION('ref_axis',(-1.,0.,0.));
#15782=DIRECTION('center_axis',(0.,-0.370582317183008,0.928799626502548));
#15783=DIRECTION('ref_axis',(0.,-0.928799626502548,-0.370582317183008));
#15784=DIRECTION('center_axis',(0.,1.,0.));
#15785=DIRECTION('ref_axis',(0.,0.,1.));
#15786=DIRECTION('center_axis',(-0.689208106250266,3.72093177779119E-14,
-0.724563445309603));
#15787=DIRECTION('ref_axis',(-0.724563445309603,-8.3586004851558E-29,0.689208106250266));
#15788=DIRECTION('center_axis',(0.,1.,0.));
#15789=DIRECTION('ref_axis',(0.,0.,1.));
#15790=DIRECTION('center_axis',(-1.47242188377277E-14,1.,1.47242188377274E-14));
#15791=DIRECTION('ref_axis',(-1.,-1.47242188377277E-14,7.9709227510944E-30));
#15792=DIRECTION('center_axis',(0.707106781186554,0.,-0.707106781186541));
#15793=DIRECTION('ref_axis',(-0.707106781186541,0.,-0.707106781186554));
#15794=DIRECTION('center_axis',(1.,0.,-1.95461800110063E-16));
#15795=DIRECTION('ref_axis',(-1.95461800110063E-16,0.,-1.));
#15796=DIRECTION('center_axis',(1.,0.,0.));
#15797=DIRECTION('ref_axis',(0.,0.,-1.));
#15798=DIRECTION('center_axis',(-0.985559589508073,0.169328956556991,-1.055202794374E-16));
#15799=DIRECTION('ref_axis',(-0.169328956556991,-0.985559589508073,-2.75791750167464E-32));
#15800=DIRECTION('center_axis',(0.,1.,0.));
#15801=DIRECTION('ref_axis',(0.,0.,1.));
#15802=DIRECTION('center_axis',(-0.724265465251897,0.,0.689521236687785));
#15803=DIRECTION('ref_axis',(0.689521236687785,0.,0.724265465251897));
#15804=DIRECTION('center_axis',(-0.707106781186548,0.,-0.707106781186547));
#15805=DIRECTION('ref_axis',(-0.707106781186547,0.,0.707106781186548));
#15806=DIRECTION('center_axis',(0.707106781186548,0.,0.707106781186548));
#15807=DIRECTION('ref_axis',(0.707106781186548,0.,-0.707106781186548));
#15808=DIRECTION('center_axis',(0.707106781186547,0.,0.707106781186548));
#15809=DIRECTION('ref_axis',(0.707106781186548,0.,-0.707106781186547));
#15810=DIRECTION('center_axis',(-0.707106781186548,0.,-0.707106781186548));
#15811=DIRECTION('ref_axis',(-0.707106781186548,0.,0.707106781186548));
#15812=DIRECTION('center_axis',(0.,-1.,0.));
#15813=DIRECTION('ref_axis',(0.,0.,-1.));
#15814=DIRECTION('center_axis',(-1.,0.,0.));
#15815=DIRECTION('ref_axis',(0.,0.,1.));
#15816=DIRECTION('center_axis',(0.,0.,1.));
#15817=DIRECTION('ref_axis',(-1.,0.,0.));
#15818=DIRECTION('center_axis',(0.,1.,0.));
#15819=DIRECTION('ref_axis',(1.,0.,0.));
#15820=DIRECTION('center_axis',(0.500078143315342,0.706996252576075,-0.50007814331529));
#15821=DIRECTION('ref_axis',(0.816411489313607,-0.577470588096692,-3.592237284197E-15));
#15822=DIRECTION('center_axis',(0.,1.,0.));
#15823=DIRECTION('ref_axis',(1.,0.,0.));
#15824=DIRECTION('center_axis',(0.50007546466997,0.707000041916716,0.50007546466996));
#15825=DIRECTION('ref_axis',(0.816414406797577,-0.577466463418752,-1.98804944403104E-15));
#15826=DIRECTION('center_axis',(0.,-1.,0.));
#15827=DIRECTION('ref_axis',(0.707106781186548,0.,0.707106781186548));
#15828=DIRECTION('center_axis',(0.707106781186561,0.,0.707106781186534));
#15829=DIRECTION('ref_axis',(0.707106781186534,0.,-0.707106781186561));
#15830=DIRECTION('center_axis',(-1.,0.,1.95461800110063E-16));
#15831=DIRECTION('ref_axis',(1.95461800110063E-16,0.,1.));
#15832=DIRECTION('center_axis',(-1.,0.,0.));
#15833=DIRECTION('ref_axis',(0.,0.,1.));
#15834=DIRECTION('center_axis',(0.,0.,-1.));
#15835=DIRECTION('ref_axis',(-1.,0.,0.));
#15836=DIRECTION('center_axis',(-2.77555756156289E-14,0.,1.));
#15837=DIRECTION('ref_axis',(1.,0.,2.77555756156289E-14));
#15838=DIRECTION('center_axis',(0.,-1.,0.));
#15839=DIRECTION('ref_axis',(0.,0.,-1.));
#15840=DIRECTION('center_axis',(-0.690742032930428,1.0933195161307E-14,
-0.723101268110587));
#15841=DIRECTION('ref_axis',(-0.723101268110587,-7.09354204639614E-29,0.690742032930428));
#15842=DIRECTION('center_axis',(0.500065457858296,0.707014197674951,-0.500065457858286));
#15843=DIRECTION('ref_axis',(-0.816425305441284,0.577451054752786,1.01752225400829E-15));
#15844=DIRECTION('center_axis',(-0.707106781186556,0.,0.707106781186539));
#15845=DIRECTION('ref_axis',(0.707106781186539,0.,0.707106781186556));
#15846=DIRECTION('center_axis',(-0.707106781186541,0.,0.707106781186554));
#15847=DIRECTION('ref_axis',(0.707106781186554,0.,0.707106781186541));
#15848=DIRECTION('center_axis',(0.,1.,0.));
#15849=DIRECTION('ref_axis',(0.,0.,1.));
#15850=DIRECTION('center_axis',(0.724265465251865,1.96202318550286E-14,
0.68952123668782));
#15851=DIRECTION('ref_axis',(0.68952123668782,-2.20983281568644E-29,-0.724265465251865));
#15852=DIRECTION('center_axis',(0.500076315110995,0.706998838846295,0.500076315111003));
#15853=DIRECTION('ref_axis',(0.707106781192132,-7.88702926797483E-12,-0.707106781180963));
#15854=DIRECTION('center_axis',(0.500078143315295,0.706996252576104,0.500078143315295));
#15855=DIRECTION('ref_axis',(1.82105156671187E-15,-0.577470588096639,0.816411489313644));
#15856=DIRECTION('center_axis',(-0.707106781186548,0.,-0.707106781186547));
#15857=DIRECTION('ref_axis',(-0.707106781186547,0.,0.707106781186548));
#15858=DIRECTION('center_axis',(0.707106781186527,0.,0.707106781186568));
#15859=DIRECTION('ref_axis',(0.707106781186568,0.,-0.707106781186527));
#15860=DIRECTION('center_axis',(0.,-1.,0.));
#15861=DIRECTION('ref_axis',(0.,0.,-1.));
#15862=DIRECTION('center_axis',(-0.723101268110554,-1.00350459623997E-14,
0.690742032930463));
#15863=DIRECTION('ref_axis',(0.690742032930463,-8.19100136791555E-29,0.723101268110554));
#15864=DIRECTION('center_axis',(-0.928799626502548,0.370582317183008,0.));
#15865=DIRECTION('ref_axis',(0.370582317183008,0.928799626502548,-2.22044604925031E-14));
#15866=DIRECTION('center_axis',(0.,-1.,0.));
#15867=DIRECTION('ref_axis',(0.,0.,-1.));
#15868=DIRECTION('center_axis',(1.,0.,0.));
#15869=DIRECTION('ref_axis',(0.,0.,-1.));
#15870=DIRECTION('center_axis',(0.,1.,0.));
#15871=DIRECTION('ref_axis',(1.,0.,0.));
#15872=DIRECTION('center_axis',(0.707106781186554,0.,-0.707106781186541));
#15873=DIRECTION('ref_axis',(0.707106781186541,0.,0.707106781186555));
#15874=DIRECTION('center_axis',(0.,1.,0.));
#15875=DIRECTION('ref_axis',(1.,0.,0.));
#15876=DIRECTION('center_axis',(-0.50007546466996,0.707000041916729,0.50007546466995));
#15877=DIRECTION('ref_axis',(0.816414406797587,0.577466463418738,-1.14723735947441E-16));
#15878=DIRECTION('center_axis',(0.,1.,0.));
#15879=DIRECTION('ref_axis',(1.,0.,0.));
#15880=DIRECTION('center_axis',(-2.01169630281381E-14,1.,1.91353484389564E-14));
#15881=DIRECTION('ref_axis',(1.,2.01169630281381E-14,-3.99449913460622E-29));
#15882=DIRECTION('center_axis',(0.,1.,0.));
#15883=DIRECTION('ref_axis',(1.,0.,0.));
#15884=DIRECTION('center_axis',(0.50006545785829,-0.707014197674953,0.50006545785829));
#15885=DIRECTION('ref_axis',(1.98508446711413E-15,0.577451054752781,0.816425305441288));
#15886=DIRECTION('center_axis',(-0.928799626502548,-0.370582317183008,0.));
#15887=DIRECTION('ref_axis',(0.370582317183008,-0.928799626502548,0.));
#15888=DIRECTION('center_axis',(-1.,0.,1.95461800110063E-16));
#15889=DIRECTION('ref_axis',(1.95461800110063E-16,0.,1.));
#15890=DIRECTION('center_axis',(1.,0.,0.));
#15891=DIRECTION('ref_axis',(0.,0.,-1.));
#15892=DIRECTION('center_axis',(0.707106781186554,0.,-0.707106781186541));
#15893=DIRECTION('ref_axis',(-0.707106781186541,0.,-0.707106781186554));
#15894=DIRECTION('center_axis',(0.707106781186554,-9.81307786677349E-15,
-0.707106781186541));
#15895=DIRECTION('ref_axis',(-0.707106781186541,-9.64572967081383E-29,-0.707106781186555));
#15896=DIRECTION('center_axis',(-0.50007804067718,0.706998150315576,0.500075562973064));
#15897=DIRECTION('ref_axis',(0.487455410632167,0.707106781187069,-0.512237467045011));
#15898=DIRECTION('center_axis',(-0.500078143315285,0.706996252576076,0.500078143315346));
#15899=DIRECTION('ref_axis',(-1.79407009105894E-15,-0.577470588096693,0.816411489313605));
#15900=DIRECTION('center_axis',(0.,1.,0.));
#15901=DIRECTION('ref_axis',(0.0125009768296248,0.,-0.999921859736202));
#15902=DIRECTION('center_axis',(1.47242188377274E-14,1.,1.47242188377274E-14));
#15903=DIRECTION('ref_axis',(7.97092275109852E-30,-1.47242188377274E-14,
1.));
#15904=DIRECTION('center_axis',(0.50007814331529,-0.706996252576075,0.500078143315342));
#15905=DIRECTION('ref_axis',(2.42101966234701E-15,-0.577470588096689,-0.816411489313609));
#15906=DIRECTION('center_axis',(0.,-1.,0.));
#15907=DIRECTION('ref_axis',(-0.707106781186559,0.,0.707106781186536));
#15908=DIRECTION('center_axis',(-0.707106781186548,1.96261557335473E-14,
0.707106781186548));
#15909=DIRECTION('ref_axis',(0.707106781186548,-3.26127331168573E-31,0.707106781186548));
#15910=DIRECTION('center_axis',(0.,1.,0.));
#15911=DIRECTION('ref_axis',(1.,0.,0.));
#15912=DIRECTION('center_axis',(1.96322917836368E-14,1.,-1.96322917836364E-14));
#15913=DIRECTION('ref_axis',(1.,-1.96322917836368E-14,-5.0497566609203E-29));
#15914=DIRECTION('center_axis',(0.,1.,0.));
#15915=DIRECTION('ref_axis',(1.,0.,0.));
#15916=DIRECTION('center_axis',(0.,-1.,0.));
#15917=DIRECTION('ref_axis',(0.,0.,-1.));
#15918=DIRECTION('center_axis',(0.723101268110551,0.,0.690742032930466));
#15919=DIRECTION('ref_axis',(0.690742032930466,0.,-0.723101268110551));
#15920=DIRECTION('center_axis',(-0.707106781186556,0.,0.707106781186539));
#15921=DIRECTION('ref_axis',(0.707106781186539,0.,0.707106781186556));
#15922=DIRECTION('center_axis',(-0.707106781186548,-9.81307786677359E-15,
0.707106781186548));
#15923=DIRECTION('ref_axis',(0.707106781186548,3.73353565333889E-32,0.707106781186548));
#15924=DIRECTION('center_axis',(0.,1.,0.));
#15925=DIRECTION('ref_axis',(-0.0125009768300713,0.,-0.999921859736197));
#15926=DIRECTION('center_axis',(-1.63450324603621E-14,1.,-1.55474706066522E-14));
#15927=DIRECTION('ref_axis',(-1.,-1.63450324603621E-14,-4.79348589056631E-30));
#15928=DIRECTION('center_axis',(0.,1.,0.));
#15929=DIRECTION('ref_axis',(1.,0.,0.));
#15930=DIRECTION('center_axis',(-0.500065457858285,-0.707014197674951,0.500065457858298));
#15931=DIRECTION('ref_axis',(-3.21586666640058E-16,0.577451054752787,0.816425305441284));
#15932=DIRECTION('center_axis',(0.,1.,0.));
#15933=DIRECTION('ref_axis',(1.,0.,0.));
#15934=DIRECTION('center_axis',(0.500078143315307,0.706996252576094,-0.500078143315297));
#15935=DIRECTION('ref_axis',(0.816411489313626,-0.577470588096664,-2.37338946977257E-14));
#15936=DIRECTION('center_axis',(-0.0822611166573126,0.0232075739978801,
0.996340562857613));
#15937=DIRECTION('ref_axis',(-0.996607302542098,0.000737174162972365,-0.0823003104126366));
#15938=DIRECTION('center_axis',(-0.99634056285741,0.0232075739985405,0.0822611166595799));
#15939=DIRECTION('ref_axis',(0.0848772062239051,0.382000889613703,0.920256040565866));
#15940=DIRECTION('center_axis',(0.996340562857634,0.0232075739980609,0.0822611166570035));
#15941=DIRECTION('ref_axis',(-0.082300310412331,0.000737174163135013,0.996607302542123));
#15942=DIRECTION('center_axis',(1.,0.,0.));
#15943=DIRECTION('ref_axis',(0.,0.,-1.));
#15944=DIRECTION('center_axis',(1.,0.,0.));
#15945=DIRECTION('ref_axis',(0.,0.,-1.));
#15946=DIRECTION('center_axis',(-1.,0.,0.));
#15947=DIRECTION('ref_axis',(0.,0.,1.));
#15948=DIRECTION('center_axis',(0.905882352941173,0.,0.423529411764713));
#15949=DIRECTION('ref_axis',(-0.423529411764713,0.,0.905882352941173));
#15950=DIRECTION('center_axis',(-0.905882352941173,0.,0.423529411764713));
#15951=DIRECTION('ref_axis',(-0.423529411764713,0.,-0.905882352941173));
#15952=DIRECTION('center_axis',(0.,1.,0.));
#15953=DIRECTION('ref_axis',(0.,0.,1.));
#15954=DIRECTION('center_axis',(0.423529411764713,0.,0.905882352941173));
#15955=DIRECTION('ref_axis',(0.905882352941173,0.,-0.423529411764713));
#15956=DIRECTION('center_axis',(-3.49148133884313E-15,0.,1.));
#15957=DIRECTION('ref_axis',(1.,0.,3.49148133884313E-15));
#15958=DIRECTION('center_axis',(0.,0.,1.));
#15959=DIRECTION('ref_axis',(1.,0.,0.));
#15960=DIRECTION('center_axis',(0.,0.,-1.));
#15961=DIRECTION('ref_axis',(-1.,0.,0.));
#15962=DIRECTION('center_axis',(0.,1.,0.));
#15963=DIRECTION('ref_axis',(0.,0.,1.));
#15964=DIRECTION('center_axis',(-0.423529411764713,0.,0.905882352941173));
#15965=DIRECTION('ref_axis',(0.905882352941173,0.,0.423529411764713));
#15966=DIRECTION('center_axis',(-0.423529411764713,0.,0.905882352941173));
#15967=DIRECTION('ref_axis',(-0.905882352941173,6.66133814775091E-14,-0.423529411764713));
#15968=DIRECTION('center_axis',(0.,0.,1.));
#15969=DIRECTION('ref_axis',(-1.,0.,0.));
#15970=DIRECTION('center_axis',(0.,1.,0.));
#15971=DIRECTION('ref_axis',(0.,0.,1.));
#15972=DIRECTION('center_axis',(0.,1.,0.));
#15973=DIRECTION('ref_axis',(0.,0.,1.));
#15974=DIRECTION('center_axis',(0.,1.,0.));
#15975=DIRECTION('ref_axis',(0.,0.,1.));
#15976=DIRECTION('center_axis',(-0.905882352941173,0.,0.423529411764713));
#15977=DIRECTION('ref_axis',(0.423529411764713,0.,0.905882352941173));
#15978=DIRECTION('center_axis',(0.,0.,-1.));
#15979=DIRECTION('ref_axis',(-1.,0.,0.));
#15980=DIRECTION('center_axis',(0.,0.,1.));
#15981=DIRECTION('ref_axis',(1.,0.,0.));
#15982=DIRECTION('center_axis',(0.0822611166581281,0.0232075739987885,0.996340562857524));
#15983=DIRECTION('ref_axis',(0.920256040566017,0.382000889613614,-0.0848772062226595));
#15984=DIRECTION('center_axis',(-1.,0.,0.));
#15985=DIRECTION('ref_axis',(0.,-1.56541446472147E-12,-1.));
#15986=DIRECTION('center_axis',(0.423529411764713,0.,0.905882352941173));
#15987=DIRECTION('ref_axis',(-0.905882352941173,4.44089209850061E-14,0.423529411764713));
#15988=DIRECTION('center_axis',(0.,1.,0.));
#15989=DIRECTION('ref_axis',(0.,0.,1.));
#15990=DIRECTION('center_axis',(0.,1.,0.));
#15991=DIRECTION('ref_axis',(0.,0.,1.));
#15992=DIRECTION('center_axis',(-1.,0.,0.));
#15993=DIRECTION('ref_axis',(0.,0.,1.));
#15994=DIRECTION('center_axis',(-1.,0.,0.));
#15995=DIRECTION('ref_axis',(0.,0.,1.));
#15996=DIRECTION('center_axis',(0.,1.,0.));
#15997=DIRECTION('ref_axis',(0.,0.,1.));
#15998=DIRECTION('center_axis',(0.905882352941173,0.,0.423529411764713));
#15999=DIRECTION('ref_axis',(0.423529411764713,0.,-0.905882352941173));
#16000=DIRECTION('center_axis',(0.997972229653585,-0.0634588605921735,0.00493982313395358));
#16001=DIRECTION('ref_axis',(-0.028904578164028,-0.382679269643752,0.923428991285244));
#16002=DIRECTION('center_axis',(0.,1.,0.));
#16003=DIRECTION('ref_axis',(0.,0.,1.));
#16004=DIRECTION('center_axis',(0.,0.,1.));
#16005=DIRECTION('ref_axis',(1.,0.,0.));
#16006=DIRECTION('center_axis',(-1.,0.,0.));
#16007=DIRECTION('ref_axis',(0.,0.,1.));
#16008=DIRECTION('center_axis',(-1.,0.,1.95461800110063E-16));
#16009=DIRECTION('ref_axis',(1.95461800110063E-16,0.,1.));
#16010=DIRECTION('center_axis',(-1.,0.,0.));
#16011=DIRECTION('ref_axis',(0.,0.,1.));
#16012=DIRECTION('center_axis',(3.29601953873307E-15,0.,-1.));
#16013=DIRECTION('ref_axis',(-1.,0.,-3.29601953873307E-15));
#16014=DIRECTION('center_axis',(0.,0.,1.));
#16015=DIRECTION('ref_axis',(-1.,0.,0.));
#16016=DIRECTION('center_axis',(0.,1.,0.));
#16017=DIRECTION('ref_axis',(0.,0.,1.));
#16018=DIRECTION('center_axis',(0.,0.,1.));
#16019=DIRECTION('ref_axis',(1.,0.,0.));
#16020=DIRECTION('center_axis',(0.,1.,0.));
#16021=DIRECTION('ref_axis',(0.,0.,1.));
#16022=DIRECTION('center_axis',(-1.,0.,0.));
#16023=DIRECTION('ref_axis',(0.,0.,1.));
#16024=DIRECTION('center_axis',(0.,0.,1.));
#16025=DIRECTION('ref_axis',(1.,0.,0.));
#16026=DIRECTION('center_axis',(0.,2.77555756156289E-14,1.));
#16027=DIRECTION('ref_axis',(0.,-1.,2.77555756156289E-14));
#16028=DIRECTION('center_axis',(1.,0.,-1.95461800110063E-16));
#16029=DIRECTION('ref_axis',(-1.95461800110063E-16,0.,-1.));
#16030=DIRECTION('center_axis',(-1.,0.,0.));
#16031=DIRECTION('ref_axis',(0.,0.,1.));
#16032=DIRECTION('center_axis',(0.,1.,0.));
#16033=DIRECTION('ref_axis',(0.,0.,1.));
#16034=DIRECTION('center_axis',(0.,1.,0.));
#16035=DIRECTION('ref_axis',(0.,0.,1.));
#16036=DIRECTION('center_axis',(0.,0.,1.));
#16037=DIRECTION('ref_axis',(1.,0.,0.));
#16038=DIRECTION('center_axis',(-1.,0.,0.));
#16039=DIRECTION('ref_axis',(0.,0.,1.));
#16040=DIRECTION('center_axis',(1.,0.,-1.95461800110063E-16));
#16041=DIRECTION('ref_axis',(-1.95461800110063E-16,0.,-1.));
#16042=DIRECTION('center_axis',(-1.,0.,0.));
#16043=DIRECTION('ref_axis',(0.,0.,1.));
#16044=DIRECTION('center_axis',(-3.29601953873307E-15,0.,1.));
#16045=DIRECTION('ref_axis',(1.,0.,3.29601953873307E-15));
#16046=DIRECTION('center_axis',(0.,0.,1.));
#16047=DIRECTION('ref_axis',(-1.,0.,0.));
#16048=DIRECTION('center_axis',(0.,1.,0.));
#16049=DIRECTION('ref_axis',(0.,0.,1.));
#16050=DIRECTION('center_axis',(0.,0.,1.));
#16051=DIRECTION('ref_axis',(1.,0.,0.));
#16052=DIRECTION('center_axis',(0.,1.,0.));
#16053=DIRECTION('ref_axis',(0.,0.,1.));
#16054=DIRECTION('center_axis',(-1.,0.,0.));
#16055=DIRECTION('ref_axis',(0.,0.,1.));
#16056=DIRECTION('center_axis',(0.,0.,-1.));
#16057=DIRECTION('ref_axis',(-1.,0.,0.));
#16058=DIRECTION('center_axis',(-2.77555756156289E-14,0.,1.));
#16059=DIRECTION('ref_axis',(1.,0.,2.77555756156289E-14));
#16060=DIRECTION('center_axis',(-1.,0.,1.95461800110063E-16));
#16061=DIRECTION('ref_axis',(1.95461800110063E-16,0.,1.));
#16062=DIRECTION('center_axis',(-1.,0.,0.));
#16063=DIRECTION('ref_axis',(0.,0.,1.));
#16064=DIRECTION('center_axis',(0.,1.,0.));
#16065=DIRECTION('ref_axis',(0.,0.,1.));
#16066=DIRECTION('center_axis',(0.,1.,0.));
#16067=DIRECTION('ref_axis',(-0.707106781186548,0.,-0.707106781186548));
#16068=DIRECTION('center_axis',(0.588235294117631,0.,0.80868982852163));
#16069=DIRECTION('ref_axis',(0.80868982852163,0.,-0.588235294117631));
#16070=DIRECTION('center_axis',(0.,1.,0.));
#16071=DIRECTION('ref_axis',(0.,0.,1.));
#16072=DIRECTION('center_axis',(-1.,0.,0.));
#16073=DIRECTION('ref_axis',(0.,0.,1.));
#16074=DIRECTION('center_axis',(0.,0.,1.));
#16075=DIRECTION('ref_axis',(1.,0.,0.));
#16076=DIRECTION('center_axis',(0.,0.,1.));
#16077=DIRECTION('ref_axis',(-1.,0.,0.));
#16078=DIRECTION('center_axis',(0.,0.,-1.));
#16079=DIRECTION('ref_axis',(-1.,0.,0.));
#16080=DIRECTION('center_axis',(-1.,0.,-1.03892784411108E-15));
#16081=DIRECTION('ref_axis',(-1.03892784411108E-15,0.,1.));
#16082=DIRECTION('center_axis',(-1.,0.,0.));
#16083=DIRECTION('ref_axis',(0.,0.,1.));
#16084=DIRECTION('center_axis',(0.,1.,0.));
#16085=DIRECTION('ref_axis',(0.27462518896381,0.,-0.961551353587832));
#16086=DIRECTION('center_axis',(-0.528132444354927,1.46586199943601E-14,
0.849162011173186));
#16087=DIRECTION('ref_axis',(0.849162011173186,-1.56277058526093E-29,0.528132444354927));
#16088=DIRECTION('center_axis',(0.,1.,0.));
#16089=DIRECTION('ref_axis',(0.,0.,1.));
#16090=DIRECTION('center_axis',(0.849162011173186,0.,-0.528132444354927));
#16091=DIRECTION('ref_axis',(-0.528132444354927,0.,-0.849162011173186));
#16092=DIRECTION('center_axis',(0.,1.,0.));
#16093=DIRECTION('ref_axis',(0.,0.,1.));
#16094=DIRECTION('center_axis',(0.,1.,0.));
#16095=DIRECTION('ref_axis',(-0.707106781186547,0.,-0.707106781186548));
#16096=DIRECTION('center_axis',(-0.588235294117645,0.,-0.808689828521621));
#16097=DIRECTION('ref_axis',(-0.808689828521621,0.,0.588235294117644));
#16098=DIRECTION('center_axis',(0.,1.,0.));
#16099=DIRECTION('ref_axis',(0.,0.,1.));
#16100=DIRECTION('center_axis',(1.,0.,0.));
#16101=DIRECTION('ref_axis',(0.,0.,-1.));
#16102=DIRECTION('center_axis',(0.,0.,-1.));
#16103=DIRECTION('ref_axis',(-1.,0.,0.));
#16104=DIRECTION('center_axis',(0.,0.,1.));
#16105=DIRECTION('ref_axis',(-1.,0.,0.));
#16106=DIRECTION('center_axis',(0.,0.,1.));
#16107=DIRECTION('ref_axis',(1.,0.,0.));
#16108=DIRECTION('center_axis',(1.,0.,1.03892784411108E-15));
#16109=DIRECTION('ref_axis',(1.03892784411108E-15,0.,-1.));
#16110=DIRECTION('center_axis',(1.,0.,0.));
#16111=DIRECTION('ref_axis',(0.,0.,-1.));
#16112=DIRECTION('center_axis',(0.,1.,0.));
#16113=DIRECTION('ref_axis',(0.274625188963811,0.,-0.961551353587832));
#16114=DIRECTION('center_axis',(0.528132444354927,0.,-0.849162011173186));
#16115=DIRECTION('ref_axis',(-0.849162011173186,0.,-0.528132444354927));
#16116=DIRECTION('center_axis',(0.,1.,0.));
#16117=DIRECTION('ref_axis',(0.,0.,1.));
#16118=DIRECTION('center_axis',(-0.849162011173186,0.,0.528132444354927));
#16119=DIRECTION('ref_axis',(0.528132444354927,0.,0.849162011173186));
#16120=DIRECTION('center_axis',(0.,1.,0.));
#16121=DIRECTION('ref_axis',(0.,0.,1.));
#16122=DIRECTION('center_axis',(0.,1.,0.));
#16123=DIRECTION('ref_axis',(0.,0.,1.));
#16124=DIRECTION('center_axis',(-1.,0.,0.));
#16125=DIRECTION('ref_axis',(0.,0.,1.));
#16126=DIRECTION('center_axis',(0.,1.,0.));
#16127=DIRECTION('ref_axis',(0.453742606486508,0.,-0.891132788679011));
#16128=DIRECTION('center_axis',(0.,0.,1.));
#16129=DIRECTION('ref_axis',(1.,0.,0.));
#16130=DIRECTION('center_axis',(1.,0.,3.49148133884313E-15));
#16131=DIRECTION('ref_axis',(3.49148133884313E-15,0.,-1.));
#16132=DIRECTION('center_axis',(-1.,0.,0.));
#16133=DIRECTION('ref_axis',(0.,0.,1.));
#16134=DIRECTION('center_axis',(-4.53040918295421E-15,0.,1.));
#16135=DIRECTION('ref_axis',(1.,0.,4.53040918295421E-15));
#16136=DIRECTION('center_axis',(0.,1.,0.));
#16137=DIRECTION('ref_axis',(0.,0.,1.));
#16138=DIRECTION('center_axis',(0.849162011173186,1.46586199943601E-14,
0.528132444354927));
#16139=DIRECTION('ref_axis',(0.528132444354927,-1.61399174840201E-29,-0.849162011173186));
#16140=DIRECTION('center_axis',(0.,1.,0.));
#16141=DIRECTION('ref_axis',(0.,0.,1.));
#16142=DIRECTION('center_axis',(0.,1.,0.));
#16143=DIRECTION('ref_axis',(0.,0.,1.));
#16144=DIRECTION('center_axis',(1.,0.,0.));
#16145=DIRECTION('ref_axis',(0.,0.,-1.));
#16146=DIRECTION('center_axis',(0.,1.,0.));
#16147=DIRECTION('ref_axis',(0.45374260648651,0.,-0.891132788679009));
#16148=DIRECTION('center_axis',(0.,0.,-1.));
#16149=DIRECTION('ref_axis',(-1.,0.,0.));
#16150=DIRECTION('center_axis',(-1.,0.,-3.49148133884313E-15));
#16151=DIRECTION('ref_axis',(-3.49148133884313E-15,0.,1.));
#16152=DIRECTION('center_axis',(1.,0.,0.));
#16153=DIRECTION('ref_axis',(0.,0.,-1.));
#16154=DIRECTION('center_axis',(4.53040918295421E-15,0.,-1.));
#16155=DIRECTION('ref_axis',(-1.,0.,-4.53040918295421E-15));
#16156=DIRECTION('center_axis',(0.,1.,0.));
#16157=DIRECTION('ref_axis',(0.,0.,1.));
#16158=DIRECTION('center_axis',(-0.849162011173186,0.,-0.528132444354927));
#16159=DIRECTION('ref_axis',(-0.528132444354927,0.,0.849162011173186));
#16160=DIRECTION('center_axis',(0.,1.,0.));
#16161=DIRECTION('ref_axis',(0.,0.,1.));
#16162=DIRECTION('center_axis',(0.,1.,0.));
#16163=DIRECTION('ref_axis',(-0.453742606486517,0.,-0.891132788679006));
#16164=DIRECTION('center_axis',(0.,0.,1.));
#16165=DIRECTION('ref_axis',(1.,0.,0.));
#16166=DIRECTION('center_axis',(0.,1.,0.));
#16167=DIRECTION('ref_axis',(0.,0.,1.));
#16168=DIRECTION('center_axis',(1.,0.,0.));
#16169=DIRECTION('ref_axis',(0.,0.,-1.));
#16170=DIRECTION('center_axis',(0.,0.,-1.));
#16171=DIRECTION('ref_axis',(-1.,0.,0.));
#16172=DIRECTION('center_axis',(1.,0.,1.03892784411108E-15));
#16173=DIRECTION('ref_axis',(1.03892784411108E-15,0.,-1.));
#16174=DIRECTION('center_axis',(1.,0.,0.));
#16175=DIRECTION('ref_axis',(0.,0.,-1.));
#16176=DIRECTION('center_axis',(0.,1.,0.));
#16177=DIRECTION('ref_axis',(0.,0.,1.));
#16178=DIRECTION('center_axis',(-0.849162011173186,0.,0.528132444354927));
#16179=DIRECTION('ref_axis',(0.528132444354927,0.,0.849162011173186));
#16180=DIRECTION('center_axis',(0.,1.,0.));
#16181=DIRECTION('ref_axis',(0.,0.,1.));
#16182=DIRECTION('center_axis',(0.,1.,0.));
#16183=DIRECTION('ref_axis',(-0.45374260648651,0.,-0.891132788679009));
#16184=DIRECTION('center_axis',(0.,0.,-1.));
#16185=DIRECTION('ref_axis',(-1.,0.,0.));
#16186=DIRECTION('center_axis',(0.,1.,0.));
#16187=DIRECTION('ref_axis',(0.,0.,1.));
#16188=DIRECTION('center_axis',(-1.,0.,0.));
#16189=DIRECTION('ref_axis',(0.,0.,1.));
#16190=DIRECTION('center_axis',(0.,0.,1.));
#16191=DIRECTION('ref_axis',(1.,0.,0.));
#16192=DIRECTION('center_axis',(-1.,0.,-1.03892784411108E-15));
#16193=DIRECTION('ref_axis',(-1.03892784411108E-15,0.,1.));
#16194=DIRECTION('center_axis',(-1.,0.,0.));
#16195=DIRECTION('ref_axis',(0.,0.,1.));
#16196=DIRECTION('center_axis',(0.,1.,0.));
#16197=DIRECTION('ref_axis',(0.,0.,1.));
#16198=DIRECTION('center_axis',(0.849162011173186,0.,-0.528132444354927));
#16199=DIRECTION('ref_axis',(-0.528132444354927,0.,-0.849162011173186));
#16200=DIRECTION('center_axis',(0.,1.,0.));
#16201=DIRECTION('ref_axis',(0.,0.,1.));
#16202=DIRECTION('center_axis',(0.,1.,0.));
#16203=DIRECTION('ref_axis',(-0.0332934199937196,0.,-0.999445620424204));
#16204=DIRECTION('',(0.,1.,0.));
#16205=DIRECTION('',(0.,1.,0.));
#16206=DIRECTION('center_axis',(0.313163806483743,0.,-0.949699126201879));
#16207=DIRECTION('ref_axis',(-0.949699126201879,0.,-0.313163806483743));
#16208=DIRECTION('',(0.,-1.,0.));
#16209=DIRECTION('',(0.,1.,0.));
#16210=DIRECTION('center_axis',(0.313163806483743,0.,-0.949699126201879));
#16211=DIRECTION('ref_axis',(-0.949699126201879,0.,-0.313163806483743));
#16212=DIRECTION('',(0.,1.,0.));
#16213=DIRECTION('',(0.,1.,0.));
#16214=DIRECTION('',(-0.949699126201879,0.,-0.313163806483743));
#16215=DIRECTION('',(0.,-1.,0.));
#16216=DIRECTION('center_axis',(0.,1.,0.));
#16217=DIRECTION('ref_axis',(0.,0.,1.));
#16218=DIRECTION('center_axis',(0.,1.,0.));
#16219=DIRECTION('ref_axis',(0.,0.,1.));
#16220=DIRECTION('center_axis',(0.,1.,0.));
#16221=DIRECTION('ref_axis',(0.,0.,1.));
#16222=DIRECTION('center_axis',(0.,1.,0.));
#16223=DIRECTION('ref_axis',(0.,0.,1.));
#16224=DIRECTION('center_axis',(0.949699126201879,0.,0.313163806483743));
#16225=DIRECTION('ref_axis',(0.313163806483743,0.,-0.949699126201879));
#16226=DIRECTION('',(0.,-1.,0.));
#16227=DIRECTION('',(0.313163806483748,0.,-0.949699126201877));
#16228=DIRECTION('center_axis',(-0.949699126201879,0.,-0.313163806483743));
#16229=DIRECTION('ref_axis',(-0.313163806483743,0.,0.949699126201879));
#16230=DIRECTION('center_axis',(1.,0.,0.));
#16231=DIRECTION('ref_axis',(0.,0.,-1.));
#16232=DIRECTION('',(0.,-1.,0.));
#16233=DIRECTION('',(0.,-1.,0.));
#16234=DIRECTION('center_axis',(0.313163806483743,0.,-0.949699126201879));
#16235=DIRECTION('ref_axis',(-0.949699126201879,0.,-0.313163806483743));
#16236=DIRECTION('',(0.,-1.,0.));
#16237=DIRECTION('',(0.949699126201879,0.,0.313163806483743));
#16238=DIRECTION('center_axis',(0.,-1.,0.));
#16239=DIRECTION('ref_axis',(0.,0.,-1.));
#16240=DIRECTION('',(0.313163806483745,0.,-0.949699126201879));
#16241=DIRECTION('center_axis',(0.,0.,-1.));
#16242=DIRECTION('ref_axis',(-1.,0.,0.));
#16243=DIRECTION('',(0.,-1.,0.));
#16244=DIRECTION('center_axis',(-1.,0.,3.46944695195362E-15));
#16245=DIRECTION('ref_axis',(3.46944695195362E-15,0.,1.));
#16246=DIRECTION('',(0.,-1.,0.));
#16247=DIRECTION('center_axis',(-1.,0.,3.46944695195362E-15));
#16248=DIRECTION('ref_axis',(3.46944695195362E-15,0.,1.));
#16249=DIRECTION('',(0.,-1.,0.));
#16250=DIRECTION('center_axis',(0.,0.,-1.));
#16251=DIRECTION('ref_axis',(-1.,0.,0.));
#16252=DIRECTION('center_axis',(0.,0.,-1.));
#16253=DIRECTION('ref_axis',(-1.,0.,0.));
#16254=DIRECTION('center_axis',(0.,0.,-1.));
#16255=DIRECTION('ref_axis',(-1.,0.,0.));
#16256=DIRECTION('',(0.,-1.,0.));
#16257=DIRECTION('center_axis',(-1.,0.,3.46944695195362E-15));
#16258=DIRECTION('ref_axis',(3.46944695195362E-15,0.,1.));
#16259=DIRECTION('',(0.,-1.,0.));
#16260=DIRECTION('center_axis',(0.,0.,-1.));
#16261=DIRECTION('ref_axis',(-1.,0.,0.));
#16262=DIRECTION('',(0.,-1.,0.));
#16263=DIRECTION('center_axis',(0.,0.,-1.));
#16264=DIRECTION('ref_axis',(-1.,0.,0.));
#16265=DIRECTION('',(0.,-1.,0.));
#16266=DIRECTION('center_axis',(-1.,0.,3.46944695195362E-15));
#16267=DIRECTION('ref_axis',(3.46944695195362E-15,0.,1.));
#16268=DIRECTION('',(0.,-1.,0.));
#16269=DIRECTION('center_axis',(0.,0.,-1.));
#16270=DIRECTION('ref_axis',(-1.,0.,0.));
#16271=DIRECTION('',(0.,-1.,0.));
#16272=DIRECTION('center_axis',(-1.,0.,3.46944695195362E-15));
#16273=DIRECTION('ref_axis',(3.46944695195362E-15,0.,1.));
#16274=DIRECTION('center_axis',(-0.949699126201879,0.,-0.313163806483745));
#16275=DIRECTION('ref_axis',(-0.313163806483745,0.,0.949699126201879));
#16276=DIRECTION('axis',(0.,0.,1.));
#16277=DIRECTION('refdir',(1.,0.,0.));
#16278=DIRECTION('center_axis',(0.,-1.,0.));
#16279=DIRECTION('ref_axis',(0.,0.,-1.));
#16280=DIRECTION('center_axis',(0.,1.,0.));
#16281=DIRECTION('ref_axis',(0.,0.,1.));
#16282=DIRECTION('',(0.,1.,0.));
#16283=DIRECTION('center_axis',(0.,-1.,0.));
#16284=DIRECTION('ref_axis',(0.,0.,1.));
#16285=DIRECTION('center_axis',(0.,-1.,0.));
#16286=DIRECTION('ref_axis',(0.,0.,1.));
#16287=DIRECTION('center_axis',(0.,-1.,0.));
#16288=DIRECTION('ref_axis',(0.,0.,1.));
#16289=DIRECTION('center_axis',(0.,-1.,0.));
#16290=DIRECTION('ref_axis',(0.,0.,1.));
#16291=DIRECTION('center_axis',(0.,-1.,0.));
#16292=DIRECTION('ref_axis',(0.,0.,1.));
#16293=DIRECTION('center_axis',(0.,-1.,0.));
#16294=DIRECTION('ref_axis',(0.,0.,1.));
#16295=DIRECTION('center_axis',(0.,-1.,0.));
#16296=DIRECTION('ref_axis',(2.66453528935155E-15,0.,1.));
#16297=DIRECTION('center_axis',(0.,-1.,0.));
#16298=DIRECTION('ref_axis',(-9.76996260157579E-15,0.,1.));
#16299=DIRECTION('',(0.,1.,0.));
#16300=DIRECTION('center_axis',(0.,-1.,0.));
#16301=DIRECTION('ref_axis',(0.,0.,-1.));
#16302=DIRECTION('center_axis',(0.,-1.,0.));
#16303=DIRECTION('ref_axis',(1.,0.,0.));
#16304=DIRECTION('center_axis',(1.,0.,1.2246462853756E-16));
#16305=DIRECTION('ref_axis',(-1.2246462853756E-16,0.,1.));
#16306=DIRECTION('center_axis',(0.,1.,0.));
#16307=DIRECTION('ref_axis',(0.,0.,-1.));
#16308=DIRECTION('center_axis',(0.,1.,0.));
#16309=DIRECTION('ref_axis',(0.,0.,1.));
#16310=DIRECTION('center_axis',(0.,-1.,0.));
#16311=DIRECTION('ref_axis',(0.,0.,-1.));
#16312=DIRECTION('',(0.,1.,0.));
#16313=DIRECTION('center_axis',(0.,1.,0.));
#16314=DIRECTION('ref_axis',(0.,0.,-1.));
#16315=DIRECTION('center_axis',(0.,-1.,0.));
#16316=DIRECTION('ref_axis',(0.,0.,-1.));
#16317=DIRECTION('center_axis',(0.,-1.,0.));
#16318=DIRECTION('ref_axis',(0.,0.,-1.));
#16319=DIRECTION('center_axis',(1.,0.,1.22464658788737E-16));
#16320=DIRECTION('ref_axis',(-1.22464658788737E-16,0.,1.));
#16321=DIRECTION('center_axis',(0.,1.,0.));
#16322=DIRECTION('ref_axis',(0.,0.,-1.));
#16323=DIRECTION('center_axis',(0.,-1.,0.));
#16324=DIRECTION('ref_axis',(0.,0.,-1.));
#16325=DIRECTION('',(0.,-1.,0.));
#16326=DIRECTION('center_axis',(0.,-1.,0.));
#16327=DIRECTION('ref_axis',(0.,0.,-1.));
#16328=DIRECTION('center_axis',(0.,-1.,0.));
#16329=DIRECTION('ref_axis',(0.,0.,-1.));
#16330=DIRECTION('',(-0.100145321866555,0.991509942423395,-0.0829394271972054));
#16331=DIRECTION('center_axis',(0.,1.,0.));
#16332=DIRECTION('ref_axis',(0.,0.,1.));
#16333=DIRECTION('center_axis',(0.,1.,0.));
#16334=DIRECTION('ref_axis',(0.,0.,1.));
#16335=DIRECTION('center_axis',(-1.,0.,1.22464701140385E-16));
#16336=DIRECTION('ref_axis',(-1.22464701140385E-16,0.,-1.));
#16337=DIRECTION('center_axis',(0.,-1.,0.));
#16338=DIRECTION('ref_axis',(-9.76996260157579E-15,0.,1.));
#16339=DIRECTION('center_axis',(0.,-1.,0.));
#16340=DIRECTION('ref_axis',(0.,0.,-1.));
#16341=DIRECTION('',(0.126213886040806,0.99150994242542,0.0312744151347175));
#16342=DIRECTION('',(0.0542417484749782,0.99150994242342,0.118177268532842));
#16343=DIRECTION('',(-0.0585755320417947,0.991509942423397,0.116090228363862));
#16344=DIRECTION('',(-0.127284242208166,0.991509942423416,0.0265848784275387));
#16345=DIRECTION('',(0.00240506843293452,0.9915099424234,-0.130008652486594));
#16346=DIRECTION('',(0.103144393148005,0.991509942423398,-0.0791787107603998));
#16347=DIRECTION('center_axis',(0.,1.,0.));
#16348=DIRECTION('ref_axis',(0.,0.,1.));
#16349=DIRECTION('center_axis',(0.,1.,0.));
#16350=DIRECTION('ref_axis',(0.,0.,1.));
#16351=DIRECTION('center_axis',(0.,-1.,0.));
#16352=DIRECTION('ref_axis',(0.,0.,-1.));
#16353=DIRECTION('center_axis',(0.,-1.,0.));
#16354=DIRECTION('ref_axis',(0.,0.,-1.));
#16355=DIRECTION('center_axis',(0.,-1.,0.));
#16356=DIRECTION('ref_axis',(0.,0.,-1.));
#16357=DIRECTION('center_axis',(0.,-1.,0.));
#16358=DIRECTION('ref_axis',(0.,0.,-1.));
#16359=DIRECTION('center_axis',(0.,-1.,0.));
#16360=DIRECTION('ref_axis',(0.,0.,-1.));
#16361=DIRECTION('center_axis',(0.,-1.,0.));
#16362=DIRECTION('ref_axis',(0.109251264469497,0.,0.994014165498569));
#16363=DIRECTION('center_axis',(0.,-1.,0.));
#16364=DIRECTION('ref_axis',(0.,0.,-1.));
#16365=DIRECTION('center_axis',(0.,-1.,0.));
#16366=DIRECTION('ref_axis',(0.,0.,-1.));
#16367=DIRECTION('center_axis',(0.,-1.,0.));
#16368=DIRECTION('ref_axis',(0.,0.,-1.));
#16369=DIRECTION('',(0.,0.,1.));
#16370=DIRECTION('',(1.,0.,0.));
#16371=DIRECTION('',(0.718124297234771,0.,0.695914860971561));
#16372=DIRECTION('',(0.695914860971561,0.,-0.718124297234771));
#16373=CARTESIAN_POINT('',(0.,0.,0.));
#16374=CARTESIAN_POINT('',(0.,0.,0.));
#16375=CARTESIAN_POINT('Origin',(0.0835265683620477,-15.7044045823054,0.0824317919394229));
#16376=CARTESIAN_POINT('',(0.0835265683620474,-14.7669045823054,-2.10506820806058));
#16377=CARTESIAN_POINT('Origin',(0.0835265683620477,-14.7669045823054,0.0824317919394229));
#16378=CARTESIAN_POINT('',(0.0835265683620474,-14.4544045823054,-2.10506820806058));
#16379=CARTESIAN_POINT('',(0.0835265683620474,-15.7044045823054,-2.10506820806058));
#16380=CARTESIAN_POINT('Origin',(0.0835265683620477,-14.4544045823054,0.0824317919394229));
#16381=CARTESIAN_POINT('Origin',(0.0835265683620477,-22.3021228236204,0.0824317919394229));
#16382=CARTESIAN_POINT('',(0.0835265683620474,-11.3294045823054,-2.48006820806058));
#16383=CARTESIAN_POINT('Origin',(0.0835265683620477,-11.3294045823054,0.0824317919394229));
#16384=CARTESIAN_POINT('',(0.0835265683620474,-10.0794045823054,-2.48006820806058));
#16385=CARTESIAN_POINT('',(0.0835265683620474,-22.3021228236204,-2.48006820806058));
#16386=CARTESIAN_POINT('Origin',(0.0835265683620477,-10.0794045823054,0.0824317919394229));
#16387=CARTESIAN_POINT('Origin',(0.0835265683620477,-22.3021228236204,0.0824317919394229));
#16388=CARTESIAN_POINT('',(0.0835265683620473,-10.0794045823054,-3.35506820806058));
#16389=CARTESIAN_POINT('Origin',(0.0835265683620477,-10.0794045823054,0.0824317919394229));
#16390=CARTESIAN_POINT('',(0.0835265683620473,-12.5794045823054,-3.35506820806058));
#16391=CARTESIAN_POINT('',(0.0835265683620473,-22.3021228236204,-3.35506820806058));
#16392=CARTESIAN_POINT('Origin',(0.0835265683620477,-12.5794045823054,0.0824317919394229));
#16393=CARTESIAN_POINT('Origin',(0.0835265683620477,-17.1192738307565,0.0824317919394229));
#16394=CARTESIAN_POINT('',(0.0835265683620475,-14.4544045823054,-1.23006820806058));
#16395=CARTESIAN_POINT('Origin',(0.0835265683620477,-14.4544045823054,0.0824317919394229));
#16396=CARTESIAN_POINT('',(0.0835265683620475,-11.3294045823054,-1.23006820806058));
#16397=CARTESIAN_POINT('',(0.0835265683620475,-17.1192738307565,-1.23006820806058));
#16398=CARTESIAN_POINT('Origin',(0.0835265683620477,-11.3294045823054,0.0824317919394229));
#16399=CARTESIAN_POINT('Origin',(-44.291473431638,16.1705954176946,-44.2925682080606));
#16400=CARTESIAN_POINT('',(-44.291473431638,16.1705954176946,-41.4800682080606));
#16401=CARTESIAN_POINT('',(-44.291473431638,16.1705954176946,-47.1050682080606));
#16402=CARTESIAN_POINT('Origin',(-44.291473431638,16.1705954176946,-44.2925682080606));
#16403=CARTESIAN_POINT('Origin',(-44.291473431638,16.1705954176946,-44.2925682080606));
#16404=CARTESIAN_POINT('',(-44.291473431638,16.4830954176946,-47.4175682080606));
#16405=CARTESIAN_POINT('Origin',(-44.291473431638,16.1705954176946,-47.4175682080606));
#16406=CARTESIAN_POINT('Origin',(-44.291473431638,16.4830954176946,-44.2925682080606));
#16407=CARTESIAN_POINT('Origin',(-44.291473431638,-14.4544045823054,-44.2925682080606));
#16408=CARTESIAN_POINT('',(-44.291473431638,-14.7669045823054,-47.4175682080606));
#16409=CARTESIAN_POINT('Origin',(-44.291473431638,-14.7669045823054,-44.2925682080606));
#16410=CARTESIAN_POINT('',(-44.291473431638,-14.4544045823054,-47.1050682080606));
#16411=CARTESIAN_POINT('Origin',(-44.291473431638,-14.4544045823054,-47.4175682080606));
#16412=CARTESIAN_POINT('',(-44.291473431638,-14.4544045823054,-41.4800682080606));
#16413=CARTESIAN_POINT('Origin',(-44.291473431638,-14.4544045823054,-44.2925682080606));
#16414=CARTESIAN_POINT('Origin',(-44.291473431638,-14.4544045823054,-44.2925682080606));
#16415=CARTESIAN_POINT('Origin',(-44.291473431638,-8.87385981233827,-44.2925682080606));
#16416=CARTESIAN_POINT('',(-44.291473431638,-8.56135981233827,-41.1675682080606));
#16417=CARTESIAN_POINT('Origin',(-44.291473431638,-8.56135981233827,-44.2925682080606));
#16418=CARTESIAN_POINT('',(-44.291473431638,-8.87385981233827,-41.4800682080606));
#16419=CARTESIAN_POINT('Origin',(-44.291473431638,-8.87385981233827,-41.1675682080606));
#16420=CARTESIAN_POINT('Origin',(-44.291473431638,-8.87385981233827,-44.2925682080606));
#16421=CARTESIAN_POINT('Origin',(-44.291473431638,13.4386401876617,-44.2925682080606));
#16422=CARTESIAN_POINT('',(-44.291473431638,13.1261401876617,-47.4175682080606));
#16423=CARTESIAN_POINT('Origin',(-44.291473431638,13.1261401876617,-44.2925682080606));
#16424=CARTESIAN_POINT('',(-44.291473431638,13.4386401876617,-47.1050682080606));
#16425=CARTESIAN_POINT('Origin',(-44.291473431638,13.4386401876617,-47.4175682080606));
#16426=CARTESIAN_POINT('',(-44.291473431638,13.4386401876617,-41.4800682080606));
#16427=CARTESIAN_POINT('Origin',(-44.291473431638,13.4386401876617,-44.2925682080606));
#16428=CARTESIAN_POINT('Origin',(-44.291473431638,13.4386401876617,-44.2925682080606));
#16429=CARTESIAN_POINT('Origin',(-47.4164734316379,15.8580954176946,-29.4599768141645));
#16430=CARTESIAN_POINT('',(-48.0414734316379,15.5455954176946,-29.4599768141645));
#16431=CARTESIAN_POINT('',(-46.8857471746547,15.5455954176946,-29.1298940364426));
#16432=CARTESIAN_POINT('Origin',(-47.4164734316379,15.5455954176946,-29.4599768141645));
#16433=CARTESIAN_POINT('',(-48.3539734316379,15.8580954176946,-29.4599768141645));
#16434=CARTESIAN_POINT('Origin',(-48.0414734316379,15.8580954176946,-29.4599768141645));
#16435=CARTESIAN_POINT('',(-46.6203840461631,15.8580954176946,-28.9648526475817));
#16436=CARTESIAN_POINT('Origin',(-47.4164734316379,15.8580954176946,-29.4599768141645));
#16437=CARTESIAN_POINT('Origin',(-46.8857471746547,15.8580954176946,-29.1298940364426));
#16438=CARTESIAN_POINT('Origin',(-44.291473431638,15.8580954176946,-44.2925682080606));
#16439=CARTESIAN_POINT('',(-46.8650028434027,15.8580954176946,-40.7545502082785));
#16440=CARTESIAN_POINT('',(-40.7534554318559,15.8580954176946,-46.8660976198253));
#16441=CARTESIAN_POINT('Origin',(-44.291473431638,15.8580954176946,-44.2925682080606));
#16442=CARTESIAN_POINT('',(-47.0488263728144,15.5455954176946,-40.5018346368655));
#16443=CARTESIAN_POINT('Origin',(-47.0488263728144,15.8580954176946,-40.5018346368655));
#16444=CARTESIAN_POINT('',(-40.5007398604429,15.5455954176946,-47.049921149237));
#16445=CARTESIAN_POINT('Origin',(-44.291473431638,15.5455954176946,-44.2925682080606));
#16446=CARTESIAN_POINT('Origin',(-40.5007398604429,15.8580954176946,-47.049921149237));
#16447=CARTESIAN_POINT('Origin',(-47.4164734316379,16.1705954176946,-29.4599768141645));
#16448=CARTESIAN_POINT('',(-46.3550209176715,16.4830954176946,-28.7998112587208));
#16449=CARTESIAN_POINT('',(-48.6664734316379,16.4830954176946,-29.4599768141645));
#16450=CARTESIAN_POINT('Origin',(-47.4164734316379,16.4830954176946,-29.4599768141645));
#16451=CARTESIAN_POINT('',(-46.6203840461631,16.1705954176946,-28.9648526475817));
#16452=CARTESIAN_POINT('Origin',(-46.3550209176715,16.1705954176946,-28.7998112587208));
#16453=CARTESIAN_POINT('',(-48.3539734316379,16.1705954176946,-29.4599768141645));
#16454=CARTESIAN_POINT('Origin',(-47.4164734316379,16.1705954176946,-29.4599768141645));
#16455=CARTESIAN_POINT('Origin',(-48.6664734316379,16.1705954176946,-29.4599768141645));
#16456=CARTESIAN_POINT('Origin',(-44.291473431638,16.1705954176946,-44.2925682080606));
#16457=CARTESIAN_POINT('',(-40.7534554318559,16.1705954176946,-46.8660976198253));
#16458=CARTESIAN_POINT('',(-46.8650028434027,16.1705954176946,-40.7545502082785));
#16459=CARTESIAN_POINT('Origin',(-44.291473431638,16.1705954176946,-44.2925682080606));
#16460=CARTESIAN_POINT('',(-41.0061710032689,16.4830954176946,-46.6822740904135));
#16461=CARTESIAN_POINT('Origin',(-41.0061710032689,16.1705954176946,-46.6822740904135));
#16462=CARTESIAN_POINT('',(-46.6811793139909,16.4830954176946,-41.0072657796915));
#16463=CARTESIAN_POINT('Origin',(-44.291473431638,16.4830954176946,-44.2925682080606));
#16464=CARTESIAN_POINT('Origin',(-46.6811793139909,16.1705954176946,-41.0072657796915));
#16465=CARTESIAN_POINT('Origin',(44.4585265683622,16.1705954176946,-44.2925682080604));
#16466=CARTESIAN_POINT('',(41.6460265683622,16.1705954176946,-44.2925682080604));
#16467=CARTESIAN_POINT('',(44.4585265683622,16.1705954176946,-47.1050682080604));
#16468=CARTESIAN_POINT('Origin',(44.4585265683622,16.1705954176946,-44.2925682080604));
#16469=CARTESIAN_POINT('Origin',(44.4585265683622,16.1705954176946,-44.2925682080604));
#16470=CARTESIAN_POINT('',(44.4585265683622,16.4830954176946,-47.4175682080604));
#16471=CARTESIAN_POINT('Origin',(44.4585265683622,16.1705954176946,-47.4175682080604));
#16472=CARTESIAN_POINT('Origin',(44.4585265683622,16.4830954176946,-44.2925682080604));
#16473=CARTESIAN_POINT('Origin',(44.4585265683622,-14.4544045823054,-44.2925682080604));
#16474=CARTESIAN_POINT('',(44.4585265683622,-14.7669045823054,-47.4175682080604));
#16475=CARTESIAN_POINT('Origin',(44.4585265683622,-14.7669045823054,-44.2925682080604));
#16476=CARTESIAN_POINT('',(44.4585265683622,-14.4544045823054,-47.1050682080604));
#16477=CARTESIAN_POINT('Origin',(44.4585265683622,-14.4544045823054,-47.4175682080604));
#16478=CARTESIAN_POINT('',(41.6460265683622,-14.4544045823054,-44.2925682080604));
#16479=CARTESIAN_POINT('Origin',(44.4585265683622,-14.4544045823054,-44.2925682080604));
#16480=CARTESIAN_POINT('Origin',(44.4585265683622,-14.4544045823054,-44.2925682080604));
#16481=CARTESIAN_POINT('Origin',(44.4585265683622,-8.87385981233827,-44.2925682080604));
#16482=CARTESIAN_POINT('',(44.4585265683622,-8.56135981233827,-41.1675682080604));
#16483=CARTESIAN_POINT('Origin',(44.4585265683622,-8.56135981233827,-44.2925682080604));
#16484=CARTESIAN_POINT('',(44.4585265683622,-8.87385981233827,-41.4800682080604));
#16485=CARTESIAN_POINT('Origin',(44.4585265683622,-8.87385981233827,-41.1675682080604));
#16486=CARTESIAN_POINT('',(41.6460265683622,-8.87385981233827,-44.2925682080604));
#16487=CARTESIAN_POINT('Origin',(44.4585265683622,-8.87385981233827,-44.2925682080604));
#16488=CARTESIAN_POINT('Origin',(44.4585265683622,-8.87385981233827,-44.2925682080604));
#16489=CARTESIAN_POINT('Origin',(44.4585265683622,13.4386401876617,-44.2925682080604));
#16490=CARTESIAN_POINT('',(44.4585265683622,13.1261401876617,-47.4175682080604));
#16491=CARTESIAN_POINT('Origin',(44.4585265683622,13.1261401876617,-44.2925682080604));
#16492=CARTESIAN_POINT('',(44.4585265683622,13.4386401876617,-47.1050682080604));
#16493=CARTESIAN_POINT('Origin',(44.4585265683622,13.4386401876617,-47.4175682080604));
#16494=CARTESIAN_POINT('',(41.6460265683622,13.4386401876617,-44.2925682080604));
#16495=CARTESIAN_POINT('Origin',(44.4585265683622,13.4386401876617,-44.2925682080604));
#16496=CARTESIAN_POINT('Origin',(44.4585265683622,13.4386401876617,-44.2925682080604));
#16497=CARTESIAN_POINT('Origin',(47.5835265683621,15.8580954176946,-29.4599768141643));
#16498=CARTESIAN_POINT('',(47.0528003113789,15.5455954176946,-29.1298940364425));
#16499=CARTESIAN_POINT('',(48.2085265683621,15.5455954176946,-29.4599768141643));
#16500=CARTESIAN_POINT('Origin',(47.5835265683621,15.5455954176946,-29.4599768141643));
#16501=CARTESIAN_POINT('',(46.7874371828873,15.8580954176946,-28.9648526475816));
#16502=CARTESIAN_POINT('Origin',(47.0528003113789,15.8580954176946,-29.1298940364425));
#16503=CARTESIAN_POINT('',(48.5210265683621,15.8580954176946,-29.4599768141643));
#16504=CARTESIAN_POINT('Origin',(47.5835265683621,15.8580954176946,-29.4599768141643));
#16505=CARTESIAN_POINT('Origin',(48.2085265683621,15.8580954176946,-29.4599768141643));
#16506=CARTESIAN_POINT('Origin',(44.4585265683622,15.8580954176946,-44.2925682080604));
#16507=CARTESIAN_POINT('',(40.9205085685801,15.8580954176946,-46.8660976198251));
#16508=CARTESIAN_POINT('',(47.0320559801269,15.8580954176946,-40.7545502082783));
#16509=CARTESIAN_POINT('Origin',(44.4585265683622,15.8580954176946,-44.2925682080604));
#16510=CARTESIAN_POINT('',(40.6677929971671,15.5455954176946,-47.0499211492369));
#16511=CARTESIAN_POINT('Origin',(40.6677929971671,15.8580954176946,-47.0499211492369));
#16512=CARTESIAN_POINT('',(47.2158795095386,15.5455954176946,-40.5018346368653));
#16513=CARTESIAN_POINT('Origin',(44.4585265683622,15.5455954176946,-44.2925682080604));
#16514=CARTESIAN_POINT('Origin',(47.2158795095386,15.8580954176946,-40.5018346368653));
#16515=CARTESIAN_POINT('Origin',(47.5835265683621,16.1705954176946,-29.4599768141643));
#16516=CARTESIAN_POINT('',(48.8335265683621,16.4830954176946,-29.4599768141643));
#16517=CARTESIAN_POINT('',(46.5220740543957,16.4830954176946,-28.7998112587207));
#16518=CARTESIAN_POINT('Origin',(47.5835265683621,16.4830954176946,-29.4599768141643));
#16519=CARTESIAN_POINT('',(48.5210265683621,16.1705954176946,-29.4599768141643));
#16520=CARTESIAN_POINT('Origin',(48.8335265683621,16.1705954176946,-29.4599768141643));
#16521=CARTESIAN_POINT('',(46.7874371828873,16.1705954176946,-28.9648526475816));
#16522=CARTESIAN_POINT('Origin',(47.5835265683621,16.1705954176946,-29.4599768141643));
#16523=CARTESIAN_POINT('Origin',(46.5220740543957,16.1705954176946,-28.7998112587207));
#16524=CARTESIAN_POINT('Origin',(44.4585265683622,16.1705954176946,-44.2925682080604));
#16525=CARTESIAN_POINT('',(47.0320559801269,16.1705954176946,-40.7545502082783));
#16526=CARTESIAN_POINT('',(40.9205085685801,16.1705954176946,-46.8660976198251));
#16527=CARTESIAN_POINT('Origin',(44.4585265683622,16.1705954176946,-44.2925682080604));
#16528=CARTESIAN_POINT('',(46.8482324507151,16.4830954176946,-41.0072657796913));
#16529=CARTESIAN_POINT('Origin',(46.8482324507151,16.1705954176946,-41.0072657796913));
#16530=CARTESIAN_POINT('',(41.1732241399931,16.4830954176946,-46.6822740904134));
#16531=CARTESIAN_POINT('Origin',(44.4585265683622,16.4830954176946,-44.2925682080604));
#16532=CARTESIAN_POINT('Origin',(41.1732241399931,16.1705954176946,-46.6822740904134));
#16533=CARTESIAN_POINT('Origin',(44.4585265683621,16.1705954176946,44.4574317919394));
#16534=CARTESIAN_POINT('',(44.4585265683621,16.1705954176946,41.6449317919394));
#16535=CARTESIAN_POINT('Origin',(44.4585265683621,16.1705954176946,44.4574317919394));
#16536=CARTESIAN_POINT('',(44.4585265683621,16.4830954176946,41.3324317919394));
#16537=CARTESIAN_POINT('Origin',(44.4585265683621,16.1705954176946,41.3324317919394));
#16538=CARTESIAN_POINT('Origin',(44.4585265683621,16.4830954176946,44.4574317919394));
#16539=CARTESIAN_POINT('Origin',(44.4585265683621,-14.4544045823054,44.4574317919394));
#16540=CARTESIAN_POINT('',(44.4585265683621,-14.7669045823054,41.3324317919394));
#16541=CARTESIAN_POINT('Origin',(44.4585265683621,-14.7669045823054,44.4574317919394));
#16542=CARTESIAN_POINT('',(44.4585265683621,-14.4544045823054,41.6449317919394));
#16543=CARTESIAN_POINT('Origin',(44.4585265683621,-14.4544045823054,41.3324317919394));
#16544=CARTESIAN_POINT('Origin',(44.4585265683621,-14.4544045823054,44.4574317919394));
#16545=CARTESIAN_POINT('Origin',(44.4585265683621,-8.87385981233827,44.4574317919394));
#16546=CARTESIAN_POINT('',(44.4585265683621,-8.56135981233827,47.5824317919394));
#16547=CARTESIAN_POINT('Origin',(44.4585265683621,-8.56135981233827,44.4574317919394));
#16548=CARTESIAN_POINT('',(44.4585265683621,-8.87385981233827,47.2699317919394));
#16549=CARTESIAN_POINT('Origin',(44.4585265683621,-8.87385981233827,47.5824317919394));
#16550=CARTESIAN_POINT('',(44.4585265683621,-8.87385981233827,41.6449317919394));
#16551=CARTESIAN_POINT('Origin',(44.4585265683621,-8.87385981233827,44.4574317919394));
#16552=CARTESIAN_POINT('Origin',(44.4585265683621,-8.87385981233827,44.4574317919394));
#16553=CARTESIAN_POINT('Origin',(44.4585265683621,13.4386401876617,44.4574317919394));
#16554=CARTESIAN_POINT('',(44.4585265683621,13.1261401876617,41.3324317919394));
#16555=CARTESIAN_POINT('Origin',(44.4585265683621,13.1261401876617,44.4574317919394));
#16556=CARTESIAN_POINT('',(44.4585265683621,13.4386401876617,41.6449317919394));
#16557=CARTESIAN_POINT('Origin',(44.4585265683621,13.4386401876617,41.3324317919394));
#16558=CARTESIAN_POINT('Origin',(44.4585265683621,13.4386401876617,44.4574317919394));
#16559=CARTESIAN_POINT('Origin',(47.583526568362,15.8580954176946,40.1612670779183));
#16560=CARTESIAN_POINT('',(47.2158795095385,15.5455954176946,40.6666982207443));
#16561=CARTESIAN_POINT('',(48.2085265683621,15.5455954176946,40.1612670779183));
#16562=CARTESIAN_POINT('Origin',(47.583526568362,15.5455954176946,40.1612670779183));
#16563=CARTESIAN_POINT('',(47.0320559801268,15.8580954176946,40.9194137921573));
#16564=CARTESIAN_POINT('Origin',(47.2158795095385,15.8580954176946,40.6666982207443));
#16565=CARTESIAN_POINT('',(48.5210265683621,15.8580954176946,40.1612670779183));
#16566=CARTESIAN_POINT('Origin',(47.583526568362,15.8580954176946,40.1612670779183));
#16567=CARTESIAN_POINT('Origin',(48.2085265683621,15.8580954176946,40.1612670779183));
#16568=CARTESIAN_POINT('Origin',(47.583526568362,16.1705954176946,40.1612670779183));
#16569=CARTESIAN_POINT('',(48.8335265683621,16.4830954176946,40.1612670779183));
#16570=CARTESIAN_POINT('',(46.848232450715,16.4830954176946,41.1721293635703));
#16571=CARTESIAN_POINT('Origin',(47.583526568362,16.4830954176946,40.1612670779183));
#16572=CARTESIAN_POINT('',(48.5210265683621,16.1705954176946,40.1612670779183));
#16573=CARTESIAN_POINT('Origin',(48.8335265683621,16.1705954176946,40.1612670779183));
#16574=CARTESIAN_POINT('',(47.0320559801268,16.1705954176946,40.9194137921573));
#16575=CARTESIAN_POINT('Origin',(47.583526568362,16.1705954176946,40.1612670779183));
#16576=CARTESIAN_POINT('Origin',(46.848232450715,16.1705954176946,41.1721293635703));
#16577=CARTESIAN_POINT('Origin',(-44.2914734316384,16.1705954176946,44.457431791939));
#16578=CARTESIAN_POINT('',(-44.2914734316384,16.1705954176946,41.644931791939));
#16579=CARTESIAN_POINT('',(-41.4789734316384,16.1705954176946,44.457431791939));
#16580=CARTESIAN_POINT('Origin',(-44.2914734316384,16.1705954176946,44.457431791939));
#16581=CARTESIAN_POINT('',(-44.2914734316384,16.4830954176946,41.332431791939));
#16582=CARTESIAN_POINT('Origin',(-44.2914734316384,16.1705954176946,41.332431791939));
#16583=CARTESIAN_POINT('Origin',(-44.2914734316384,16.4830954176946,44.457431791939));
#16584=CARTESIAN_POINT('Origin',(-44.2914734316384,16.1705954176946,44.457431791939));
#16585=CARTESIAN_POINT('Origin',(-44.2914734316384,-14.4544045823054,44.457431791939));
#16586=CARTESIAN_POINT('',(-44.2914734316384,-14.7669045823054,41.332431791939));
#16587=CARTESIAN_POINT('Origin',(-44.2914734316384,-14.7669045823054,44.457431791939));
#16588=CARTESIAN_POINT('',(-44.2914734316384,-14.4544045823054,41.644931791939));
#16589=CARTESIAN_POINT('Origin',(-44.2914734316384,-14.4544045823054,41.332431791939));
#16590=CARTESIAN_POINT('',(-41.4789734316384,-14.4544045823054,44.457431791939));
#16591=CARTESIAN_POINT('Origin',(-44.2914734316384,-14.4544045823054,44.457431791939));
#16592=CARTESIAN_POINT('Origin',(-44.2914734316384,-14.4544045823054,44.457431791939));
#16593=CARTESIAN_POINT('Origin',(-44.2914734316384,-8.87385981233827,44.457431791939));
#16594=CARTESIAN_POINT('',(-44.2914734316384,-8.56135981233827,47.582431791939));
#16595=CARTESIAN_POINT('Origin',(-44.2914734316384,-8.56135981233827,44.457431791939));
#16596=CARTESIAN_POINT('',(-44.2914734316384,-8.87385981233827,47.269931791939));
#16597=CARTESIAN_POINT('Origin',(-44.2914734316384,-8.87385981233827,47.582431791939));
#16598=CARTESIAN_POINT('',(-41.4789734316384,-8.87385981233827,44.457431791939));
#16599=CARTESIAN_POINT('Origin',(-44.2914734316384,-8.87385981233827,44.457431791939));
#16600=CARTESIAN_POINT('Origin',(-44.2914734316384,-8.87385981233827,44.457431791939));
#16601=CARTESIAN_POINT('Origin',(-44.2914734316384,13.4386401876617,44.457431791939));
#16602=CARTESIAN_POINT('',(-44.2914734316384,13.1261401876617,41.332431791939));
#16603=CARTESIAN_POINT('Origin',(-44.2914734316384,13.1261401876617,44.457431791939));
#16604=CARTESIAN_POINT('',(-44.2914734316384,13.4386401876617,41.644931791939));
#16605=CARTESIAN_POINT('Origin',(-44.2914734316384,13.4386401876617,41.332431791939));
#16606=CARTESIAN_POINT('',(-41.4789734316384,13.4386401876617,44.457431791939));
#16607=CARTESIAN_POINT('Origin',(-44.2914734316384,13.4386401876617,44.457431791939));
#16608=CARTESIAN_POINT('Origin',(-44.2914734316384,13.4386401876617,44.457431791939));
#16609=CARTESIAN_POINT('Origin',(0.0835265683620477,-3.61941807409668,0.0824317919394229));
#16610=CARTESIAN_POINT('',(-34.1615012109487,-3.61941807409668,36.0841779807597));
#16611=CARTESIAN_POINT('',(34.3285543476724,-3.61941807409668,36.0841779807601));
#16612=CARTESIAN_POINT('Origin',(0.0835265683620477,-3.61941807409668,0.0824317919394229));
#16613=CARTESIAN_POINT('',(-34.2245838299087,-3.84038894321748,36.1504966431758));
#16614=CARTESIAN_POINT('Origin',(-34.3768787441519,-3.61941807409668,36.310604057419));
#16615=CARTESIAN_POINT('',(34.3916369666324,-3.84038894321748,36.1504966431761));
#16616=CARTESIAN_POINT('Origin',(0.0835265683620477,-3.84038894321747,0.0824317919394229));
#16617=CARTESIAN_POINT('Origin',(34.5439318808756,-3.61941807409668,36.3106040574193));
#16618=CARTESIAN_POINT('Origin',(0.0835265683620477,11.9341984494201,0.0824317919394229));
#16619=CARTESIAN_POINT('',(-34.2245838299085,12.155169318541,36.1504966431761));
#16620=CARTESIAN_POINT('',(34.3916369666327,12.1551693185413,36.1504966431763));
#16621=CARTESIAN_POINT('Origin',(0.0835265683620477,12.1551693185409,0.0824317919394229));
#16622=CARTESIAN_POINT('',(-34.1615012109487,11.9341984494201,36.0841779807597));
#16623=CARTESIAN_POINT('Origin',(-34.3768787441519,11.9341984494201,36.310604057419));
#16624=CARTESIAN_POINT('',(34.3285543476724,11.9341984494201,36.0841779807601));
#16625=CARTESIAN_POINT('Origin',(0.0835265683620477,11.9341984494201,0.0824317919394229));
#16626=CARTESIAN_POINT('Origin',(34.5439318808756,11.9341984494201,36.3106040574193));
#16627=CARTESIAN_POINT('Origin',(-39.6912298733817,12.8136401876617,39.8571882336823));
#16628=CARTESIAN_POINT('',(-40.5751133498648,13.1261401876617,38.9733047571991));
#16629=CARTESIAN_POINT('',(-38.8073463968985,13.1261401876617,40.7410717101655));
#16630=CARTESIAN_POINT('Origin',(-39.6912298733817,13.1261401876617,39.8571882336823));
#16631=CARTESIAN_POINT('',(-40.354142480744,12.8136401876617,39.1942756263199));
#16632=CARTESIAN_POINT('Origin',(-40.5751133498648,12.8136401876617,38.9733047571991));
#16633=CARTESIAN_POINT('',(-39.0283172660193,12.8136401876617,40.5201008410447));
#16634=CARTESIAN_POINT('Origin',(-39.6912298733817,12.8136401876617,39.8571882336823));
#16635=CARTESIAN_POINT('Origin',(-38.8073463968985,12.8136401876617,40.7410717101655));
#16636=CARTESIAN_POINT('Origin',(39.8582830101054,12.8136401876617,39.8571882336827));
#16637=CARTESIAN_POINT('',(38.9743995336222,13.1261401876617,40.7410717101659));
#16638=CARTESIAN_POINT('',(40.7421664865885,13.1261401876617,38.9733047571995));
#16639=CARTESIAN_POINT('Origin',(39.8582830101054,13.1261401876617,39.8571882336827));
#16640=CARTESIAN_POINT('',(39.195370402743,12.8136401876617,40.5201008410451));
#16641=CARTESIAN_POINT('Origin',(38.9743995336222,12.8136401876617,40.7410717101659));
#16642=CARTESIAN_POINT('',(40.5211956174677,12.8136401876617,39.1942756263203));
#16643=CARTESIAN_POINT('Origin',(39.8582830101054,12.8136401876617,39.8571882336827));
#16644=CARTESIAN_POINT('Origin',(40.7421664865885,12.8136401876617,38.9733047571995));
#16645=CARTESIAN_POINT('Origin',(-39.6912298733813,-8.24885981233827,-39.6923246498039));
#16646=CARTESIAN_POINT('',(-40.5751133498644,-8.56135981233827,-38.8084411733207));
#16647=CARTESIAN_POINT('',(-38.8073463968981,-8.56135981233827,-40.576208126287));
#16648=CARTESIAN_POINT('Origin',(-39.6912298733813,-8.56135981233827,-39.6923246498039));
#16649=CARTESIAN_POINT('',(-40.3541424807436,-8.24885981233828,-39.0294120424415));
#16650=CARTESIAN_POINT('Origin',(-40.5751133498644,-8.24885981233827,-38.8084411733207));
#16651=CARTESIAN_POINT('',(-39.0283172660189,-8.24885981233828,-40.3552372571663));
#16652=CARTESIAN_POINT('Origin',(-39.6912298733813,-8.24885981233827,-39.6923246498039));
#16653=CARTESIAN_POINT('Origin',(-38.8073463968981,-8.24885981233827,-40.576208126287));
#16654=CARTESIAN_POINT('Origin',(39.8582830101055,-8.24885981233827,-39.6923246498037));
#16655=CARTESIAN_POINT('',(38.9743995336223,-8.56135981233827,-40.5762081262869));
#16656=CARTESIAN_POINT('',(40.7421664865887,-8.56135981233827,-38.8084411733206));
#16657=CARTESIAN_POINT('Origin',(39.8582830101055,-8.56135981233827,-39.6923246498037));
#16658=CARTESIAN_POINT('',(39.1953704027431,-8.24885981233828,-40.3552372571661));
#16659=CARTESIAN_POINT('Origin',(38.9743995336223,-8.24885981233827,-40.5762081262869));
#16660=CARTESIAN_POINT('',(40.5211956174679,-8.24885981233828,-39.0294120424414));
#16661=CARTESIAN_POINT('Origin',(39.8582830101055,-8.24885981233827,-39.6923246498037));
#16662=CARTESIAN_POINT('Origin',(40.7421664865887,-8.24885981233827,-38.8084411733206));
#16663=CARTESIAN_POINT('Origin',(-34.3768787441515,11.4830954176946,-36.1457404735405));
#16664=CARTESIAN_POINT('',(-34.5978496132723,-3.61941807409669,-35.9247696044197));
#16665=CARTESIAN_POINT('',(-34.1615012109483,-3.61941807409668,-35.9193143968812));
#16666=CARTESIAN_POINT('Origin',(-34.3768787441515,-3.61941807409669,-36.1457404735405));
#16667=CARTESIAN_POINT('',(-34.5978496132723,11.9341984494202,-35.9247696044197));
#16668=CARTESIAN_POINT('',(-34.5978496132723,-3.74885981233827,-35.9247696044197));
#16669=CARTESIAN_POINT('',(-34.1615012109483,11.9341984494201,-35.9193143968812));
#16670=CARTESIAN_POINT('Origin',(-34.3768787441515,11.9341984494201,-36.1457404735405));
#16671=CARTESIAN_POINT('',(-34.1615012109483,11.4830954176946,-35.9193143968812));
#16672=CARTESIAN_POINT('Origin',(34.5439318808757,11.4830954176946,-36.1457404735404));
#16673=CARTESIAN_POINT('',(34.3285543476725,-3.61941807409668,-35.9193143968811));
#16674=CARTESIAN_POINT('',(34.7649027499965,-3.61941807409669,-35.9247696044196));
#16675=CARTESIAN_POINT('Origin',(34.5439318808757,-3.61941807409668,-36.1457404735404));
#16676=CARTESIAN_POINT('',(34.3285543476725,11.9341984494201,-35.9193143968811));
#16677=CARTESIAN_POINT('',(34.3285543476725,11.4830954176946,-35.9193143968811));
#16678=CARTESIAN_POINT('',(34.7649027499969,11.9341984494207,-35.92476960442));
#16679=CARTESIAN_POINT('Origin',(34.5439318808757,11.9341984494202,-36.1457404735404));
#16680=CARTESIAN_POINT('',(34.7649027499965,12.0636401876617,-35.9247696044196));
#16681=CARTESIAN_POINT('Origin',(-19.6585232829181,-11.0169045823054,10.2084687225244));
#16682=CARTESIAN_POINT('',(-19.3804662427592,-11.3294045823054,10.0658484840654));
#16683=CARTESIAN_POINT('',(-19.9553042598562,-11.3294045823054,10.1106050329982));
#16684=CARTESIAN_POINT('Origin',(-19.6585232829181,-11.3294045823054,10.2084687225244));
#16685=CARTESIAN_POINT('',(-19.9553042598562,-14.4544045823054,10.1106050329982));
#16686=CARTESIAN_POINT('',(-19.9553042598562,-11.0169045823054,10.1106050329982));
#16687=CARTESIAN_POINT('',(-19.3804662427592,-14.4544045823054,10.0658484840654));
#16688=CARTESIAN_POINT('Origin',(-19.6585232829181,-14.4544045823054,10.2084687225244));
#16689=CARTESIAN_POINT('',(-19.3804662427592,-11.0169045823054,10.0658484840654));
#16690=CARTESIAN_POINT('Origin',(-19.6585232829181,-11.3294045823054,10.2084687225244));
#16691=CARTESIAN_POINT('',(-19.1024092026003,-11.0169045823054,9.9232282456065));
#16692=CARTESIAN_POINT('Origin',(-19.1024092026003,-11.3294045823054,9.9232282456065));
#16693=CARTESIAN_POINT('',(-20.2520852367942,-11.0169045823054,10.012741343472));
#16694=CARTESIAN_POINT('Origin',(-19.6585232829181,-11.0169045823054,10.2084687225244));
#16695=CARTESIAN_POINT('Origin',(-20.2520852367942,-11.3294045823054,10.012741343472));
#16696=CARTESIAN_POINT('Origin',(-35.8042963200226,-14.7669045823054,33.0767747666364));
#16697=CARTESIAN_POINT('',(-36.1010780564215,-7.07885853810828,32.9789133801876));
#16698=CARTESIAN_POINT('',(-35.5742461733022,-7.07886995352308,32.8652725680806));
#16699=CARTESIAN_POINT('Origin',(-35.8042963200226,-7.07886995352308,33.0767747666364));
#16700=CARTESIAN_POINT('',(-35.5742461733022,-12.8919045823054,32.8652725680806));
#16701=CARTESIAN_POINT('',(-35.5742461733022,-14.7669045823054,32.8652725680806));
#16702=CARTESIAN_POINT('',(-36.1010772969607,-12.8919045823054,32.9789110771102));
#16703=CARTESIAN_POINT('Origin',(-35.8042963200226,-12.8919045823054,33.0767747666364));
#16704=CARTESIAN_POINT('',(-36.1010772969607,16.4855954176946,32.9789110771102));
#16705=CARTESIAN_POINT('Origin',(-38.2816342705276,-14.7669045823054,-28.971484618867));
#16706=CARTESIAN_POINT('',(-38.5307586915594,-11.3294045823054,-29.1601464137424));
#16707=CARTESIAN_POINT('',(-38.1837705810015,-11.3294045823054,-29.2682655958051));
#16708=CARTESIAN_POINT('Origin',(-38.2816342705276,-11.3294045823054,-28.971484618867));
#16709=CARTESIAN_POINT('',(-38.5307586915594,-12.8919045823054,-29.1601464137424));
#16710=CARTESIAN_POINT('',(-38.5307586915594,-14.7669045823054,-29.1601464137424));
#16711=CARTESIAN_POINT('',(-38.1837705810015,-12.8919045823054,-29.2682655958051));
#16712=CARTESIAN_POINT('Origin',(-38.2816342705276,-12.8919045823054,-28.971484618867));
#16713=CARTESIAN_POINT('',(-38.1837705810015,-11.0169045823054,-29.2682655958051));
#16714=CARTESIAN_POINT('Origin',(40.0376426042469,-14.7669045823054,28.0150491378139));
#16715=CARTESIAN_POINT('',(39.7815264758118,-6.59535043767467,27.8359938984173));
#16716=CARTESIAN_POINT('',(40.1355064102017,-6.5953500105935,27.7182681992682));
#16717=CARTESIAN_POINT('Origin',(40.0376426042469,-6.59535043767467,28.0150491378139));
#16718=CARTESIAN_POINT('',(40.1355062937731,-12.8919045823054,27.7182681608758));
#16719=CARTESIAN_POINT('',(40.1355062937731,-6.01690458230549,27.7182681608758));
#16720=CARTESIAN_POINT('',(39.7815264758118,-12.8919045823054,27.8359938984173));
#16721=CARTESIAN_POINT('Origin',(40.0376426042469,-12.8919045823054,28.0150491378139));
#16722=CARTESIAN_POINT('',(39.7815264758118,-14.7669045823054,27.8359938984173));
#16723=CARTESIAN_POINT('Origin',(34.5286855795389,-14.7669045823054,-33.5262969209224));
#16724=CARTESIAN_POINT('',(34.2319046026008,-11.3294045823054,-33.6241606104486));
#16725=CARTESIAN_POINT('',(34.7523554432479,-11.3294045823054,-33.7445354190578));
#16726=CARTESIAN_POINT('Origin',(34.5286855795389,-11.3294045823054,-33.5262969209224));
#16727=CARTESIAN_POINT('',(34.2319046026008,-12.8919045823054,-33.6241606104486));
#16728=CARTESIAN_POINT('',(34.2319046026008,-11.0169045823054,-33.6241606104486));
#16729=CARTESIAN_POINT('',(34.7523554432479,-12.8919045823054,-33.7445354190578));
#16730=CARTESIAN_POINT('Origin',(34.5286855795389,-12.8919045823054,-33.5262969209224));
#16731=CARTESIAN_POINT('',(34.7523554432479,-14.7669045823054,-33.7445354190578));
#16732=CARTESIAN_POINT('Origin',(19.8255764196421,-14.4544045823054,-10.0436051386457));
#16733=CARTESIAN_POINT('',(20.1223573965802,-14.4544045823054,-9.94574144911951));
#16734=CARTESIAN_POINT('',(19.5475193794832,-14.4544045823054,-9.90098490018674));
#16735=CARTESIAN_POINT('Origin',(19.8255764196421,-14.4544045823054,-10.0436051386457));
#16736=CARTESIAN_POINT('',(20.4191383735183,-14.7669045823054,-9.84787775959334));
#16737=CARTESIAN_POINT('Origin',(20.4191383735183,-14.4544045823054,-9.84787775959334));
#16738=CARTESIAN_POINT('',(19.2694623393243,-14.7669045823054,-9.75836466172779));
#16739=CARTESIAN_POINT('Origin',(19.8255764196421,-14.7669045823054,-10.0436051386457));
#16740=CARTESIAN_POINT('Origin',(19.2694623393243,-14.4544045823054,-9.75836466172779));
#16741=CARTESIAN_POINT('Origin',(-47.4164734316384,15.8580954176946,40.1612670779178));
#16742=CARTESIAN_POINT('',(-48.0414734316384,15.5455954176946,40.1612670779178));
#16743=CARTESIAN_POINT('',(-47.0488263728148,15.5455954176946,40.6666982207438));
#16744=CARTESIAN_POINT('Origin',(-47.4164734316384,15.5455954176946,40.1612670779178));
#16745=CARTESIAN_POINT('',(-48.3539734316384,15.8580954176946,40.1612670779178));
#16746=CARTESIAN_POINT('Origin',(-48.0414734316384,15.8580954176946,40.1612670779178));
#16747=CARTESIAN_POINT('',(-46.8650028434031,15.8580954176946,40.9194137921568));
#16748=CARTESIAN_POINT('Origin',(-47.4164734316384,15.8580954176946,40.1612670779178));
#16749=CARTESIAN_POINT('Origin',(-47.0488263728148,15.8580954176946,40.6666982207438));
#16750=CARTESIAN_POINT('Origin',(-47.4164734316384,16.1705954176946,40.1612670779178));
#16751=CARTESIAN_POINT('',(-46.6811793139913,16.4830954176946,41.1721293635699));
#16752=CARTESIAN_POINT('',(-48.6664734316384,16.4830954176946,40.1612670779178));
#16753=CARTESIAN_POINT('Origin',(-47.4164734316384,16.4830954176946,40.1612670779178));
#16754=CARTESIAN_POINT('',(-46.8650028434031,16.1705954176946,40.9194137921568));
#16755=CARTESIAN_POINT('Origin',(-46.6811793139913,16.1705954176946,41.1721293635698));
#16756=CARTESIAN_POINT('',(-48.3539734316384,16.1705954176946,40.1612670779178));
#16757=CARTESIAN_POINT('Origin',(-47.4164734316384,16.1705954176946,40.1612670779178));
#16758=CARTESIAN_POINT('Origin',(-48.6664734316384,16.1705954176946,40.1612670779178));
#16759=CARTESIAN_POINT('Origin',(-29.4588820377423,15.5455954176946,47.5824317919391));
#16760=CARTESIAN_POINT('',(-28.9637578711596,15.8580954176946,46.7863424064643));
#16761=CARTESIAN_POINT('',(-29.4588820377423,15.8580954176946,48.5199317919391));
#16762=CARTESIAN_POINT('Origin',(-29.4588820377423,15.8580954176946,47.5824317919391));
#16763=CARTESIAN_POINT('',(-29.4588820377423,16.1705954176946,48.5199317919391));
#16764=CARTESIAN_POINT('',(-29.4588820377423,15.5455954176946,48.5199317919391));
#16765=CARTESIAN_POINT('',(-28.9637578711596,16.1705954176946,46.7863424064643));
#16766=CARTESIAN_POINT('Origin',(-29.4588820377423,16.1705954176946,47.5824317919391));
#16767=CARTESIAN_POINT('',(-28.9637578711596,15.5455954176946,46.7863424064643));
#16768=CARTESIAN_POINT('Origin',(-44.2914734316384,15.5455954176946,44.457431791939));
#16769=CARTESIAN_POINT('',(-40.7534554318564,15.8580954176946,47.0309612037037));
#16770=CARTESIAN_POINT('Origin',(-44.2914734316384,15.8580954176946,44.457431791939));
#16771=CARTESIAN_POINT('',(-46.8650028434031,15.5455954176946,40.9194137921568));
#16772=CARTESIAN_POINT('',(-40.7534554318564,16.1705954176946,47.0309612037037));
#16773=CARTESIAN_POINT('Origin',(-44.2914734316384,16.1705954176946,44.457431791939));
#16774=CARTESIAN_POINT('',(-40.7534554318564,15.5455954176946,47.0309612037037));
#16775=CARTESIAN_POINT('Origin',(-44.2914734316384,16.4830954176946,44.457431791939));
#16776=CARTESIAN_POINT('',(-41.4789734316384,16.4830954176946,44.457431791939));
#16777=CARTESIAN_POINT('Origin',(-44.2914734316384,16.4830954176946,44.457431791939));
#16778=CARTESIAN_POINT('',(-41.4789734316384,16.4830954176946,44.457431791939));
#16779=CARTESIAN_POINT('Origin',(-39.6912298733817,13.1261401876617,39.8571882336823));
#16780=CARTESIAN_POINT('',(-40.354142480744,-8.24885981233828,39.1942756263199));
#16781=CARTESIAN_POINT('',(-40.354142480744,16.4855954176946,39.1942756263199));
#16782=CARTESIAN_POINT('',(-39.0283172660193,-8.24885981233828,40.5201008410447));
#16783=CARTESIAN_POINT('Origin',(-39.6912298733817,-8.24885981233827,39.8571882336823));
#16784=CARTESIAN_POINT('',(-39.0283172660193,16.4855954176946,40.5201008410447));
#16785=CARTESIAN_POINT('Origin',(47.583526568362,15.5455954176946,29.6248403980433));
#16786=CARTESIAN_POINT('',(46.7874371828872,15.8580954176946,29.1297162314606));
#16787=CARTESIAN_POINT('',(48.5210265683621,15.8580954176946,29.6248403980433));
#16788=CARTESIAN_POINT('Origin',(47.583526568362,15.8580954176946,29.6248403980433));
#16789=CARTESIAN_POINT('',(48.5210265683621,16.1705954176946,29.6248403980433));
#16790=CARTESIAN_POINT('',(48.5210265683621,15.5455954176946,29.6248403980433));
#16791=CARTESIAN_POINT('',(46.7874371828872,16.1705954176946,29.1297162314606));
#16792=CARTESIAN_POINT('Origin',(47.583526568362,16.1705954176946,29.6248403980433));
#16793=CARTESIAN_POINT('',(46.7874371828872,15.5455954176946,29.1297162314606));
#16794=CARTESIAN_POINT('Origin',(44.4585265683621,15.5455954176946,44.4574317919394));
#16795=CARTESIAN_POINT('',(40.92050856858,15.8580954176946,47.0309612037041));
#16796=CARTESIAN_POINT('Origin',(44.4585265683621,15.8580954176946,44.4574317919394));
#16797=CARTESIAN_POINT('',(40.92050856858,16.1705954176946,47.0309612037041));
#16798=CARTESIAN_POINT('',(40.92050856858,15.5455954176946,47.0309612037041));
#16799=CARTESIAN_POINT('Origin',(44.4585265683621,16.1705954176946,44.4574317919394));
#16800=CARTESIAN_POINT('',(47.0320559801268,15.5455954176946,40.9194137921573));
#16801=CARTESIAN_POINT('Origin',(44.4585265683621,16.4830954176946,44.4574317919394));
#16802=CARTESIAN_POINT('',(44.4585265683621,16.4830954176946,41.6449317919394));
#16803=CARTESIAN_POINT('Origin',(44.4585265683621,16.4830954176946,44.4574317919394));
#16804=CARTESIAN_POINT('',(44.4585265683621,16.4830954176946,41.6449317919394));
#16805=CARTESIAN_POINT('Origin',(0.0835265683620477,-8.56135981233827,0.0824317919394229));
#16806=CARTESIAN_POINT('',(-37.498691208412,-8.46983068145907,39.4252660733572));
#16807=CARTESIAN_POINT('Ctrl Pts',(-34.2245838299087,-3.84038894321748,
36.1504966431758));
#16808=CARTESIAN_POINT('Ctrl Pts',(-34.3287551251596,-3.98768003220409,
36.2546909526594));
#16809=CARTESIAN_POINT('Ctrl Pts',(-34.4329263800975,-4.13497132206384,
36.3588850184894));
#16810=CARTESIAN_POINT('Ctrl Pts',(-34.9537824584041,-4.87142874967366,
36.8798541610334));
#16811=CARTESIAN_POINT('Ctrl Pts',(-35.370466693267,-5.46059781902367,37.2966256819533));
#16812=CARTESIAN_POINT('Ctrl Pts',(-36.3576649944858,-6.85645163869056,
38.2840240167437));
#16813=CARTESIAN_POINT('Ctrl Pts',(-36.9281785657525,-7.66313885272879,
38.8546478427941));
#16814=CARTESIAN_POINT('Ctrl Pts',(-37.498691208412,-8.46983068145907,39.4252660733572));
#16815=CARTESIAN_POINT('',(-21.6249416886588,-8.46983068145907,49.9725521390571));
#16816=CARTESIAN_POINT('Origin',(0.0835265683620477,-8.46983068145906,0.0824317919394229));
#16817=CARTESIAN_POINT('',(0.0835265683492263,-3.96983068145906,49.9909026610602));
#16818=CARTESIAN_POINT('Ctrl Pts',(-21.6249416886588,-8.46983068145907,
49.9725521390571));
#16819=CARTESIAN_POINT('Ctrl Pts',(-18.1505891136337,-7.08833344112081,
49.9777178959269));
#16820=CARTESIAN_POINT('Ctrl Pts',(-14.6164545138694,-5.9615388332069,49.9823364948316));
#16821=CARTESIAN_POINT('Ctrl Pts',(-9.19340825173301,-4.7904640513231,49.9872996399547));
#16822=CARTESIAN_POINT('Ctrl Pts',(-7.36536697272742,-4.48684598729498,
49.9886233704762));
#16823=CARTESIAN_POINT('Ctrl Pts',(-4.58873775481838,-4.17869234558141,
49.9899767682438));
#16824=CARTESIAN_POINT('Ctrl Pts',(-3.65694097482046,-4.10048196518639,
49.9903229073071));
#16825=CARTESIAN_POINT('Ctrl Pts',(-1.7832453138779,-3.99585474310376,49.9907867430663));
#16826=CARTESIAN_POINT('Ctrl Pts',(-0.848713204691103,-3.9698306814593,
49.9909026610602));
#16827=CARTESIAN_POINT('Ctrl Pts',(0.0835265683492263,-3.96983068145906,
49.9909026610602));
#16828=CARTESIAN_POINT('',(21.7919948253829,-8.46983068145907,49.9725521390571));
#16829=CARTESIAN_POINT('Ctrl Pts',(0.0835265683492263,-3.96983068145906,
49.9909026610602));
#16830=CARTESIAN_POINT('Ctrl Pts',(3.7948657945546,-3.96983068145811,49.9909026610602));
#16831=CARTESIAN_POINT('Ctrl Pts',(7.46954951636237,-4.38596719587718,49.9890155336001));
#16832=CARTESIAN_POINT('Ctrl Pts',(12.022537961721,-5.36440184532963,49.9848668452853));
#16833=CARTESIAN_POINT('Ctrl Pts',(12.9310838207197,-5.58285881740927,49.9839501483763));
#16834=CARTESIAN_POINT('Ctrl Pts',(14.7347887768393,-6.06008817135185,49.9819775669644));
#16835=CARTESIAN_POINT('Ctrl Pts',(15.6315620628568,-6.31922781225809,49.9809201793626));
#16836=CARTESIAN_POINT('Ctrl Pts',(18.3027695373097,-7.15188128916169,49.9775797432466));
#16837=CARTESIAN_POINT('Ctrl Pts',(20.0580108836304,-7.78035142493754,49.9751302710301));
#16838=CARTESIAN_POINT('Ctrl Pts',(21.7919948253829,-8.46983068145907,49.9725521390571));
#16839=CARTESIAN_POINT('',(37.6657443451356,-8.46983068145907,39.4252660733575));
#16840=CARTESIAN_POINT('Origin',(0.0835265683620477,-8.46983068145906,0.0824317919394229));
#16841=CARTESIAN_POINT('Ctrl Pts',(37.6657443451356,-8.46983068145907,39.4252660733575));
#16842=CARTESIAN_POINT('Ctrl Pts',(37.5615737916312,-8.32253590125116,39.3210762404375));
#16843=CARTESIAN_POINT('Ctrl Pts',(37.457403207105,-8.17524127521396,39.2168862205796));
#16844=CARTESIAN_POINT('Ctrl Pts',(36.9365501255862,-7.43876893481716,38.6959351635992));
#16845=CARTESIAN_POINT('Ctrl Pts',(36.5198671524687,-6.84959358714928,38.2791712566788));
#16846=CARTESIAN_POINT('Ctrl Pts',(35.5326691698879,-5.45373818194082,37.2917748447513));
#16847=CARTESIAN_POINT('Ctrl Pts',(34.9621536716281,-4.64706055617428,36.7211393906113));
#16848=CARTESIAN_POINT('Ctrl Pts',(34.3916369666324,-3.84038894321748,36.1504966431761));
#16849=CARTESIAN_POINT('Origin',(39.8582830101054,13.1261401876617,39.8571882336827));
#16850=CARTESIAN_POINT('',(39.195370402743,-8.24885981233828,40.5201008410451));
#16851=CARTESIAN_POINT('',(39.195370402743,16.4855954176946,40.5201008410451));
#16852=CARTESIAN_POINT('',(40.5211956174677,-8.24885981233828,39.1942756263203));
#16853=CARTESIAN_POINT('Origin',(39.8582830101054,-8.24885981233827,39.8571882336827));
#16854=CARTESIAN_POINT('',(40.5211956174677,16.4855954176946,39.1942756263203));
#16855=CARTESIAN_POINT('Origin',(29.6259351744661,15.5455954176946,-47.4175682080605));
#16856=CARTESIAN_POINT('',(29.1308110078834,15.8580954176946,-46.6214788225856));
#16857=CARTESIAN_POINT('',(29.6259351744661,15.8580954176946,-48.3550682080605));
#16858=CARTESIAN_POINT('Origin',(29.6259351744661,15.8580954176946,-47.4175682080605));
#16859=CARTESIAN_POINT('',(29.6259351744661,16.1705954176946,-48.3550682080605));
#16860=CARTESIAN_POINT('',(29.6259351744661,15.5455954176946,-48.3550682080605));
#16861=CARTESIAN_POINT('',(29.1308110078834,16.1705954176946,-46.6214788225856));
#16862=CARTESIAN_POINT('Origin',(29.6259351744661,16.1705954176946,-47.4175682080605));
#16863=CARTESIAN_POINT('',(29.1308110078834,15.5455954176946,-46.6214788225856));
#16864=CARTESIAN_POINT('Origin',(44.4585265683622,15.5455954176946,-44.2925682080604));
#16865=CARTESIAN_POINT('',(47.0320559801269,15.5455954176946,-40.7545502082783));
#16866=CARTESIAN_POINT('',(40.9205085685801,15.5455954176946,-46.8660976198251));
#16867=CARTESIAN_POINT('Origin',(44.4585265683622,16.4830954176946,-44.2925682080604));
#16868=CARTESIAN_POINT('',(41.6460265683622,16.4830954176946,-44.2925682080604));
#16869=CARTESIAN_POINT('Origin',(44.4585265683622,16.4830954176946,-44.2925682080604));
#16870=CARTESIAN_POINT('',(41.6460265683622,16.4830954176946,-44.2925682080604));
#16871=CARTESIAN_POINT('Origin',(0.0835265683620477,-8.56135981233827,0.0824317919394229));
#16872=CARTESIAN_POINT('',(36.1515914195989,-3.84038894321748,-34.2256786063308));
#16873=CARTESIAN_POINT('',(36.1515914195988,-3.84038894321748,34.3905421902098));
#16874=CARTESIAN_POINT('Origin',(0.0835265683620477,-3.84038894321747,0.0824317919394229));
#16875=CARTESIAN_POINT('',(39.4263608497802,-8.46983068145907,37.664649568713));
#16876=CARTESIAN_POINT('Ctrl Pts',(36.1515914195988,-3.84038894321748,34.3905421902098));
#16877=CARTESIAN_POINT('Ctrl Pts',(36.2557857290823,-3.98768003220409,34.4947134854607));
#16878=CARTESIAN_POINT('Ctrl Pts',(36.3599797949124,-4.13497132206384,34.5988847403986));
#16879=CARTESIAN_POINT('Ctrl Pts',(36.8809489374564,-4.87142874967365,35.1197408187052));
#16880=CARTESIAN_POINT('Ctrl Pts',(37.2977204583763,-5.46059781902367,35.536425053568));
#16881=CARTESIAN_POINT('Ctrl Pts',(38.2851187931668,-6.85645163869055,36.5236233547868));
#16882=CARTESIAN_POINT('Ctrl Pts',(38.8557426192171,-7.66313885272879,37.0941369260536));
#16883=CARTESIAN_POINT('Ctrl Pts',(39.4263608497802,-8.46983068145907,37.664649568713));
#16884=CARTESIAN_POINT('',(49.9736469154797,-8.46983068145907,21.7909000489604));
#16885=CARTESIAN_POINT('Origin',(0.0835265683620477,-8.46983068145906,0.0824317919394229));
#16886=CARTESIAN_POINT('',(49.9919974374829,-3.96983068145906,0.0824317919524185));
#16887=CARTESIAN_POINT('Ctrl Pts',(49.9736469154797,-8.46983068145907,21.7909000489604));
#16888=CARTESIAN_POINT('Ctrl Pts',(49.9788126723494,-7.08833344112081,18.3165474739353));
#16889=CARTESIAN_POINT('Ctrl Pts',(49.9834312712542,-5.9615388332069,14.7824128741711));
#16890=CARTESIAN_POINT('Ctrl Pts',(49.9883944163773,-4.7904640513231,9.35936661203465));
#16891=CARTESIAN_POINT('Ctrl Pts',(49.9897181468988,-4.48684598729498,7.53132533302907));
#16892=CARTESIAN_POINT('Ctrl Pts',(49.9910715446664,-4.17869234558141,4.75469611512003));
#16893=CARTESIAN_POINT('Ctrl Pts',(49.9914176837298,-4.10048196518639,3.8228993351221));
#16894=CARTESIAN_POINT('Ctrl Pts',(49.9918815194889,-3.99585474310375,1.94920367417954));
#16895=CARTESIAN_POINT('Ctrl Pts',(49.9919974374829,-3.9698306814593,1.01467156499275));
#16896=CARTESIAN_POINT('Ctrl Pts',(49.9919974374829,-3.96983068145906,0.0824317919524185));
#16897=CARTESIAN_POINT('',(49.9736469154798,-8.46983068145907,-21.6260364650812));
#16898=CARTESIAN_POINT('Ctrl Pts',(49.9919974374829,-3.96983068145906,0.0824317919524185));
#16899=CARTESIAN_POINT('Ctrl Pts',(49.9919974374829,-3.96983068145811,-3.62890743425295));
#16900=CARTESIAN_POINT('Ctrl Pts',(49.9901103100228,-4.38596719587718,-7.30359115606072));
#16901=CARTESIAN_POINT('Ctrl Pts',(49.9859616217079,-5.36440184532962,-11.8565796014193));
#16902=CARTESIAN_POINT('Ctrl Pts',(49.985044924799,-5.58285881740927,-12.7651254604181));
#16903=CARTESIAN_POINT('Ctrl Pts',(49.9830723433871,-6.06008817135185,-14.5688304165376));
#16904=CARTESIAN_POINT('Ctrl Pts',(49.9820149557853,-6.31922781225809,-15.4656037025551));
#16905=CARTESIAN_POINT('Ctrl Pts',(49.9786745196693,-7.15188128916169,-18.136811177008));
#16906=CARTESIAN_POINT('Ctrl Pts',(49.9762250474528,-7.78035142493754,-19.8920525233287));
#16907=CARTESIAN_POINT('Ctrl Pts',(49.9736469154798,-8.46983068145907,-21.6260364650812));
#16908=CARTESIAN_POINT('',(39.4263608497803,-8.46983068145907,-37.499785984834));
#16909=CARTESIAN_POINT('Origin',(0.0835265683620477,-8.46983068145906,0.0824317919394229));
#16910=CARTESIAN_POINT('Ctrl Pts',(39.4263608497803,-8.46983068145907,-37.499785984834));
#16911=CARTESIAN_POINT('Ctrl Pts',(39.3221710168602,-8.32253590125115,-37.3956154313296));
#16912=CARTESIAN_POINT('Ctrl Pts',(39.2179809970023,-8.17524127521395,-37.2914448468034));
#16913=CARTESIAN_POINT('Ctrl Pts',(38.6970299400219,-7.43876893481715,-36.7705917652845));
#16914=CARTESIAN_POINT('Ctrl Pts',(38.2802660331016,-6.84959358714927,-36.3539087921671));
#16915=CARTESIAN_POINT('Ctrl Pts',(37.292869621174,-5.45373818194082,-35.3667108095863));
#16916=CARTESIAN_POINT('Ctrl Pts',(36.7222341670341,-4.64706055617428,-34.7961953113265));
#16917=CARTESIAN_POINT('Ctrl Pts',(36.1515914195989,-3.84038894321748,-34.2256786063308));
#16918=CARTESIAN_POINT('Origin',(39.8582830101055,13.1261401876617,-39.6923246498037));
#16919=CARTESIAN_POINT('',(39.1953704027431,12.8136401876617,-40.3552372571661));
#16920=CARTESIAN_POINT('',(40.5211956174679,12.8136401876617,-39.0294120424414));
#16921=CARTESIAN_POINT('Origin',(39.8582830101055,12.8136401876617,-39.6923246498037));
#16922=CARTESIAN_POINT('',(40.5211956174679,16.4855954176946,-39.0294120424414));
#16923=CARTESIAN_POINT('',(39.1953704027431,16.4855954176946,-40.3552372571661));
#16924=CARTESIAN_POINT('Origin',(-47.4164734316379,15.5455954176946,-29.4599768141645));
#16925=CARTESIAN_POINT('',(-48.3539734316379,15.5455954176946,-29.4599768141645));
#16926=CARTESIAN_POINT('',(-46.6203840461631,15.5455954176946,-28.9648526475817));
#16927=CARTESIAN_POINT('Origin',(-44.291473431638,15.5455954176946,-44.2925682080606));
#16928=CARTESIAN_POINT('',(-40.7534554318559,15.5455954176946,-46.8660976198253));
#16929=CARTESIAN_POINT('',(-46.8650028434027,15.5455954176946,-40.7545502082785));
#16930=CARTESIAN_POINT('Origin',(0.0835265683620477,-14.7669045823054,0.0824317919394229));
#16931=CARTESIAN_POINT('',(-4.12926308943375,11.3536536794531,-48.1715194405676));
#16932=CARTESIAN_POINT('',(0.0835265683620358,11.3536536794531,-48.3550682080606));
#16933=CARTESIAN_POINT('Origin',(0.083526568361586,11.3536536794531,0.08243179193129));
#16934=CARTESIAN_POINT('',(-48.170424664145,11.3536536794531,-4.13035786585642));
#16935=CARTESIAN_POINT('Origin',(0.0835265683620477,11.3536536794531,0.0824317919394229));
#16936=CARTESIAN_POINT('',(-48.3539734316379,11.3536536794531,0.0824317919394318));
#16937=CARTESIAN_POINT('Origin',(0.0835265683582076,11.3536536794531,0.0824317919397211));
#16938=CARTESIAN_POINT('',(-48.170424664145,11.3536536794531,4.29522144973529));
#16939=CARTESIAN_POINT('Origin',(0.0835265683498587,11.3536536794531,0.0824317919398798));
#16940=CARTESIAN_POINT('',(-4.12926308943382,11.3536536794531,48.3363830244465));
#16941=CARTESIAN_POINT('Origin',(0.0835265683620477,11.3536536794531,0.0824317919394229));
#16942=CARTESIAN_POINT('',(0.0835265683619891,11.353653679453,48.5199317919394));
#16943=CARTESIAN_POINT('Origin',(0.083526568362857,11.3536536794495,0.0824317919438222));
#16944=CARTESIAN_POINT('',(0.0835265683620321,-5.88746284406389,48.5199317919394));
#16945=CARTESIAN_POINT('',(0.0835265683620418,-14.7669045823054,48.5199317919394));
#16946=CARTESIAN_POINT('',(-4.12926308943386,-5.88746284406389,48.3363830244465));
#16947=CARTESIAN_POINT('Origin',(0.0835265683626552,-5.88746284406448,0.0824317919388395));
#16948=CARTESIAN_POINT('',(-27.2418903719914,-5.88746284406389,40.0763437697123));
#16949=CARTESIAN_POINT('Origin',(0.0835265683620477,-5.88746284406389,0.0824317919394229));
#16950=CARTESIAN_POINT('',(-27.6700355381162,-6.59535043767466,39.7804316993888));
#16951=CARTESIAN_POINT('Ctrl Pts',(-27.6700355381162,-6.59535043767466,
39.7804316993888));
#16952=CARTESIAN_POINT('Ctrl Pts',(-27.6700355381162,-6.5748915141942,39.7804316993888));
#16953=CARTESIAN_POINT('Ctrl Pts',(-27.6696020394875,-6.5545035776552,39.7807360426617));
#16954=CARTESIAN_POINT('Ctrl Pts',(-27.6687133155359,-6.53419088775616,
39.781359050409));
#16955=CARTESIAN_POINT('Ctrl Pts',(-27.6675053825142,-6.5065823498666,39.782205828117));
#16956=CARTESIAN_POINT('Ctrl Pts',(-27.6654348566091,-6.479110981132,39.783656417799));
#16957=CARTESIAN_POINT('Ctrl Pts',(-27.662458871153,-6.45179259387541,39.7857387782774));
#16958=CARTESIAN_POINT('Ctrl Pts',(-27.659628589561,-6.42581171133553,39.7877191866554));
#16959=CARTESIAN_POINT('Ctrl Pts',(-27.6559796057934,-6.39996806268515,
39.7902708432567));
#16960=CARTESIAN_POINT('Ctrl Pts',(-27.651437028073,-6.37426951908202,39.7934443375415));
#16961=CARTESIAN_POINT('Ctrl Pts',(-27.6502134107345,-6.36734719755818,
39.794299169945));
#16962=CARTESIAN_POINT('Ctrl Pts',(-27.6489247207208,-6.36043542154694,
39.795199285491));
#16963=CARTESIAN_POINT('Ctrl Pts',(-27.6475689488363,-6.3535344231453,39.7961460526717));
#16964=CARTESIAN_POINT('Ctrl Pts',(-27.6456220716296,-6.3436246465487,39.7975056025083));
#16965=CARTESIAN_POINT('Ctrl Pts',(-27.6435418871642,-6.33375626741061,
39.7989578438024));
#16966=CARTESIAN_POINT('Ctrl Pts',(-27.6413233490211,-6.32393813773166,
39.8005062057689));
#16967=CARTESIAN_POINT('Ctrl Pts',(-27.6327865713909,-6.2861586701688,39.8064641929417));
#16968=CARTESIAN_POINT('Ctrl Pts',(-27.6222074393751,-6.24912973385534,
39.813841101647));
#16969=CARTESIAN_POINT('Ctrl Pts',(-27.6092852505015,-6.21334185676859,
39.8228414839607));
#16970=CARTESIAN_POINT('Ctrl Pts',(-27.5986999063164,-6.18402584844163,
39.8302142398862));
#16971=CARTESIAN_POINT('Ctrl Pts',(-27.5865425257292,-6.15554336971624,
39.8386762248601));
#16972=CARTESIAN_POINT('Ctrl Pts',(-27.5726642605709,-6.12818087652873,
39.8483281744703));
#16973=CARTESIAN_POINT('Ctrl Pts',(-27.5725963897865,-6.12804706197383,
39.8483753767238));
#16974=CARTESIAN_POINT('Ctrl Pts',(-27.5725284783993,-6.12791327327701,
39.8484226070511));
#16975=CARTESIAN_POINT('Ctrl Pts',(-27.5724605263936,-6.12777951046925,
39.8484698654626));
#16976=CARTESIAN_POINT('Ctrl Pts',(-27.5485439724826,-6.08070002591405,
39.8651030514228));
#16977=CARTESIAN_POINT('Ctrl Pts',(-27.5191242797118,-6.03703191462283,
39.8855326916264));
#16978=CARTESIAN_POINT('Ctrl Pts',(-27.4849266552093,-6.00042962270608,
39.9092043716615));
#16979=CARTESIAN_POINT('Ctrl Pts',(-27.4687964376931,-5.98316517996187,
39.9203697480142));
#16980=CARTESIAN_POINT('Ctrl Pts',(-27.4516032390886,-5.96747341995239,
39.9322563953063));
#16981=CARTESIAN_POINT('Ctrl Pts',(-27.4334232937986,-5.95374197151968,
39.9448059878606));
#16982=CARTESIAN_POINT('Ctrl Pts',(-27.4332934621217,-5.95364390868465,
39.944895610498));
#16983=CARTESIAN_POINT('Ctrl Pts',(-27.4331635831385,-5.95354594807983,
39.9449852648623));
#16984=CARTESIAN_POINT('Ctrl Pts',(-27.4330336568643,-5.95344808981852,
39.945074950941));
#16985=CARTESIAN_POINT('Ctrl Pts',(-27.4150725570453,-5.93992009472891,
39.957473217735));
#16986=CARTESIAN_POINT('Ctrl Pts',(-27.396127418154,-5.9283828834484,39.970530680642));
#16987=CARTESIAN_POINT('Ctrl Pts',(-27.3764749543957,-5.91890173045426,
39.9840541937056));
#16988=CARTESIAN_POINT('Ctrl Pts',(-27.3568153303916,-5.90941712306448,
39.9975826339721));
#16989=CARTESIAN_POINT('Ctrl Pts',(-27.3364466141785,-5.9019896316863,40.0115783367673));
#16990=CARTESIAN_POINT('Ctrl Pts',(-27.3156304996253,-5.89673275177562,
40.0258579998765));
#16991=CARTESIAN_POINT('Ctrl Pts',(-27.2957189352997,-5.89170430603829,
40.0395171498498));
#16992=CARTESIAN_POINT('Ctrl Pts',(-27.27539694813,-5.88866186034996,40.0534368547936));
#16993=CARTESIAN_POINT('Ctrl Pts',(-27.254896375492,-5.88775186306171,40.0674541942025));
#16994=CARTESIAN_POINT('Ctrl Pts',(-27.2505682042467,-5.88755974042368,
40.0704135966757));
#16995=CARTESIAN_POINT('Ctrl Pts',(-27.2462321146088,-5.88746284473751,
40.0733773200353));
#16996=CARTESIAN_POINT('Ctrl Pts',(-27.2418903719914,-5.88746284406389,
40.0763437697123));
#16997=CARTESIAN_POINT('',(-27.6700355381162,-12.8919045823054,39.7804316993888));
#16998=CARTESIAN_POINT('',(-27.6700355381162,-14.7669045823054,39.7804316993888));
#16999=CARTESIAN_POINT('',(-29.1590516373201,-12.8919045823054,38.6967170518605));
#17000=CARTESIAN_POINT('Origin',(0.0835265683620477,-12.8919045823054,0.0824317919394229));
#17001=CARTESIAN_POINT('',(-29.1590516373201,-11.3294045823054,38.6967170518605));
#17002=CARTESIAN_POINT('',(-29.1590516373202,-14.7669045823054,38.6967170518605));
#17003=CARTESIAN_POINT('',(-29.687554196627,-10.7044045823054,38.2907313659129));
#17004=CARTESIAN_POINT('Ctrl Pts',(-29.687554196627,-10.7044045823054,38.2907313659129));
#17005=CARTESIAN_POINT('Ctrl Pts',(-29.6583757220387,-10.7044045890531,
38.313466602321));
#17006=CARTESIAN_POINT('Ctrl Pts',(-29.6292220155259,-10.7074293129566,
38.3361197336984));
#17007=CARTESIAN_POINT('Ctrl Pts',(-29.6004506138901,-10.7132787489596,
38.3584250011361));
#17008=CARTESIAN_POINT('Ctrl Pts',(-29.5697316292104,-10.7195241428141,
38.382240148461));
#17009=CARTESIAN_POINT('Ctrl Pts',(-29.5394474529814,-10.7289894494766,
38.4056595080039));
#17010=CARTESIAN_POINT('Ctrl Pts',(-29.5100173969805,-10.7414871419677,
38.4283705160146));
#17011=CARTESIAN_POINT('Ctrl Pts',(-29.4803562185471,-10.7540829823212,
38.4512598799011));
#17012=CARTESIAN_POINT('Ctrl Pts',(-29.4515613322926,-10.769759396561,38.4734306970218));
#17013=CARTESIAN_POINT('Ctrl Pts',(-29.4240644721472,-10.7883769193556,
38.4945600707541));
#17014=CARTESIAN_POINT('Ctrl Pts',(-29.3976983269581,-10.8062288597759,
38.5148205707761));
#17015=CARTESIAN_POINT('Ctrl Pts',(-29.3725246545643,-10.8267856372238,
38.5341242584425));
#17016=CARTESIAN_POINT('Ctrl Pts',(-29.3489428815995,-10.8499643578231,
38.5521714250646));
#17017=CARTESIAN_POINT('Ctrl Pts',(-29.3390845628995,-10.8596541811907,
38.5597160113203));
#17018=CARTESIAN_POINT('Ctrl Pts',(-29.3295047666208,-10.869802668699,38.5670407550077));
#17019=CARTESIAN_POINT('Ctrl Pts',(-29.3202343227628,-10.8804055842375,
38.5741224750986));
#17020=CARTESIAN_POINT('Ctrl Pts',(-29.320109404838,-10.8805484570304,38.574217900279));
#17021=CARTESIAN_POINT('Ctrl Pts',(-29.3199845450897,-10.8806914099898,
38.5743132797999));
#17022=CARTESIAN_POINT('Ctrl Pts',(-29.3198597435962,-10.8808344430918,
38.5744086136027));
#17023=CARTESIAN_POINT('Ctrl Pts',(-29.2975936746061,-10.9063532475959,
38.5914172965067));
#17024=CARTESIAN_POINT('Ctrl Pts',(-29.2772105079594,-10.9345143821537,
38.6069608464538));
#17025=CARTESIAN_POINT('Ctrl Pts',(-29.2589893852,-10.9647671393855,38.6208380965538));
#17026=CARTESIAN_POINT('Ctrl Pts',(-29.2363360171296,-11.0023788087523,
38.6380909551439));
#17027=CARTESIAN_POINT('Ctrl Pts',(-29.2170205823372,-11.0432205203856,
38.6527712187733));
#17028=CARTESIAN_POINT('Ctrl Pts',(-29.2015725997599,-11.0862730506022,
38.6644974939291));
#17029=CARTESIAN_POINT('Ctrl Pts',(-29.1879031237235,-11.1243689978983,
38.6748737379748));
#17030=CARTESIAN_POINT('Ctrl Pts',(-29.1772602520119,-11.1641988556188,
38.6829382142099));
#17031=CARTESIAN_POINT('Ctrl Pts',(-29.1700361140648,-11.2050768635799,
38.6884075571799));
#17032=CARTESIAN_POINT('Ctrl Pts',(-29.1628548700807,-11.2457121547251,
38.6938444254385));
#17033=CARTESIAN_POINT('Ctrl Pts',(-29.1590516538054,-11.2873849299308,
38.6967170393762));
#17034=CARTESIAN_POINT('Ctrl Pts',(-29.1590516373202,-11.3294045823054,
38.6967170518605));
#17035=CARTESIAN_POINT('',(-34.088419713945,-10.7044045823054,34.4112752552593));
#17036=CARTESIAN_POINT('Origin',(0.0835265683620477,-10.7044045823054,0.0824317919394229));
#17037=CARTESIAN_POINT('',(-34.585302306524,-11.3294045823054,33.9093990029365));
#17038=CARTESIAN_POINT('Ctrl Pts',(-34.585302306524,-11.3294045823054,33.9093990029365));
#17039=CARTESIAN_POINT('Ctrl Pts',(-34.585302306524,-11.2968266539588,33.9093990029365));
#17040=CARTESIAN_POINT('Ctrl Pts',(-34.583309967139,-11.2645751882994,33.9114431380499));
#17041=CARTESIAN_POINT('Ctrl Pts',(-34.5793977169934,-11.2329045289625,
33.9154520195086));
#17042=CARTESIAN_POINT('Ctrl Pts',(-34.5753887114088,-11.2004506097532,
33.9195600462345));
#17043=CARTESIAN_POINT('Ctrl Pts',(-34.5693637902165,-11.1686071890508,
33.9257310494866));
#17044=CARTESIAN_POINT('Ctrl Pts',(-34.561438831968,-11.137638677353,33.9338407021739));
#17045=CARTESIAN_POINT('Ctrl Pts',(-34.5562225782153,-11.1172550222857,
33.9391785228837));
#17046=CARTESIAN_POINT('Ctrl Pts',(-34.5501839428663,-11.0972501995401,
33.9453554341431));
#17047=CARTESIAN_POINT('Ctrl Pts',(-34.5433640724374,-11.0776955263552,
33.9523277291817));
#17048=CARTESIAN_POINT('Ctrl Pts',(-34.5432467507797,-11.0773591289561,
33.9524476729872));
#17049=CARTESIAN_POINT('Ctrl Pts',(-34.543129225895,-11.0770229370417,33.9525678233924));
#17050=CARTESIAN_POINT('Ctrl Pts',(-34.5430114980424,-11.0766869507352,
33.9526881801171));
#17051=CARTESIAN_POINT('Ctrl Pts',(-34.5278035526398,-11.0332846352166,
33.9682357201253));
#17052=CARTESIAN_POINT('Ctrl Pts',(-34.5091770363952,-10.9932074810414,
33.9872584511094));
#17053=CARTESIAN_POINT('Ctrl Pts',(-34.4875301338769,-10.9565169212725,
34.0093162098418));
#17054=CARTESIAN_POINT('Ctrl Pts',(-34.4702171093455,-10.9271720964961,
34.0269578339827));
#17055=CARTESIAN_POINT('Ctrl Pts',(-34.450971186212,-10.8999941023543,34.046541760117));
#17056=CARTESIAN_POINT('Ctrl Pts',(-34.4299825590917,-10.8750283402103,
34.067856520148));
#17057=CARTESIAN_POINT('Ctrl Pts',(-34.4297522092966,-10.8747543414318,
34.0680904492458));
#17058=CARTESIAN_POINT('Ctrl Pts',(-34.4295217184696,-10.8744806828914,
34.0683245168216));
#17059=CARTESIAN_POINT('Ctrl Pts',(-34.4292910866631,-10.8742073644078,
34.0685587228044));
#17060=CARTESIAN_POINT('Ctrl Pts',(-34.3965447492566,-10.8354001442594,
34.1018125409014));
#17061=CARTESIAN_POINT('Ctrl Pts',(-34.3610247157663,-10.8035158666735,
34.1377871350208));
#17062=CARTESIAN_POINT('Ctrl Pts',(-34.3229358340806,-10.7780132627796,
34.1762252785902));
#17063=CARTESIAN_POINT('Ctrl Pts',(-34.3059237294467,-10.7666227218479,
34.1933933783451));
#17064=CARTESIAN_POINT('Ctrl Pts',(-34.2883989200401,-10.7565058951398,
34.2110531805233));
#17065=CARTESIAN_POINT('Ctrl Pts',(-34.2703785428131,-10.7476174402578,
34.2291828798374));
#17066=CARTESIAN_POINT('Ctrl Pts',(-34.2275028321476,-10.7264692248246,
34.2723186994961));
#17067=CARTESIAN_POINT('Ctrl Pts',(-34.1835721667184,-10.7131720598041,
34.3163530721274));
#17068=CARTESIAN_POINT('Ctrl Pts',(-34.1386526306351,-10.7075299712003,
34.3611985567771));
#17069=CARTESIAN_POINT('Ctrl Pts',(-34.122042545285,-10.7054436724218,34.3777812598179));
#17070=CARTESIAN_POINT('Ctrl Pts',(-34.1052971897794,-10.7044045890775,
34.3944749165526));
#17071=CARTESIAN_POINT('Ctrl Pts',(-34.088419713945,-10.7044045823054,34.4112752552593));
#17072=CARTESIAN_POINT('',(-34.585302306524,-12.8919045823054,33.9093990029365));
#17073=CARTESIAN_POINT('',(-34.585302306524,-14.7669045823054,33.9093990029365));
#17074=CARTESIAN_POINT('Origin',(0.0835265683620477,-12.8919045823054,0.0824317919394229));
#17075=CARTESIAN_POINT('',(-36.2237408786571,-5.88746284406389,32.1444613094329));
#17076=CARTESIAN_POINT('Ctrl Pts',(-35.5742461733022,-7.07886995352309,
32.8652725680806));
#17077=CARTESIAN_POINT('Ctrl Pts',(-35.5742461905474,-7.03750286915196,
32.8652725493231));
#17078=CARTESIAN_POINT('Ctrl Pts',(-35.5760044206528,-6.99633891590724,
32.863362060325));
#17079=CARTESIAN_POINT('Ctrl Pts',(-35.5792938503007,-6.95552189493502,
32.8597839374456));
#17080=CARTESIAN_POINT('Ctrl Pts',(-35.5827607190485,-6.91250311370712,
32.8560128027158));
#17081=CARTESIAN_POINT('Ctrl Pts',(-35.5879288090133,-6.86986888736257,
32.8503888771501));
#17082=CARTESIAN_POINT('Ctrl Pts',(-35.5945728456146,-6.82778372080405,
32.8431525152966));
#17083=CARTESIAN_POINT('Ctrl Pts',(-35.6017074630717,-6.78259107933759,
32.8353818366108));
#17084=CARTESIAN_POINT('Ctrl Pts',(-35.6105445405223,-6.7380302650318,32.8257512854625));
#17085=CARTESIAN_POINT('Ctrl Pts',(-35.6208438312383,-6.69431754453991,
32.8145162260134));
#17086=CARTESIAN_POINT('Ctrl Pts',(-35.6227946757033,-6.68603768127784,
32.8123881325218));
#17087=CARTESIAN_POINT('Ctrl Pts',(-35.6247980718656,-6.67778831509133,
32.8102023731186));
#17088=CARTESIAN_POINT('Ctrl Pts',(-35.6268525024301,-6.66957102631489,
32.807960556045));
#17089=CARTESIAN_POINT('Ctrl Pts',(-35.6269399263545,-6.66922134906351,
32.8078651581037));
#17090=CARTESIAN_POINT('Ctrl Pts',(-35.6270274407123,-6.66887173803708,
32.8077696608134));
#17091=CARTESIAN_POINT('Ctrl Pts',(-35.6271150453592,-6.6685221934126,32.8076740643278));
#17092=CARTESIAN_POINT('Ctrl Pts',(-35.6522048178754,-6.56841340442319,
32.7802954473215));
#17093=CARTESIAN_POINT('Ctrl Pts',(-35.6848608854292,-6.47280389883387,
32.7446034716752));
#17094=CARTESIAN_POINT('Ctrl Pts',(-35.7243443623766,-6.38345298969106,
32.7012583566614));
#17095=CARTESIAN_POINT('Ctrl Pts',(-35.7361066934472,-6.35683489381763,
32.6883456237284));
#17096=CARTESIAN_POINT('Ctrl Pts',(-35.7484751158299,-6.33077245142131,
32.6747534913653));
#17097=CARTESIAN_POINT('Ctrl Pts',(-35.7614305154779,-6.30531282539103,
32.6604989221267));
#17098=CARTESIAN_POINT('Ctrl Pts',(-35.7616616260539,-6.30485865269114,
32.6602446357445));
#17099=CARTESIAN_POINT('Ctrl Pts',(-35.7618929228611,-6.3044046736758,32.6599901391734));
#17100=CARTESIAN_POINT('Ctrl Pts',(-35.7621244057861,-6.30395088860763,
32.6597354325154));
#17101=CARTESIAN_POINT('Ctrl Pts',(-35.7976459149302,-6.23431667928829,
32.6206501959543));
#17102=CARTESIAN_POINT('Ctrl Pts',(-35.8367531956665,-6.17022875422762,
32.5775022926724));
#17103=CARTESIAN_POINT('Ctrl Pts',(-35.8803413149544,-6.11310220427935,
32.5291872149407));
#17104=CARTESIAN_POINT('Ctrl Pts',(-35.9060289575148,-6.07943600303571,
32.500713849553));
#17105=CARTESIAN_POINT('Ctrl Pts',(-35.9332732469221,-6.04818793999518,
32.4704454107571));
#17106=CARTESIAN_POINT('Ctrl Pts',(-35.9622619599609,-6.01965292485596,
32.4381505401005));
#17107=CARTESIAN_POINT('Ctrl Pts',(-35.9625476299596,-6.01937172583458,
32.4378322894888));
#17108=CARTESIAN_POINT('Ctrl Pts',(-35.9628334737629,-6.01909078646767,
32.4375138371825));
#17109=CARTESIAN_POINT('Ctrl Pts',(-35.9631194915227,-6.01881010710761,
32.4371951829905));
#17110=CARTESIAN_POINT('Ctrl Pts',(-35.9944691963256,-5.98804553120513,
32.4022682789445));
#17111=CARTESIAN_POINT('Ctrl Pts',(-36.0275206206836,-5.96083151819991,
32.3653395143693));
#17112=CARTESIAN_POINT('Ctrl Pts',(-36.0618832816626,-5.93928082321596,
32.3268185345682));
#17113=CARTESIAN_POINT('Ctrl Pts',(-36.0900646290595,-5.92160676641468,
32.2952268858741));
#17114=CARTESIAN_POINT('Ctrl Pts',(-36.119127144603,-5.90774301103966,32.2625651728106));
#17115=CARTESIAN_POINT('Ctrl Pts',(-36.1488454697205,-5.89882514864856,
32.229071245035));
#17116=CARTESIAN_POINT('Ctrl Pts',(-36.1734061046961,-5.89145500372673,
32.2013902727479));
#17117=CARTESIAN_POINT('Ctrl Pts',(-36.1984144339698,-5.88746290319468,
32.1731411533038));
#17118=CARTESIAN_POINT('Ctrl Pts',(-36.2237408786571,-5.8874628440639,32.1444613094329));
#17119=CARTESIAN_POINT('',(-48.170424664145,-5.88746284406388,4.2952214497352));
#17120=CARTESIAN_POINT('Origin',(0.0835265683620477,-5.88746284406389,0.0824317919394229));
#17121=CARTESIAN_POINT('',(-48.3539734316379,-5.88746284406389,0.0824317919393457));
#17122=CARTESIAN_POINT('Origin',(0.083526568354122,-5.88746284406389,0.0824317919399243));
#17123=CARTESIAN_POINT('',(-48.170424664145,-5.8874628440639,-4.13035786585653));
#17124=CARTESIAN_POINT('Origin',(0.0835265683638564,-5.88746284406038,0.0824317919403333));
#17125=CARTESIAN_POINT('',(-39.9103854094111,-5.8874628440639,-27.2429851484136));
#17126=CARTESIAN_POINT('Origin',(0.0835265683620477,-5.8874628440639,0.0824317919394229));
#17127=CARTESIAN_POINT('',(-39.6144733390877,-6.59535043767467,-27.6711303145384));
#17128=CARTESIAN_POINT('Ctrl Pts',(-39.6144733390877,-6.59535043767467,
-27.6711303145384));
#17129=CARTESIAN_POINT('Ctrl Pts',(-39.6144733390877,-6.57489151419421,
-27.6711303145384));
#17130=CARTESIAN_POINT('Ctrl Pts',(-39.6147776823602,-6.55450357765519,
-27.6706968159101));
#17131=CARTESIAN_POINT('Ctrl Pts',(-39.6154006901076,-6.53419088775615,
-27.6698080919584));
#17132=CARTESIAN_POINT('Ctrl Pts',(-39.6162474678158,-6.50658234986474,
-27.6686001589365));
#17133=CARTESIAN_POINT('Ctrl Pts',(-39.617698057498,-6.47911098112832,-27.6665296330311));
#17134=CARTESIAN_POINT('Ctrl Pts',(-39.6197804179767,-6.45179259386993,
-27.6635536475747));
#17135=CARTESIAN_POINT('Ctrl Pts',(-39.6217608263548,-6.42581171132876,
-27.6607233659824));
#17136=CARTESIAN_POINT('Ctrl Pts',(-39.6243124829563,-6.3999680626771,-27.6570743822144));
#17137=CARTESIAN_POINT('Ctrl Pts',(-39.6274859772415,-6.37426951907271,
-27.6525318044936));
#17138=CARTESIAN_POINT('Ctrl Pts',(-39.6283408096446,-6.36734719755199,
-27.6513081871555));
#17139=CARTESIAN_POINT('Ctrl Pts',(-39.6292409251903,-6.36043542154385,
-27.6500194971424));
#17140=CARTESIAN_POINT('Ctrl Pts',(-39.6301876923705,-6.35353442314531,
-27.6486637252585));
#17141=CARTESIAN_POINT('Ctrl Pts',(-39.6315472422071,-6.3436246465487,-27.6467168480518));
#17142=CARTESIAN_POINT('Ctrl Pts',(-39.6329994835012,-6.33375626741061,
-27.6446366635865));
#17143=CARTESIAN_POINT('Ctrl Pts',(-39.6345478454677,-6.32393813773167,
-27.6424181254434));
#17144=CARTESIAN_POINT('Ctrl Pts',(-39.6405058326386,-6.2861586701808,-27.6338813478158));
#17145=CARTESIAN_POINT('Ctrl Pts',(-39.6478827413411,-6.24912973387886,
-27.623302215804));
#17146=CARTESIAN_POINT('Ctrl Pts',(-39.6568831236509,-6.21334185680268,
-27.6103800269361));
#17147=CARTESIAN_POINT('Ctrl Pts',(-39.6642558795785,-6.18402584846371,
-27.599794682748));
#17148=CARTESIAN_POINT('Ctrl Pts',(-39.6727178645552,-6.15554336972683,
-27.5876373021568));
#17149=CARTESIAN_POINT('Ctrl Pts',(-39.6823698141691,-6.12818087652871,
-27.5737590369931));
#17150=CARTESIAN_POINT('Ctrl Pts',(-39.6824170164226,-6.12804706197382,
-27.5736911662087));
#17151=CARTESIAN_POINT('Ctrl Pts',(-39.6824642467499,-6.127913273277,-27.5736232548215));
#17152=CARTESIAN_POINT('Ctrl Pts',(-39.6825115051614,-6.12777951046925,
-27.5735553028158));
#17153=CARTESIAN_POINT('Ctrl Pts',(-39.6991446911241,-6.0807000259069,-27.5496387489013));
#17154=CARTESIAN_POINT('Ctrl Pts',(-39.7195743313313,-6.03703191460944,
-27.5202190561252));
#17155=CARTESIAN_POINT('Ctrl Pts',(-39.7432460113709,-6.00042962268924,
-27.4860214316161));
#17156=CARTESIAN_POINT('Ctrl Pts',(-39.7544113877206,-5.98316517995156,
-27.4698912141044));
#17157=CARTESIAN_POINT('Ctrl Pts',(-39.7662980350091,-5.96747341994775,
-27.4526980155051));
#17158=CARTESIAN_POINT('Ctrl Pts',(-39.7788476275594,-5.95374197151949,
-27.4345180702209));
#17159=CARTESIAN_POINT('Ctrl Pts',(-39.7789372501968,-5.95364390868447,
-27.434388238544));
#17160=CARTESIAN_POINT('Ctrl Pts',(-39.7790269045611,-5.95354594807965,
-27.4342583595609));
#17161=CARTESIAN_POINT('Ctrl Pts',(-39.7791165906397,-5.95344808981835,
-27.4341284332866));
#17162=CARTESIAN_POINT('Ctrl Pts',(-39.7915148574324,-5.93992009473035,
-27.4161673334697));
#17163=CARTESIAN_POINT('Ctrl Pts',(-39.8045723203378,-5.92838288345103,
-27.3972221945806));
#17164=CARTESIAN_POINT('Ctrl Pts',(-39.8180958333997,-5.91890173045759,
-27.3775697308246));
#17165=CARTESIAN_POINT('Ctrl Pts',(-39.831624273665,-5.90941712306821,-27.3579101068224));
#17166=CARTESIAN_POINT('Ctrl Pts',(-39.845619976459,-5.90198963169007,-27.3375413906112));
#17167=CARTESIAN_POINT('Ctrl Pts',(-39.8598996395668,-5.89673275177899,
-27.3167252760599));
#17168=CARTESIAN_POINT('Ctrl Pts',(-39.8735587895391,-5.89170430604118,
-27.2968137117359));
#17169=CARTESIAN_POINT('Ctrl Pts',(-39.8874784944817,-5.88866186035204,
-27.2764917245678));
#17170=CARTESIAN_POINT('Ctrl Pts',(-39.9014958338896,-5.88775186306256,
-27.2559911519314));
#17171=CARTESIAN_POINT('Ctrl Pts',(-39.9044552363665,-5.88755974042401,
-27.2516629806806));
#17172=CARTESIAN_POINT('Ctrl Pts',(-39.90741895973,-5.88746284473756,-27.2473268910371));
#17173=CARTESIAN_POINT('Ctrl Pts',(-39.9103854094107,-5.88746284406391,
-27.2429851484142));
#17174=CARTESIAN_POINT('',(-39.6144733390877,-12.8919045823054,-27.6711303145384));
#17175=CARTESIAN_POINT('',(-39.6144733390877,-14.7669045823054,-27.6711303145384));
#17176=CARTESIAN_POINT('Origin',(0.0835265683620477,-12.8919045823054,0.0824317919394229));
#17177=CARTESIAN_POINT('',(-38.1247730056117,-10.7044045823054,-29.6886489730492));
#17178=CARTESIAN_POINT('Ctrl Pts',(-38.1247730056117,-10.7044045823054,
-29.6886489730492));
#17179=CARTESIAN_POINT('Ctrl Pts',(-38.1475082420184,-10.7044045890531,
-29.6594704984628));
#17180=CARTESIAN_POINT('Ctrl Pts',(-38.1701613733944,-10.7074293129562,
-29.6303167919518));
#17181=CARTESIAN_POINT('Ctrl Pts',(-38.1924666408307,-10.7132787489585,
-29.6015453903178));
#17182=CARTESIAN_POINT('Ctrl Pts',(-38.2162817881541,-10.7195241428122,
-29.57082640564));
#17183=CARTESIAN_POINT('Ctrl Pts',(-38.2397011476956,-10.7289894494735,
-29.5405422294129));
#17184=CARTESIAN_POINT('Ctrl Pts',(-38.262412155705,-10.741487141963,-29.5111121734136));
#17185=CARTESIAN_POINT('Ctrl Pts',(-38.2853015195902,-10.754082982315,-29.481450994982));
#17186=CARTESIAN_POINT('Ctrl Pts',(-38.3074723367097,-10.7697593965528,
-29.4526561087291));
#17187=CARTESIAN_POINT('Ctrl Pts',(-38.328601710441,-10.788376919345,-29.425159248585));
#17188=CARTESIAN_POINT('Ctrl Pts',(-38.3488622104619,-10.806228859763,-29.3987931033972));
#17189=CARTESIAN_POINT('Ctrl Pts',(-38.3681658981275,-10.8267856372082,
-29.3736194310045));
#17190=CARTESIAN_POINT('Ctrl Pts',(-38.3862130647491,-10.8499643578044,
-29.3500376580405));
#17191=CARTESIAN_POINT('Ctrl Pts',(-38.3937576510098,-10.8596541811777,
-29.3401793393339));
#17192=CARTESIAN_POINT('Ctrl Pts',(-38.4010823947021,-10.8698026686922,
-29.3305995430489));
#17193=CARTESIAN_POINT('Ctrl Pts',(-38.4081641147974,-10.8804055842374,
-29.321329099185));
#17194=CARTESIAN_POINT('Ctrl Pts',(-38.4082595399778,-10.8805484570303,
-29.3212041812602));
#17195=CARTESIAN_POINT('Ctrl Pts',(-38.4083549194988,-10.8806914099898,
-29.3210793215119));
#17196=CARTESIAN_POINT('Ctrl Pts',(-38.4084502533016,-10.8808344430917,
-29.3209545200184));
#17197=CARTESIAN_POINT('Ctrl Pts',(-38.4254589362055,-10.9063532475959,
-29.2986884510284));
#17198=CARTESIAN_POINT('Ctrl Pts',(-38.4410024861526,-10.9345143821538,
-29.2783052843817));
#17199=CARTESIAN_POINT('Ctrl Pts',(-38.4548797362525,-10.9647671393856,
-29.2600841616223));
#17200=CARTESIAN_POINT('Ctrl Pts',(-38.4721325948409,-11.0023788087487,
-29.2374307935541));
#17201=CARTESIAN_POINT('Ctrl Pts',(-38.4868128584692,-11.0432205203777,
-29.2181153587633));
#17202=CARTESIAN_POINT('Ctrl Pts',(-38.4985391336244,-11.0862730505896,
-29.2026673761867));
#17203=CARTESIAN_POINT('Ctrl Pts',(-38.50891537767,-11.1243689978829,-29.1889979001506));
#17204=CARTESIAN_POINT('Ctrl Pts',(-38.5169798539052,-11.1641988556004,
-29.1783550284388));
#17205=CARTESIAN_POINT('Ctrl Pts',(-38.5224491968758,-11.2050768635585,
-29.1711308904909));
#17206=CARTESIAN_POINT('Ctrl Pts',(-38.5278860651363,-11.2457121547105,
-29.1639496465043));
#17207=CARTESIAN_POINT('Ctrl Pts',(-38.5307586790751,-11.2873849299234,
-29.1601464302277));
#17208=CARTESIAN_POINT('Ctrl Pts',(-38.5307586915594,-11.3294045823054,
-29.1601464137424));
#17209=CARTESIAN_POINT('',(-34.2453168949582,-10.7044045823054,-34.0895144903672));
#17210=CARTESIAN_POINT('Origin',(0.0835265683620477,-10.7044045823054,0.0824317919394229));
#17211=CARTESIAN_POINT('',(-33.7434406426353,-11.3294045823054,-34.5863970829463));
#17212=CARTESIAN_POINT('Ctrl Pts',(-33.7434406426353,-11.3294045823054,
-34.5863970829463));
#17213=CARTESIAN_POINT('Ctrl Pts',(-33.7434406426353,-11.2968266539592,
-34.5863970829463));
#17214=CARTESIAN_POINT('Ctrl Pts',(-33.7454847777487,-11.2645751883002,
-34.5844047435613));
#17215=CARTESIAN_POINT('Ctrl Pts',(-33.7494936592074,-11.2329045289636,
-34.5804924934159));
#17216=CARTESIAN_POINT('Ctrl Pts',(-33.7536016859333,-11.2004506097536,
-34.5764834878312));
#17217=CARTESIAN_POINT('Ctrl Pts',(-33.7597726891855,-11.1686071890505,
-34.5704585666387));
#17218=CARTESIAN_POINT('Ctrl Pts',(-33.767882341873,-11.137638677352,-34.56253360839));
#17219=CARTESIAN_POINT('Ctrl Pts',(-33.7732201625828,-11.1172550222851,
-34.5573173546374));
#17220=CARTESIAN_POINT('Ctrl Pts',(-33.7793970738421,-11.0972501995398,
-34.5512787192884));
#17221=CARTESIAN_POINT('Ctrl Pts',(-33.7863693688805,-11.0776955263552,
-34.5444588488597));
#17222=CARTESIAN_POINT('Ctrl Pts',(-33.7864893126861,-11.0773591289561,
-34.544341527202));
#17223=CARTESIAN_POINT('Ctrl Pts',(-33.7866094630912,-11.0770229370417,
-34.5442240023173));
#17224=CARTESIAN_POINT('Ctrl Pts',(-33.786729819816,-11.0766869507352,-34.5441062744646));
#17225=CARTESIAN_POINT('Ctrl Pts',(-33.8022773598336,-11.0332846351901,
-34.5288983290528));
#17226=CARTESIAN_POINT('Ctrl Pts',(-33.8213000908315,-10.9932074809924,
-34.5102718127948));
#17227=CARTESIAN_POINT('Ctrl Pts',(-33.843357849581,-10.9565169212052,-34.4886249102596));
#17228=CARTESIAN_POINT('Ctrl Pts',(-33.8609994737114,-10.9271720964544,
-34.4713118857385));
#17229=CARTESIAN_POINT('Ctrl Pts',(-33.8805833998321,-10.8999941023351,
-34.4520659626183));
#17230=CARTESIAN_POINT('Ctrl Pts',(-33.9018981598468,-10.8750283402102,
-34.431077335514));
#17231=CARTESIAN_POINT('Ctrl Pts',(-33.9021320889446,-10.8747543414317,
-34.4308469857189));
#17232=CARTESIAN_POINT('Ctrl Pts',(-33.9023661565204,-10.8744806828913,
-34.4306164948919));
#17233=CARTESIAN_POINT('Ctrl Pts',(-33.9026003625033,-10.8742073644076,
-34.4303858630855));
#17234=CARTESIAN_POINT('Ctrl Pts',(-33.9358541806131,-10.8354001442444,
-34.3976395256663));
#17235=CARTESIAN_POINT('Ctrl Pts',(-33.9718287747473,-10.8035158666488,
-34.3621194921614));
#17236=CARTESIAN_POINT('Ctrl Pts',(-34.0102669183332,-10.77801326275,-34.3240306104592));
#17237=CARTESIAN_POINT('Ctrl Pts',(-34.0274350180743,-10.7666227218303,
-34.307018505839));
#17238=CARTESIAN_POINT('Ctrl Pts',(-34.0450948202377,-10.7565058951319,
-34.2894936964469));
#17239=CARTESIAN_POINT('Ctrl Pts',(-34.0632245195362,-10.7476174402576,
-34.2714733192354));
#17240=CARTESIAN_POINT('Ctrl Pts',(-34.1063603392022,-10.726469224821,-34.2285976085627));
#17241=CARTESIAN_POINT('Ctrl Pts',(-34.1503947118412,-10.7131720597996,
-34.1846669431258));
#17242=CARTESIAN_POINT('Ctrl Pts',(-34.1952401964989,-10.7075299711974,
-34.1397474070344));
#17243=CARTESIAN_POINT('Ctrl Pts',(-34.2118228995322,-10.7054436724208,
-34.1231373216918));
#17244=CARTESIAN_POINT('Ctrl Pts',(-34.2285165562592,-10.7044045890775,
-34.1063919661939));
#17245=CARTESIAN_POINT('Ctrl Pts',(-34.2453168949582,-10.7044045823054,
-34.0895144903673));
#17246=CARTESIAN_POINT('',(-33.7434406426353,-12.8919045823054,-34.5863970829463));
#17247=CARTESIAN_POINT('',(-33.7434406426353,-14.7669045823054,-34.5863970829463));
#17248=CARTESIAN_POINT('',(-32.6993142077795,-12.8919045823054,-35.5753409497245));
#17249=CARTESIAN_POINT('Origin',(0.0835265683620477,-12.8919045823054,0.0824317919394229));
#17250=CARTESIAN_POINT('',(-32.6993142077795,-7.07886995352309,-35.5753409497245));
#17251=CARTESIAN_POINT('',(-32.6993142077795,-14.7669045823054,-35.5753409497245));
#17252=CARTESIAN_POINT('',(-31.9785029491318,-5.88746284406389,-36.2248356550794));
#17253=CARTESIAN_POINT('Ctrl Pts',(-32.6993142077795,-7.07886995352308,
-35.5753409497245));
#17254=CARTESIAN_POINT('Ctrl Pts',(-32.6993141890216,-7.03750286914987,
-35.57534096697));
#17255=CARTESIAN_POINT('Ctrl Pts',(-32.6974037000232,-6.99633891590311,
-35.5770991970757));
#17256=CARTESIAN_POINT('Ctrl Pts',(-32.6938255771434,-6.95552189492887,
-35.5803886267239));
#17257=CARTESIAN_POINT('Ctrl Pts',(-32.6900544424132,-6.91250311369896,
-35.5838554954721));
#17258=CARTESIAN_POINT('Ctrl Pts',(-32.6844305168472,-6.86986888735245,
-35.5890235854372));
#17259=CARTESIAN_POINT('Ctrl Pts',(-32.6771941549931,-6.82778372079203,
-35.595667622039));
#17260=CARTESIAN_POINT('Ctrl Pts',(-32.6694234763069,-6.78259107932476,
-35.6028022394964));
#17261=CARTESIAN_POINT('Ctrl Pts',(-32.6597929251584,-6.7380302650182,-35.6116393169474));
#17262=CARTESIAN_POINT('Ctrl Pts',(-32.6485578657088,-6.6943175445256,-35.6219386076638));
#17263=CARTESIAN_POINT('Ctrl Pts',(-32.6464297722183,-6.68603768126831,
-35.6238894521278));
#17264=CARTESIAN_POINT('Ctrl Pts',(-32.6442440128163,-6.67778831508655,
-35.6258928482889));
#17265=CARTESIAN_POINT('Ctrl Pts',(-32.642002195744,-6.66957102631483,-35.6279472788522));
#17266=CARTESIAN_POINT('Ctrl Pts',(-32.6419067978027,-6.66922134906346,
-35.6280347027766));
#17267=CARTESIAN_POINT('Ctrl Pts',(-32.6418113005124,-6.66887173803703,
-35.6281222171344));
#17268=CARTESIAN_POINT('Ctrl Pts',(-32.6417157040268,-6.66852219341255,
-35.6282098217813));
#17269=CARTESIAN_POINT('Ctrl Pts',(-32.6143370871273,-6.56841340481339,
-35.6532995941997));
#17270=CARTESIAN_POINT('Ctrl Pts',(-32.5786451116525,-6.47280389957943,
-35.6859556615968));
#17271=CARTESIAN_POINT('Ctrl Pts',(-32.5352999968674,-6.38345299073607,
-35.725439138337));
#17272=CARTESIAN_POINT('Ctrl Pts',(-32.5223872637832,-6.35683489449971,
-35.7372014695457));
#17273=CARTESIAN_POINT('Ctrl Pts',(-32.5087951312509,-6.33077245175437,
-35.7495698920825));
#17274=CARTESIAN_POINT('Ctrl Pts',(-32.4945405618258,-6.30531282539085,
-35.7625252919));
#17275=CARTESIAN_POINT('Ctrl Pts',(-32.4942862754435,-6.30485865269096,
-35.762756402476));
#17276=CARTESIAN_POINT('Ctrl Pts',(-32.4940317788724,-6.30440467367563,
-35.7629876992832));
#17277=CARTESIAN_POINT('Ctrl Pts',(-32.4937770722144,-6.30395088860745,
-35.7632191822082));
#17278=CARTESIAN_POINT('Ctrl Pts',(-32.4546918357289,-6.23431667942218,
-35.7987406912838));
#17279=CARTESIAN_POINT('Ctrl Pts',(-32.4115439325377,-6.17022875447443,
-35.8378479719379));
#17280=CARTESIAN_POINT('Ctrl Pts',(-32.3632288549189,-6.11310220460954,
-35.8814360911247));
#17281=CARTESIAN_POINT('Ctrl Pts',(-32.3347554894498,-6.0794360032401,-35.9071237337589));
#17282=CARTESIAN_POINT('Ctrl Pts',(-32.3044870505616,-6.04818794008861,
-35.9343680232496));
#17283=CARTESIAN_POINT('Ctrl Pts',(-32.2721921797993,-6.01965292485617,
-35.9633567363832));
#17284=CARTESIAN_POINT('Ctrl Pts',(-32.2718739291876,-6.01937172583479,
-35.9636424063819));
#17285=CARTESIAN_POINT('Ctrl Pts',(-32.2715554768813,-6.01909078646788,
-35.9639282501853));
#17286=CARTESIAN_POINT('Ctrl Pts',(-32.2712368226893,-6.01881010710782,
-35.9642142679451));
#17287=CARTESIAN_POINT('Ctrl Pts',(-32.2363099186584,-5.98804553121875,
-35.9955639727344));
#17288=CARTESIAN_POINT('Ctrl Pts',(-32.1993811541001,-5.9608315182235,-36.0286153970774));
#17289=CARTESIAN_POINT('Ctrl Pts',(-32.1608601743171,-5.93928082324375,
-36.0629780580403));
#17290=CARTESIAN_POINT('Ctrl Pts',(-32.1292685256388,-5.92160676644647,
-36.0911594054232));
#17291=CARTESIAN_POINT('Ctrl Pts',(-32.096606812592,-5.90774301107131,-36.120221920952));
#17292=CARTESIAN_POINT('Ctrl Pts',(-32.0631128848336,-5.89882514867459,
-36.1499402460543));
#17293=CARTESIAN_POINT('Ctrl Pts',(-32.0354319125146,-5.89145500373582,
-36.1745008810583));
#17294=CARTESIAN_POINT('Ctrl Pts',(-32.0071827930371,-5.88746290319435,
-36.1995092103617));
#17295=CARTESIAN_POINT('Ctrl Pts',(-31.9785029491318,-5.88746284406389,
-36.2248356550794));
#17296=CARTESIAN_POINT('',(-4.12926308943377,-5.88746284406389,-48.1715194405676));
#17297=CARTESIAN_POINT('Origin',(0.0835265683620477,-5.88746284406389,0.0824317919394229));
#17298=CARTESIAN_POINT('',(0.0835265683620358,-5.88746284406389,-48.3550682080606));
#17299=CARTESIAN_POINT('Origin',(0.0835265683620358,-5.88746284406389,0.0824317919239981));
#17300=CARTESIAN_POINT('',(4.29631622615797,-5.88746284406389,-48.1715194405676));
#17301=CARTESIAN_POINT('Origin',(0.0835265683614989,-5.88746284406448,0.0824317919478901));
#17302=CARTESIAN_POINT('',(27.4089435087152,-5.88746284406389,-39.9114801858336));
#17303=CARTESIAN_POINT('Origin',(0.0835265683620477,-5.88746284406389,0.0824317919394229));
#17304=CARTESIAN_POINT('',(27.83708867484,-6.59535043767467,-39.6155681155102));
#17305=CARTESIAN_POINT('Ctrl Pts',(27.83708867484,-6.59535043767467,-39.6155681155102));
#17306=CARTESIAN_POINT('Ctrl Pts',(27.83708867484,-6.57489151419422,-39.6155681155102));
#17307=CARTESIAN_POINT('Ctrl Pts',(27.836655176211,-6.55450357765523,-39.6158724587832));
#17308=CARTESIAN_POINT('Ctrl Pts',(27.8357664522595,-6.53419088775619,-39.6164954665305));
#17309=CARTESIAN_POINT('Ctrl Pts',(27.8345585192379,-6.50658234986769,-39.6173422442385));
#17310=CARTESIAN_POINT('Ctrl Pts',(27.832487993333,-6.47911098113413,-39.6187928339203));
#17311=CARTESIAN_POINT('Ctrl Pts',(27.8295120078771,-6.45179259387858,-39.6208751943986));
#17312=CARTESIAN_POINT('Ctrl Pts',(27.8266817262854,-6.42581171133972,-39.6228556027764));
#17313=CARTESIAN_POINT('Ctrl Pts',(27.823032742518,-6.39996806269036,-39.6254072593775));
#17314=CARTESIAN_POINT('Ctrl Pts',(27.8184901647979,-6.37426951908824,-39.6285807536621));
#17315=CARTESIAN_POINT('Ctrl Pts',(27.8172665474591,-6.36734719756233,-39.6294355860658));
#17316=CARTESIAN_POINT('Ctrl Pts',(27.815977857445,-6.36043542154902,-39.6303357016121));
#17317=CARTESIAN_POINT('Ctrl Pts',(27.8146220855601,-6.35353442314532,-39.631282468793));
#17318=CARTESIAN_POINT('Ctrl Pts',(27.8126752083534,-6.34362464654871,-39.6326420186297));
#17319=CARTESIAN_POINT('Ctrl Pts',(27.8105950238881,-6.33375626741062,-39.6340942599238));
#17320=CARTESIAN_POINT('Ctrl Pts',(27.808376485745,-6.32393813773167,-39.6356426218902));
#17321=CARTESIAN_POINT('Ctrl Pts',(27.7998397081135,-6.28615867016339,-39.6416006090639));
#17322=CARTESIAN_POINT('Ctrl Pts',(27.7892605760959,-6.24912973384469,-39.6489775177705));
#17323=CARTESIAN_POINT('Ctrl Pts',(27.7763383872198,-6.21334185675317,-39.6579779000859));
#17324=CARTESIAN_POINT('Ctrl Pts',(27.7657530430359,-6.18402584843166,-39.6653506560106));
#17325=CARTESIAN_POINT('Ctrl Pts',(27.7535956624506,-6.15554336971148,-39.6738126409832));
#17326=CARTESIAN_POINT('Ctrl Pts',(27.7397173972946,-6.1281808765288,-39.6834645905917));
#17327=CARTESIAN_POINT('Ctrl Pts',(27.7396495265103,-6.1280470619739,-39.6835117928452));
#17328=CARTESIAN_POINT('Ctrl Pts',(27.739581615123,-6.12791327327708,-39.6835590231725));
#17329=CARTESIAN_POINT('Ctrl Pts',(27.7395136631173,-6.12777951046932,-39.683606281584));
#17330=CARTESIAN_POINT('Ctrl Pts',(27.7155971091982,-6.08070002589822,-39.7002394675499));
#17331=CARTESIAN_POINT('Ctrl Pts',(27.6861774164157,-6.03703191459323,-39.7206691077616));
#17332=CARTESIAN_POINT('Ctrl Pts',(27.6519797918984,-6.00042962266881,-39.7443407878068));
#17333=CARTESIAN_POINT('Ctrl Pts',(27.6358495743922,-5.98316517993923,-39.7555061641526));
#17334=CARTESIAN_POINT('Ctrl Pts',(27.6186563757994,-5.96747341994242,-39.7673928114367));
#17335=CARTESIAN_POINT('Ctrl Pts',(27.6004764305224,-5.95374197151959,-39.7799424039819));
#17336=CARTESIAN_POINT('Ctrl Pts',(27.6003465988456,-5.95364390868456,-39.7800320266193));
#17337=CARTESIAN_POINT('Ctrl Pts',(27.6002167198624,-5.95354594807974,-39.7801216809836));
#17338=CARTESIAN_POINT('Ctrl Pts',(27.6000867935882,-5.95344808981843,-39.7802113670623));
#17339=CARTESIAN_POINT('Ctrl Pts',(27.5821256937692,-5.93992009472884,-39.7926096338564));
#17340=CARTESIAN_POINT('Ctrl Pts',(27.5631805548778,-5.92838288344823,-39.8056670967633));
#17341=CARTESIAN_POINT('Ctrl Pts',(27.5435280911194,-5.91890173045397,-39.819190609827));
#17342=CARTESIAN_POINT('Ctrl Pts',(27.5238684671156,-5.90941712306419,-39.8327190500933));
#17343=CARTESIAN_POINT('Ctrl Pts',(27.5034997509027,-5.90198963168597,-39.8467147528884));
#17344=CARTESIAN_POINT('Ctrl Pts',(27.4826836363497,-5.89673275177528,-39.8609944159974));
#17345=CARTESIAN_POINT('Ctrl Pts',(27.4627720720246,-5.89170430603802,-39.8746535659704));
#17346=CARTESIAN_POINT('Ctrl Pts',(27.4424500848554,-5.88866186034975,-39.8885732709138));
#17347=CARTESIAN_POINT('Ctrl Pts',(27.421949512218,-5.88775186306162,-39.9025906103224));
#17348=CARTESIAN_POINT('Ctrl Pts',(27.4176213409719,-5.88755974042358,-39.905550012796));
#17349=CARTESIAN_POINT('Ctrl Pts',(27.4132852513333,-5.88746284473744,-39.9085137361562));
#17350=CARTESIAN_POINT('Ctrl Pts',(27.4089435087152,-5.8874628440639,-39.9114801858336));
#17351=CARTESIAN_POINT('',(27.83708867484,-12.8919045823054,-39.6155681155102));
#17352=CARTESIAN_POINT('',(27.83708867484,-14.7669045823054,-39.6155681155102));
#17353=CARTESIAN_POINT('',(29.326104774044,-12.8919045823054,-38.5318534679819));
#17354=CARTESIAN_POINT('Origin',(0.0835265683620477,-12.8919045823054,0.0824317919394229));
#17355=CARTESIAN_POINT('',(29.326104774044,-11.3294045823054,-38.5318534679819));
#17356=CARTESIAN_POINT('',(29.326104774044,-14.7669045823054,-38.5318534679819));
#17357=CARTESIAN_POINT('',(29.8546073333508,-10.7044045823054,-38.1258677820342));
#17358=CARTESIAN_POINT('Ctrl Pts',(29.8546073333508,-10.7044045823054,-38.1258677820342));
#17359=CARTESIAN_POINT('Ctrl Pts',(29.8254288587611,-10.7044045890531,-38.1486030184435));
#17360=CARTESIAN_POINT('Ctrl Pts',(29.7962751522468,-10.7074293129569,-38.171256149822));
#17361=CARTESIAN_POINT('Ctrl Pts',(29.7675037506096,-10.7132787489605,-38.1935614172609));
#17362=CARTESIAN_POINT('Ctrl Pts',(29.7367847659283,-10.7195241428156,-38.2173765645869));
#17363=CARTESIAN_POINT('Ctrl Pts',(29.7065005896978,-10.728989449479,-38.240795924131));
#17364=CARTESIAN_POINT('Ctrl Pts',(29.6770705336955,-10.7414871419714,-38.2635069321427));
#17365=CARTESIAN_POINT('Ctrl Pts',(29.6474093552607,-10.7540829823262,-38.2863962960303));
#17366=CARTESIAN_POINT('Ctrl Pts',(29.6186144690049,-10.7697593965676,-38.3085671131521));
#17367=CARTESIAN_POINT('Ctrl Pts',(29.5911176088584,-10.7883769193641,-38.3296964868852));
#17368=CARTESIAN_POINT('Ctrl Pts',(29.5647514636682,-10.8062288597864,-38.349956986908));
#17369=CARTESIAN_POINT('Ctrl Pts',(29.5395777912734,-10.8267856372365,-38.3692606745751));
#17370=CARTESIAN_POINT('Ctrl Pts',(29.515996018308,-10.8499643578382,-38.3873078411977));
#17371=CARTESIAN_POINT('Ctrl Pts',(29.5061376996133,-10.8596541812013,-38.3948524274492));
#17372=CARTESIAN_POINT('Ctrl Pts',(29.4965579033399,-10.8698026687045,-38.4021771711327));
#17373=CARTESIAN_POINT('Ctrl Pts',(29.4872874594866,-10.8804055842375,-38.4092588912199));
#17374=CARTESIAN_POINT('Ctrl Pts',(29.4871625415619,-10.8805484570304,-38.4093543164003));
#17375=CARTESIAN_POINT('Ctrl Pts',(29.4870376818136,-10.8806914099898,-38.4094496959213));
#17376=CARTESIAN_POINT('Ctrl Pts',(29.48691288032,-10.8808344430918,-38.4095450297241));
#17377=CARTESIAN_POINT('Ctrl Pts',(29.46464681133,-10.9063532475959,-38.426553712628));
#17378=CARTESIAN_POINT('Ctrl Pts',(29.4442636446832,-10.9345143821536,-38.4420972625752));
#17379=CARTESIAN_POINT('Ctrl Pts',(29.4260425219237,-10.9647671393854,-38.4559745126752));
#17380=CARTESIAN_POINT('Ctrl Pts',(29.4033891538499,-11.0023788087573,-38.4732273712679));
#17381=CARTESIAN_POINT('Ctrl Pts',(29.3840737190552,-11.0432205203968,-38.4879076348992));
#17382=CARTESIAN_POINT('Ctrl Pts',(29.3686257364766,-11.08627305062,-38.4996339100558));
#17383=CARTESIAN_POINT('Ctrl Pts',(29.3549562604386,-11.1243689979234,-38.5100101541028));
#17384=CARTESIAN_POINT('Ctrl Pts',(29.3443133887266,-11.1641988556518,-38.5180746303382));
#17385=CARTESIAN_POINT('Ctrl Pts',(29.3370892507806,-11.2050768636209,-38.5235439733073));
#17386=CARTESIAN_POINT('Ctrl Pts',(29.3299080068013,-11.2457121547532,-38.5289808415623));
#17387=CARTESIAN_POINT('Ctrl Pts',(29.3261047905288,-11.287384929945,-38.5318534554979));
#17388=CARTESIAN_POINT('Ctrl Pts',(29.326104774044,-11.3294045823054,-38.5318534679819));
#17389=CARTESIAN_POINT('',(34.2554728506688,-10.7044045823054,-34.2464116713807));
#17390=CARTESIAN_POINT('Origin',(0.0835265683620477,-10.7044045823054,0.0824317919394229));
#17391=CARTESIAN_POINT('Ctrl Pts',(34.7523554432478,-11.3294045823054,-33.7445354190578));
#17392=CARTESIAN_POINT('Ctrl Pts',(34.7523554432478,-11.2968266539615,-33.7445354190578));
#17393=CARTESIAN_POINT('Ctrl Pts',(34.7503631038632,-11.2645751883046,-33.7465795541709));
#17394=CARTESIAN_POINT('Ctrl Pts',(34.7464508537183,-11.2329045289702,-33.750588435629));
#17395=CARTESIAN_POINT('Ctrl Pts',(34.7424418481339,-11.2004506097603,-33.7546964623547));
#17396=CARTESIAN_POINT('Ctrl Pts',(34.7364169269417,-11.1686071890573,-33.7608674656065));
#17397=CARTESIAN_POINT('Ctrl Pts',(34.7284919686934,-11.1376386773589,-33.7689771182937));
#17398=CARTESIAN_POINT('Ctrl Pts',(34.7232757149404,-11.1172550222896,-33.7743149390039));
#17399=CARTESIAN_POINT('Ctrl Pts',(34.7172370795908,-11.097250199542,-33.7804918502638));
#17400=CARTESIAN_POINT('Ctrl Pts',(34.7104172091613,-11.0776955263552,-33.7874641453031));
#17401=CARTESIAN_POINT('Ctrl Pts',(34.7102998875036,-11.0773591289561,-33.7875840891086));
#17402=CARTESIAN_POINT('Ctrl Pts',(34.7101823626189,-11.0770229370417,-33.7877042395138));
#17403=CARTESIAN_POINT('Ctrl Pts',(34.7100646347662,-11.0766869507352,-33.7878245962385));
#17404=CARTESIAN_POINT('Ctrl Pts',(34.6948566893518,-11.0332846351828,-33.8033721362587));
#17405=CARTESIAN_POINT('Ctrl Pts',(34.6762301730901,-10.993207480979,-33.8223948672603));
#17406=CARTESIAN_POINT('Ctrl Pts',(34.6545832705503,-10.9565169211867,-33.8444526260146));
#17407=CARTESIAN_POINT('Ctrl Pts',(34.637270246032,-10.927172096443,-33.8620942501421));
#17408=CARTESIAN_POINT('Ctrl Pts',(34.6180243229155,-10.8999941023299,-33.8816781762591));
#17409=CARTESIAN_POINT('Ctrl Pts',(34.5970356958156,-10.8750283402102,-33.9029929362693));
#17410=CARTESIAN_POINT('Ctrl Pts',(34.5968053460205,-10.8747543414317,-33.9032268653671));
#17411=CARTESIAN_POINT('Ctrl Pts',(34.5965748551935,-10.8744806828913,-33.9034609329429));
#17412=CARTESIAN_POINT('Ctrl Pts',(34.5963442233871,-10.8742073644076,-33.9036951389258));
#17413=CARTESIAN_POINT('Ctrl Pts',(34.5635978859542,-10.8354001442282,-33.9369489570494));
#17414=CARTESIAN_POINT('Ctrl Pts',(34.5280778524334,-10.8035158666223,-33.9729235511997));
#17415=CARTESIAN_POINT('Ctrl Pts',(34.4899889707131,-10.7780132627181,-34.0113616948038));
#17416=CARTESIAN_POINT('Ctrl Pts',(34.4729768661079,-10.7666227218115,-34.0285297945297));
#17417=CARTESIAN_POINT('Ctrl Pts',(34.4554520567317,-10.7565058951237,-34.0461895966771));
#17418=CARTESIAN_POINT('Ctrl Pts',(34.437431679537,-10.7476174402577,-34.0643192959587));
#17419=CARTESIAN_POINT('Ctrl Pts',(34.3945559688426,-10.7264692248103,-34.1074551156465));
#17420=CARTESIAN_POINT('Ctrl Pts',(34.3506253033834,-10.7131720597862,-34.1514894883078));
#17421=CARTESIAN_POINT('Ctrl Pts',(34.3057057672688,-10.707529971189,-34.1963349729886));
#17422=CARTESIAN_POINT('Ctrl Pts',(34.2890956819482,-10.705443672418,-34.2129176759997));
#17423=CARTESIAN_POINT('Ctrl Pts',(34.2723503264727,-10.7044045890775,-34.2296113327044));
#17424=CARTESIAN_POINT('Ctrl Pts',(34.2554728506688,-10.7044045823054,-34.2464116713807));
#17425=CARTESIAN_POINT('',(35.7412993100261,-12.8919045823054,-32.700408984202));
#17426=CARTESIAN_POINT('Origin',(0.0835265683620477,-12.8919045823054,0.0824317919394229));
#17427=CARTESIAN_POINT('',(35.7412993100261,-7.07886995352309,-32.700408984202));
#17428=CARTESIAN_POINT('',(35.7412993100261,-14.7669045823054,-32.700408984202));
#17429=CARTESIAN_POINT('',(36.390794015381,-5.88746284406389,-31.9795977255543));
#17430=CARTESIAN_POINT('Ctrl Pts',(35.7412993100261,-7.0788699535231,-32.700408984202));
#17431=CARTESIAN_POINT('Ctrl Pts',(35.7412993272714,-7.03750286915156,-32.7004089654444));
#17432=CARTESIAN_POINT('Ctrl Pts',(35.7430575573768,-6.99633891590645,-32.6984984764463));
#17433=CARTESIAN_POINT('Ctrl Pts',(35.7463469870247,-6.95552189493383,-32.6949203535668));
#17434=CARTESIAN_POINT('Ctrl Pts',(35.7498138557726,-6.91250311370568,-32.6911492188369));
#17435=CARTESIAN_POINT('Ctrl Pts',(35.7549819457374,-6.8698688873609,-32.6855252932712));
#17436=CARTESIAN_POINT('Ctrl Pts',(35.7616259823388,-6.82778372080215,-32.6782889314176));
#17437=CARTESIAN_POINT('Ctrl Pts',(35.7687605997959,-6.78259107933578,-32.6705182527317));
#17438=CARTESIAN_POINT('Ctrl Pts',(35.7775976772465,-6.73803026503009,-32.6608877015835));
#17439=CARTESIAN_POINT('Ctrl Pts',(35.7878969679625,-6.69431754453829,-32.6496526421344));
#17440=CARTESIAN_POINT('Ctrl Pts',(35.7898478124275,-6.68603768127677,-32.6475245486429));
#17441=CARTESIAN_POINT('Ctrl Pts',(35.7918512085896,-6.6777883150908,-32.6453387892399));
#17442=CARTESIAN_POINT('Ctrl Pts',(35.7939056391539,-6.6695710263149,-32.6430969721664));
#17443=CARTESIAN_POINT('Ctrl Pts',(35.7939930630783,-6.66922134906352,-32.6430015742251));
#17444=CARTESIAN_POINT('Ctrl Pts',(35.7940805774361,-6.66887173803709,-32.6429060769348));
#17445=CARTESIAN_POINT('Ctrl Pts',(35.794168182083,-6.66852219341261,-32.6428104804492));
#17446=CARTESIAN_POINT('Ctrl Pts',(35.8192579545976,-6.56841340442999,-32.6154318634447));
#17447=CARTESIAN_POINT('Ctrl Pts',(35.8519140221486,-6.47280389884689,-32.5797398878015));
#17448=CARTESIAN_POINT('Ctrl Pts',(35.8913974990923,-6.38345298970913,-32.5363947727917));
#17449=CARTESIAN_POINT('Ctrl Pts',(35.9031598301653,-6.35683489382933,-32.5234820398561));
#17450=CARTESIAN_POINT('Ctrl Pts',(35.9155282525506,-6.33077245142688,-32.5098899074902));
#17451=CARTESIAN_POINT('Ctrl Pts',(35.9284836522014,-6.30531282539074,-32.4956353382484));
#17452=CARTESIAN_POINT('Ctrl Pts',(35.9287147627774,-6.30485865269084,-32.4953810518661));
#17453=CARTESIAN_POINT('Ctrl Pts',(35.9289460595847,-6.30440467367551,-32.495126555295));
#17454=CARTESIAN_POINT('Ctrl Pts',(35.9291775425096,-6.30395088860734,-32.4948718486371));
#17455=CARTESIAN_POINT('Ctrl Pts',(35.9646990516115,-6.23431667937041,-32.4557866121226));
#17456=CARTESIAN_POINT('Ctrl Pts',(36.0038063322973,-6.17022875437937,-32.4126387088964));
#17457=CARTESIAN_POINT('Ctrl Pts',(36.047394451523,-6.1131022044825,-32.3643236312342));
#17458=CARTESIAN_POINT('Ctrl Pts',(36.0730820941289,-6.07943600316146,-32.3358502657963));
#17459=CARTESIAN_POINT('Ctrl Pts',(36.1003263835876,-6.04818794005264,-32.3055818269435));
#17460=CARTESIAN_POINT('Ctrl Pts',(36.1293150966848,-6.019652924856,-32.2732869562219));
#17461=CARTESIAN_POINT('Ctrl Pts',(36.1296007666834,-6.01937172583463,-32.2729687056102));
#17462=CARTESIAN_POINT('Ctrl Pts',(36.1298866104868,-6.01909078646772,-32.2726502533039));
#17463=CARTESIAN_POINT('Ctrl Pts',(36.1301726282466,-6.01881010710765,-32.2723315991119));
#17464=CARTESIAN_POINT('Ctrl Pts',(36.1615223330518,-5.98804553120297,-32.2374046950633));
#17465=CARTESIAN_POINT('Ctrl Pts',(36.1945737574123,-5.96083151819561,-32.2004759304853));
#17466=CARTESIAN_POINT('Ctrl Pts',(36.228936418394,-5.93928082321056,-32.1619549506812));
#17467=CARTESIAN_POINT('Ctrl Pts',(36.2571177657912,-5.92160676640953,-32.1303633019867));
#17468=CARTESIAN_POINT('Ctrl Pts',(36.2861802813351,-5.90774301103496,-32.0977015889228));
#17469=CARTESIAN_POINT('Ctrl Pts',(36.3158986064529,-5.89882514864486,-32.0642076611468));
#17470=CARTESIAN_POINT('Ctrl Pts',(36.3404592414257,-5.89145500372474,-32.0365266888627));
#17471=CARTESIAN_POINT('Ctrl Pts',(36.3654675706966,-5.88746290319394,-32.0082775694218));
#17472=CARTESIAN_POINT('Ctrl Pts',(36.390794015381,-5.88746284406389,-31.9795977255543));
#17473=CARTESIAN_POINT('',(48.3374778008691,-5.88746284406389,-4.1303578658561));
#17474=CARTESIAN_POINT('Origin',(0.0835265683620477,-5.88746284406389,0.0824317919394229));
#17475=CARTESIAN_POINT('',(48.5210265683621,-5.88746284406389,0.082431791939678));
#17476=CARTESIAN_POINT('Origin',(0.0835265683666275,-5.88746284406447,0.082431791939678));
#17477=CARTESIAN_POINT('',(48.3374778008691,-5.88746284406389,4.29522144973544));
#17478=CARTESIAN_POINT('Origin',(0.0835265683722142,-5.88746284406447,0.0824317919400358));
#17479=CARTESIAN_POINT('',(40.0774385461352,-5.88746284406389,27.4078487322925));
#17480=CARTESIAN_POINT('Origin',(0.0835265683620477,-5.88746284406389,0.0824317919394229));
#17481=CARTESIAN_POINT('Ctrl Pts',(39.7815264758118,-6.59535043767467,27.8359938984173));
#17482=CARTESIAN_POINT('Ctrl Pts',(39.7815264758118,-6.57489151419421,27.8359938984173));
#17483=CARTESIAN_POINT('Ctrl Pts',(39.7818308190845,-6.5545035776552,27.8355603997887));
#17484=CARTESIAN_POINT('Ctrl Pts',(39.7824538268318,-6.53419088775616,27.8346716758371));
#17485=CARTESIAN_POINT('Ctrl Pts',(39.78330060454,-6.50658234986543,27.8334637428152));
#17486=CARTESIAN_POINT('Ctrl Pts',(39.7847511942221,-6.47911098112967,27.83139321691));
#17487=CARTESIAN_POINT('Ctrl Pts',(39.7868335547006,-6.45179259387194,27.8284172314537));
#17488=CARTESIAN_POINT('Ctrl Pts',(39.7888139630787,-6.42581171133136,27.8255869498616));
#17489=CARTESIAN_POINT('Ctrl Pts',(39.7913656196801,-6.39996806268029,27.8219379660937));
#17490=CARTESIAN_POINT('Ctrl Pts',(39.7945391139651,-6.37426951907649,27.8173953883731));
#17491=CARTESIAN_POINT('Ctrl Pts',(39.7953939463684,-6.3673471975545,27.8161717710348));
#17492=CARTESIAN_POINT('Ctrl Pts',(39.7962940619142,-6.36043542154511,27.8148830810215));
#17493=CARTESIAN_POINT('Ctrl Pts',(39.7972408290946,-6.35353442314531,27.8135273091373));
#17494=CARTESIAN_POINT('Ctrl Pts',(39.7986003789312,-6.34362464654871,27.8115804319307));
#17495=CARTESIAN_POINT('Ctrl Pts',(39.8000526202253,-6.33375626741061,27.8095002474653));
#17496=CARTESIAN_POINT('Ctrl Pts',(39.8016009821918,-6.32393813773167,27.8072817093222));
#17497=CARTESIAN_POINT('Ctrl Pts',(39.8075589693638,-6.28615867017362,27.798744931693));
#17498=CARTESIAN_POINT('Ctrl Pts',(39.814935878068,-6.24912973386477,27.7881657996788));
#17499=CARTESIAN_POINT('Ctrl Pts',(39.8239362603802,-6.21334185678225,27.7752436108075));
#17500=CARTESIAN_POINT('Ctrl Pts',(39.8313090163065,-6.18402584845048,27.7646582666212));
#17501=CARTESIAN_POINT('Ctrl Pts',(39.8397710012815,-6.15554336972048,27.7525008860325));
#17502=CARTESIAN_POINT('Ctrl Pts',(39.8494229508932,-6.12818087652871,27.738622620872));
#17503=CARTESIAN_POINT('Ctrl Pts',(39.8494701531467,-6.12804706197381,27.7385547500876));
#17504=CARTESIAN_POINT('Ctrl Pts',(39.849517383474,-6.12791327327699,27.7384868387004));
#17505=CARTESIAN_POINT('Ctrl Pts',(39.8495646418855,-6.12777951046923,27.7384188866947));
#17506=CARTESIAN_POINT('Ctrl Pts',(39.8661978278375,-6.08070002593731,27.7145023327956));
#17507=CARTESIAN_POINT('Ctrl Pts',(39.886627468029,-6.03703191466581,27.6850826400422));
#17508=CARTESIAN_POINT('Ctrl Pts',(39.9102991480491,-6.0004296227601,27.6508850155614));
#17509=CARTESIAN_POINT('Ctrl Pts',(39.921464524412,-5.98316517999444,27.6347547980304));
#17510=CARTESIAN_POINT('Ctrl Pts',(39.9333511717159,-5.96747341996643,27.617561599409));
#17511=CARTESIAN_POINT('Ctrl Pts',(39.9459007642834,-5.95374197151939,27.5993816540998));
#17512=CARTESIAN_POINT('Ctrl Pts',(39.9459903869208,-5.95364390868437,27.5992518224229));
#17513=CARTESIAN_POINT('Ctrl Pts',(39.9460800412851,-5.95354594807955,27.5991219434397));
#17514=CARTESIAN_POINT('Ctrl Pts',(39.9461697273638,-5.95344808981824,27.5989920171655));
#17515=CARTESIAN_POINT('Ctrl Pts',(39.9585679941583,-5.93992009472827,27.5810309173459));
#17516=CARTESIAN_POINT('Ctrl Pts',(39.9716254570657,-5.92838288344757,27.5620857784538));
#17517=CARTESIAN_POINT('Ctrl Pts',(39.9851489701298,-5.91890173045338,27.5424333146948));
#17518=CARTESIAN_POINT('Ctrl Pts',(39.9986774103974,-5.90941712306312,27.5227736906891));
#17519=CARTESIAN_POINT('Ctrl Pts',(40.0126731131938,-5.9019896316848,27.5024049744744));
#17520=CARTESIAN_POINT('Ctrl Pts',(40.0269527763041,-5.89673275177423,27.4815888599194));
#17521=CARTESIAN_POINT('Ctrl Pts',(40.0406119262791,-5.89170430603683,27.4616772955916));
#17522=CARTESIAN_POINT('Ctrl Pts',(40.0545316312244,-5.88866186034882,27.4413553084195));
#17523=CARTESIAN_POINT('Ctrl Pts',(40.0685489706349,-5.88775186306124,27.4208547357792));
#17524=CARTESIAN_POINT('Ctrl Pts',(40.0715083731049,-5.88755974042358,27.4165265645385));
#17525=CARTESIAN_POINT('Ctrl Pts',(40.0744720964614,-5.88746284473756,27.4121904749052));
#17526=CARTESIAN_POINT('Ctrl Pts',(40.0774385461352,-5.88746284406389,27.4078487322925));
#17527=CARTESIAN_POINT('',(38.6978118282835,-12.8919045823054,29.3250099976212));
#17528=CARTESIAN_POINT('Origin',(0.0835265683620477,-12.8919045823054,0.0824317919394229));
#17529=CARTESIAN_POINT('',(38.6978118282835,-11.3294045823054,29.3250099976212));
#17530=CARTESIAN_POINT('',(38.6978118282835,-14.7669045823054,29.3250099976212));
#17531=CARTESIAN_POINT('',(38.2918261423358,-10.7044045823054,29.8535125569281));
#17532=CARTESIAN_POINT('Ctrl Pts',(38.2918261423358,-10.7044045823054,29.8535125569281));
#17533=CARTESIAN_POINT('Ctrl Pts',(38.3145613787425,-10.7044045890531,29.8243340823417));
#17534=CARTESIAN_POINT('Ctrl Pts',(38.3372145101185,-10.7074293129562,29.7951803758307));
#17535=CARTESIAN_POINT('Ctrl Pts',(38.3595197775548,-10.7132787489585,29.7664089741967));
#17536=CARTESIAN_POINT('Ctrl Pts',(38.3833349248782,-10.7195241428123,29.7356899895188));
#17537=CARTESIAN_POINT('Ctrl Pts',(38.4067542844197,-10.7289894494735,29.7054058132917));
#17538=CARTESIAN_POINT('Ctrl Pts',(38.4294652924291,-10.7414871419631,29.6759757572924));
#17539=CARTESIAN_POINT('Ctrl Pts',(38.4523546563143,-10.754082982315,29.6463145788608));
#17540=CARTESIAN_POINT('Ctrl Pts',(38.4745254734339,-10.7697593965528,29.6175196926078));
#17541=CARTESIAN_POINT('Ctrl Pts',(38.4956548471652,-10.7883769193451,29.5900228324637));
#17542=CARTESIAN_POINT('Ctrl Pts',(38.5159153471861,-10.8062288597631,29.563656687276));
#17543=CARTESIAN_POINT('Ctrl Pts',(38.5352190348517,-10.8267856372083,29.5384830148832));
#17544=CARTESIAN_POINT('Ctrl Pts',(38.5532662014732,-10.8499643578046,29.5149012419193));
#17545=CARTESIAN_POINT('Ctrl Pts',(38.5608107877339,-10.8596541811778,29.5050429232126));
#17546=CARTESIAN_POINT('Ctrl Pts',(38.5681355314262,-10.8698026686923,29.4954631269277));
#17547=CARTESIAN_POINT('Ctrl Pts',(38.5752172515215,-10.8804055842374,29.4861926830638));
#17548=CARTESIAN_POINT('Ctrl Pts',(38.5753126767019,-10.8805484570303,29.4860677651391));
#17549=CARTESIAN_POINT('Ctrl Pts',(38.5754080562229,-10.8806914099898,29.4859429053908));
#17550=CARTESIAN_POINT('Ctrl Pts',(38.5755033900257,-10.8808344430917,29.4858181038972));
#17551=CARTESIAN_POINT('Ctrl Pts',(38.5925120729296,-10.9063532475959,29.4635520349072));
#17552=CARTESIAN_POINT('Ctrl Pts',(38.6080556228767,-10.9345143821538,29.4431688682605));
#17553=CARTESIAN_POINT('Ctrl Pts',(38.6219328729767,-10.9647671393856,29.4249477455011));
#17554=CARTESIAN_POINT('Ctrl Pts',(38.6391857315655,-11.0023788087495,29.4022943774324));
#17555=CARTESIAN_POINT('Ctrl Pts',(38.653865995194,-11.0432205203795,29.3829789426412));
#17556=CARTESIAN_POINT('Ctrl Pts',(38.6655922703494,-11.0862730505925,29.3675309600644));
#17557=CARTESIAN_POINT('Ctrl Pts',(38.6759685143952,-11.124368997887,29.353861484028));
#17558=CARTESIAN_POINT('Ctrl Pts',(38.6840329906305,-11.1641988556059,29.3432186123161));
#17559=CARTESIAN_POINT('Ctrl Pts',(38.689502333601,-11.2050768635654,29.3359944743684));
#17560=CARTESIAN_POINT('Ctrl Pts',(38.6949392018608,-11.2457121547152,29.3288132303826));
#17561=CARTESIAN_POINT('Ctrl Pts',(38.6978118157992,-11.2873849299258,29.3250100141064));
#17562=CARTESIAN_POINT('Ctrl Pts',(38.6978118282835,-11.3294045823054,29.3250099976212));
#17563=CARTESIAN_POINT('',(34.4123700316823,-10.7044045823054,34.2543780742461));
#17564=CARTESIAN_POINT('Origin',(0.0835265683620477,-10.7044045823054,0.0824317919394229));
#17565=CARTESIAN_POINT('',(33.9104937793594,-11.3294045823054,34.7512606668251));
#17566=CARTESIAN_POINT('Ctrl Pts',(33.9104937793594,-11.3294045823054,34.7512606668251));
#17567=CARTESIAN_POINT('Ctrl Pts',(33.9104937793594,-11.2968266539584,34.7512606668251));
#17568=CARTESIAN_POINT('Ctrl Pts',(33.9125379144729,-11.2645751882985,34.7492683274401));
#17569=CARTESIAN_POINT('Ctrl Pts',(33.9165467959317,-11.2329045289611,34.7453560772944));
#17570=CARTESIAN_POINT('Ctrl Pts',(33.9206548226578,-11.2004506097504,34.7413470717096));
#17571=CARTESIAN_POINT('Ctrl Pts',(33.9268258259103,-11.1686071890466,34.7353221505169));
#17572=CARTESIAN_POINT('Ctrl Pts',(33.9349354785982,-11.1376386773475,34.7273971922678));
#17573=CARTESIAN_POINT('Ctrl Pts',(33.9402732993077,-11.1172550222821,34.7221809385155));
#17574=CARTESIAN_POINT('Ctrl Pts',(33.9464502105666,-11.0972501995383,34.7161423031669));
#17575=CARTESIAN_POINT('Ctrl Pts',(33.9534225056046,-11.0776955263552,34.7093224327386));
#17576=CARTESIAN_POINT('Ctrl Pts',(33.9535424494101,-11.077359128956,34.7092051110809));
#17577=CARTESIAN_POINT('Ctrl Pts',(33.9536625998153,-11.0770229370416,34.7090875861962));
#17578=CARTESIAN_POINT('Ctrl Pts',(33.95378295654,-11.0766869507352,34.7089698583435));
#17579=CARTESIAN_POINT('Ctrl Pts',(33.9693304965678,-11.033284635162,34.6937619129218));
#17580=CARTESIAN_POINT('Ctrl Pts',(33.9883532275802,-10.9932074809405,34.6751353966495));
#17581=CARTESIAN_POINT('Ctrl Pts',(34.0104109863479,-10.9565169211339,34.6534884940964));
#17582=CARTESIAN_POINT('Ctrl Pts',(34.0280526104672,-10.9271720964104,34.6361754695862));
#17583=CARTESIAN_POINT('Ctrl Pts',(34.0476365365734,-10.8999941023149,34.6169295464802));
#17584=CARTESIAN_POINT('Ctrl Pts',(34.0689512965709,-10.8750283402102,34.5959409193929));
#17585=CARTESIAN_POINT('Ctrl Pts',(34.0691852256687,-10.8747543414317,34.5957105695978));
#17586=CARTESIAN_POINT('Ctrl Pts',(34.0694192932445,-10.8744806828913,34.5954800787707));
#17587=CARTESIAN_POINT('Ctrl Pts',(34.0696534992273,-10.8742073644076,34.5952494469643));
#17588=CARTESIAN_POINT('Ctrl Pts',(34.1029073173621,-10.8354001442153,34.5625031095206));
#17589=CARTESIAN_POINT('Ctrl Pts',(34.1388819115252,-10.8035158666011,34.5269830759871));
#17590=CARTESIAN_POINT('Ctrl Pts',(34.1773200551437,-10.7780132626927,34.4888941942524));
#17591=CARTESIAN_POINT('Ctrl Pts',(34.1944881548576,-10.7666227217964,34.4718820896591));
#17592=CARTESIAN_POINT('Ctrl Pts',(34.2121479569922,-10.7565058951171,34.4543572802956));
#17593=CARTESIAN_POINT('Ctrl Pts',(34.2302776562603,-10.7476174402577,34.4363369031143));
#17594=CARTESIAN_POINT('Ctrl Pts',(34.2734134759625,-10.7264692248033,34.3934611924055));
#17595=CARTESIAN_POINT('Ctrl Pts',(34.3174478486389,-10.7131720597773,34.3495305269313));
#17596=CARTESIAN_POINT('Ctrl Pts',(34.3622933333352,-10.7075299711833,34.3046109908009));
#17597=CARTESIAN_POINT('Ctrl Pts',(34.3788760363315,-10.7054436724162,34.2880009054952));
#17598=CARTESIAN_POINT('Ctrl Pts',(34.3955696930212,-10.7044045890775,34.2712555500347));
#17599=CARTESIAN_POINT('Ctrl Pts',(34.4123700316823,-10.7044045823054,34.2543780742461));
#17600=CARTESIAN_POINT('',(33.9104937793594,-12.8919045823054,34.7512606668251));
#17601=CARTESIAN_POINT('',(33.9104937793594,-14.7669045823054,34.7512606668251));
#17602=CARTESIAN_POINT('',(32.8663673445036,-12.8919045823054,35.7402045336033));
#17603=CARTESIAN_POINT('Origin',(0.0835265683620477,-12.8919045823054,0.0824317919394229));
#17604=CARTESIAN_POINT('',(32.8663673445036,-7.07886995352309,35.7402045336033));
#17605=CARTESIAN_POINT('',(32.8663673445036,-14.7669045823054,35.7402045336033));
#17606=CARTESIAN_POINT('',(32.1455560858559,-5.88746284406389,36.3896992389582));
#17607=CARTESIAN_POINT('Ctrl Pts',(32.8663673445036,-7.07886995352308,35.7402045336033));
#17608=CARTESIAN_POINT('Ctrl Pts',(32.8663673257456,-7.03750286914797,35.740204550849));
#17609=CARTESIAN_POINT('Ctrl Pts',(32.8644568367469,-6.99633891589931,35.7419627809549));
#17610=CARTESIAN_POINT('Ctrl Pts',(32.8608787138668,-6.95552189492322,35.7452522106034));
#17611=CARTESIAN_POINT('Ctrl Pts',(32.8571075791363,-6.91250311369205,35.7487190793519));
#17612=CARTESIAN_POINT('Ctrl Pts',(32.8514836535699,-6.86986888734432,35.7538871693173));
#17613=CARTESIAN_POINT('Ctrl Pts',(32.8442472917155,-6.82778372078273,35.7605312059195));
#17614=CARTESIAN_POINT('Ctrl Pts',(32.836476613029,-6.78259107931536,35.7676658233771));
#17615=CARTESIAN_POINT('Ctrl Pts',(32.8268460618802,-6.73803026500875,35.7765029008283));
#17616=CARTESIAN_POINT('Ctrl Pts',(32.8156110024303,-6.69431754451611,35.786802191545));
#17617=CARTESIAN_POINT('Ctrl Pts',(32.8134829089406,-6.68603768126203,35.7887530360083));
#17618=CARTESIAN_POINT('Ctrl Pts',(32.8112971495395,-6.67778831508346,35.7907564321687));
#17619=CARTESIAN_POINT('Ctrl Pts',(32.809055332468,-6.66957102631489,35.7928108627312));
#17620=CARTESIAN_POINT('Ctrl Pts',(32.8089599345267,-6.66922134906352,35.7928982866556));
#17621=CARTESIAN_POINT('Ctrl Pts',(32.8088644372364,-6.66887173803708,35.7929858010134));
#17622=CARTESIAN_POINT('Ctrl Pts',(32.8087688407508,-6.6685221934126,35.7930734056603));
#17623=CARTESIAN_POINT('Ctrl Pts',(32.7813902237688,-6.56841340451216,35.8181631781542));
#17624=CARTESIAN_POINT('Ctrl Pts',(32.7456982481617,-6.47280389900386,35.8508192456723));
#17625=CARTESIAN_POINT('Ctrl Pts',(32.7023531332,-6.38345298992926,35.8903027225724));
#17626=CARTESIAN_POINT('Ctrl Pts',(32.6894404002325,-6.35683489397307,35.9020650536745));
#17627=CARTESIAN_POINT('Ctrl Pts',(32.6758482678309,-6.33077245149717,35.9144334760923));
#17628=CARTESIAN_POINT('Ctrl Pts',(32.6615936985498,-6.30531282539089,35.9273888757788));
#17629=CARTESIAN_POINT('Ctrl Pts',(32.6613394121676,-6.304858652691,35.9276199863548));
#17630=CARTESIAN_POINT('Ctrl Pts',(32.6610849155965,-6.30440467367567,35.9278512831621));
#17631=CARTESIAN_POINT('Ctrl Pts',(32.6608302089385,-6.3039508886075,35.9280827660871));
#17632=CARTESIAN_POINT('Ctrl Pts',(32.6217449724213,-6.23431667936603,35.9636042751914));
#17633=CARTESIAN_POINT('Ctrl Pts',(32.5785970691921,-6.170228754371,36.0027115558799));
#17634=CARTESIAN_POINT('Ctrl Pts',(32.530281991526,-6.11310220447119,36.0462996751091));
#17635=CARTESIAN_POINT('Ctrl Pts',(32.501808626091,-6.07943600315446,36.0719873177124));
#17636=CARTESIAN_POINT('Ctrl Pts',(32.4715401872415,-6.04818794004946,36.0992316071682));
#17637=CARTESIAN_POINT('Ctrl Pts',(32.4392453165235,-6.01965292485606,36.1282203202621));
#17638=CARTESIAN_POINT('Ctrl Pts',(32.4389270659117,-6.01937172583469,36.1285059902607));
#17639=CARTESIAN_POINT('Ctrl Pts',(32.4386086136055,-6.01909078646778,36.1287918340641));
#17640=CARTESIAN_POINT('Ctrl Pts',(32.4382899594135,-6.01881010710771,36.1290778518239));
#17641=CARTESIAN_POINT('Ctrl Pts',(32.4033630553722,-5.98804553120947,36.1604275566225));
#17642=CARTESIAN_POINT('Ctrl Pts',(32.3664342908023,-5.96083151820698,36.1934789809758));
#17643=CARTESIAN_POINT('Ctrl Pts',(32.3279133110069,-5.93928082322402,36.2278416419498));
#17644=CARTESIAN_POINT('Ctrl Pts',(32.2963216623196,-5.92160676642473,36.2560229893406));
#17645=CARTESIAN_POINT('Ctrl Pts',(32.2636599492633,-5.90774301105001,36.2850855048778));
#17646=CARTESIAN_POINT('Ctrl Pts',(32.2301660214951,-5.8988251486572,36.3148038299887));
#17647=CARTESIAN_POINT('Ctrl Pts',(32.2024850491961,-5.89145500372915,36.3393644649749));
#17648=CARTESIAN_POINT('Ctrl Pts',(32.1742359297396,-5.8874629031939,36.3643727942596));
#17649=CARTESIAN_POINT('Ctrl Pts',(32.1455560858559,-5.8874628440639,36.3896992389582));
#17650=CARTESIAN_POINT('',(4.29631622615791,-5.88746284406389,48.3363830244465));
#17651=CARTESIAN_POINT('Origin',(0.0835265683620477,-5.88746284406389,0.0824317919394229));
#17652=CARTESIAN_POINT('Origin',(0.0835265683623214,-5.88746284406272,0.0824317919373119));
#17653=CARTESIAN_POINT('',(4.29631622615776,11.353653679453,48.3363830244465));
#17654=CARTESIAN_POINT('Origin',(0.0835265683614805,11.3536536794601,0.0824317919346118));
#17655=CARTESIAN_POINT('',(48.3374778008691,11.353653679453,4.29522144973533));
#17656=CARTESIAN_POINT('Origin',(0.0835265683620477,11.353653679453,0.0824317919394229));
#17657=CARTESIAN_POINT('',(48.5210265683621,11.353653679453,0.0824317919395275));
#17658=CARTESIAN_POINT('Origin',(0.0835265683614939,11.3536536794601,0.0824317919395275));
#17659=CARTESIAN_POINT('',(48.3374778008691,11.3536536794531,-4.13035786585629));
#17660=CARTESIAN_POINT('Origin',(0.0835265683752606,11.3536536794495,0.0824317919385903));
#17661=CARTESIAN_POINT('',(4.29631622615795,11.3536536794531,-48.1715194405676));
#17662=CARTESIAN_POINT('Origin',(0.0835265683620477,11.3536536794531,0.0824317919394229));
#17663=CARTESIAN_POINT('Origin',(0.0835265683620358,11.3536536794531,0.0824317919406425));
#17664=CARTESIAN_POINT('Origin',(-44.291473431638,16.4830954176946,-44.2925682080606));
#17665=CARTESIAN_POINT('',(-44.291473431638,16.4830954176946,-41.4800682080606));
#17666=CARTESIAN_POINT('Origin',(-44.291473431638,16.4830954176946,-44.2925682080606));
#17667=CARTESIAN_POINT('',(-44.291473431638,16.4830954176946,-41.4800682080606));
#17668=CARTESIAN_POINT('Origin',(0.0835265683620477,-8.56135981233827,0.0824317919394229));
#17669=CARTESIAN_POINT('',(-34.2245838299083,-3.84038894321748,-35.9856330592973));
#17670=CARTESIAN_POINT('',(34.3916369666325,-3.84038894321748,-35.9856330592972));
#17671=CARTESIAN_POINT('Origin',(0.0835265683620477,-3.84038894321748,0.0824317919394229));
#17672=CARTESIAN_POINT('',(37.6657443451358,-8.46983068145907,-39.2604024894786));
#17673=CARTESIAN_POINT('Ctrl Pts',(34.3916369666325,-3.84038894321748,-35.9856330592972));
#17674=CARTESIAN_POINT('Ctrl Pts',(34.4958082618834,-3.98768003220409,-36.0898273687807));
#17675=CARTESIAN_POINT('Ctrl Pts',(34.5999795168213,-4.13497132206384,-36.1940214346108));
#17676=CARTESIAN_POINT('Ctrl Pts',(35.120835595128,-4.87142874967365,-36.7149905771548));
#17677=CARTESIAN_POINT('Ctrl Pts',(35.5375198299908,-5.46059781902367,-37.1317620980747));
#17678=CARTESIAN_POINT('Ctrl Pts',(36.5247181312096,-6.85645163869056,-38.1191604328652));
#17679=CARTESIAN_POINT('Ctrl Pts',(37.0952317024764,-7.66313885272879,-38.6897842589155));
#17680=CARTESIAN_POINT('Ctrl Pts',(37.6657443451358,-8.46983068145907,-39.2604024894786));
#17681=CARTESIAN_POINT('',(21.7919948253829,-8.46983068145907,-49.8076885551783));
#17682=CARTESIAN_POINT('Origin',(0.0835265683620477,-8.46983068145906,0.0824317919394229));
#17683=CARTESIAN_POINT('',(0.0835265683748736,-3.96983068145906,-49.8260390771814));
#17684=CARTESIAN_POINT('Ctrl Pts',(21.7919948253829,-8.46983068145907,-49.8076885551783));
#17685=CARTESIAN_POINT('Ctrl Pts',(18.3176422503578,-7.08833344112081,-49.812854312048));
#17686=CARTESIAN_POINT('Ctrl Pts',(14.7835076505935,-5.9615388332069,-49.8174729109528));
#17687=CARTESIAN_POINT('Ctrl Pts',(9.36046138845711,-4.79046405132309,-49.8224360560758));
#17688=CARTESIAN_POINT('Ctrl Pts',(7.53242010945153,-4.48684598729498,-49.8237597865973));
#17689=CARTESIAN_POINT('Ctrl Pts',(4.75579089154249,-4.17869234558141,-49.825113184365));
#17690=CARTESIAN_POINT('Ctrl Pts',(3.82399411154456,-4.10048196518639,-49.8254593234283));
#17691=CARTESIAN_POINT('Ctrl Pts',(1.950298450602,-3.99585474310376,-49.8259231591874));
#17692=CARTESIAN_POINT('Ctrl Pts',(1.0157663414152,-3.9698306814593,-49.8260390771814));
#17693=CARTESIAN_POINT('Ctrl Pts',(0.0835265683748736,-3.96983068145906,
-49.8260390771814));
#17694=CARTESIAN_POINT('',(-21.6249416886588,-8.46983068145907,-49.8076885551783));
#17695=CARTESIAN_POINT('Ctrl Pts',(0.0835265683748736,-3.96983068145906,
-49.8260390771814));
#17696=CARTESIAN_POINT('Ctrl Pts',(-3.6278126578305,-3.96983068145811,-49.8260390771814));
#17697=CARTESIAN_POINT('Ctrl Pts',(-7.30249637963826,-4.38596719587718,
-49.8241519497213));
#17698=CARTESIAN_POINT('Ctrl Pts',(-11.8554848249969,-5.36440184532962,
-49.8200032614064));
#17699=CARTESIAN_POINT('Ctrl Pts',(-12.7640306839956,-5.58285881740927,
-49.8190865644975));
#17700=CARTESIAN_POINT('Ctrl Pts',(-14.5677356401152,-6.06008817135185,
-49.8171139830856));
#17701=CARTESIAN_POINT('Ctrl Pts',(-15.4645089261327,-6.31922781225809,
-49.8160565954838));
#17702=CARTESIAN_POINT('Ctrl Pts',(-18.1357164005855,-7.15188128916168,
-49.8127161593677));
#17703=CARTESIAN_POINT('Ctrl Pts',(-19.8909577469063,-7.78035142493754,
-49.8102666871513));
#17704=CARTESIAN_POINT('Ctrl Pts',(-21.6249416886588,-8.46983068145907,
-49.8076885551783));
#17705=CARTESIAN_POINT('',(-37.4986912084115,-8.46983068145907,-39.2604024894787));
#17706=CARTESIAN_POINT('Origin',(0.0835265683620477,-8.46983068145906,0.0824317919394229));
#17707=CARTESIAN_POINT('Ctrl Pts',(-37.4986912084115,-8.46983068145907,
-39.2604024894787));
#17708=CARTESIAN_POINT('Ctrl Pts',(-37.3945206549071,-8.32253590125116,
-39.1562126565586));
#17709=CARTESIAN_POINT('Ctrl Pts',(-37.2903500703809,-8.17524127521396,
-39.0520226367007));
#17710=CARTESIAN_POINT('Ctrl Pts',(-36.7694969888621,-7.43876893481716,
-38.5310715797203));
#17711=CARTESIAN_POINT('Ctrl Pts',(-36.3528140157447,-6.84959358714928,
-38.1143076728));
#17712=CARTESIAN_POINT('Ctrl Pts',(-35.3656160331638,-5.45373818194082,
-37.1269112608724));
#17713=CARTESIAN_POINT('Ctrl Pts',(-34.795100534904,-4.64706055617428,-36.5562758067325));
#17714=CARTESIAN_POINT('Ctrl Pts',(-34.2245838299083,-3.84038894321748,
-35.9856330592973));
#17715=CARTESIAN_POINT('Origin',(-39.6912298733813,13.1261401876617,-39.6923246498039));
#17716=CARTESIAN_POINT('',(-40.3541424807436,12.8136401876617,-39.0294120424415));
#17717=CARTESIAN_POINT('',(-39.0283172660189,12.8136401876617,-40.3552372571663));
#17718=CARTESIAN_POINT('Origin',(-39.6912298733813,12.8136401876617,-39.6923246498039));
#17719=CARTESIAN_POINT('',(-39.0283172660189,16.4855954176946,-40.3552372571663));
#17720=CARTESIAN_POINT('',(-40.3541424807436,16.4855954176946,-39.0294120424415));
#17721=CARTESIAN_POINT('Origin',(16.7670594440865,-17.1192738307565,25.3269308122136));
#17722=CARTESIAN_POINT('',(16.3756046859818,-11.3294045823054,26.5140547199659));
#17723=CARTESIAN_POINT('',(17.9541833518389,-11.3294045823054,25.7183855703182));
#17724=CARTESIAN_POINT('Origin',(16.7670594440865,-11.3294045823054,25.3269308122136));
#17725=CARTESIAN_POINT('',(16.3756046859818,-11.0169045823054,26.5140547199659));
#17726=CARTESIAN_POINT('',(16.3756046859818,-17.1192738307565,26.5140547199659));
#17727=CARTESIAN_POINT('',(17.9541833518389,-11.0169045823054,25.7183855703182));
#17728=CARTESIAN_POINT('Origin',(16.7670594440865,-11.0169045823054,25.3269308122136));
#17729=CARTESIAN_POINT('',(17.9541833518389,-17.1192738307565,25.7183855703182));
#17730=CARTESIAN_POINT('Origin',(-44.291473431638,16.4830954176946,-44.2925682080606));
#17731=CARTESIAN_POINT('',(49.7710265683621,16.4830954176946,44.4574317919394));
#17732=CARTESIAN_POINT('',(49.7710265683619,16.4830954176946,37.6072170232579));
#17733=CARTESIAN_POINT('',(49.7710265683622,16.4830954176946,-44.2925682080604));
#17734=CARTESIAN_POINT('',(48.8335265683621,16.4830954176946,37.6072170232579));
#17735=CARTESIAN_POINT('',(0.0835265683620477,16.4830954176946,37.6072170232579));
#17736=CARTESIAN_POINT('',(48.8335265683621,16.4830954176946,38.3884670232579));
#17737=CARTESIAN_POINT('',(48.8335265683619,16.4830954176946,0.0824317919392537));
#17738=CARTESIAN_POINT('',(48.8335265683621,16.4830954176946,40.1612670779183));
#17739=CARTESIAN_POINT('',(41.173224139993,16.4830954176946,46.8471376742924));
#17740=CARTESIAN_POINT('Origin',(44.4585265683621,16.4830954176946,44.4574317919394));
#17741=CARTESIAN_POINT('',(40.162361854341,16.4830954176946,48.8324317919394));
#17742=CARTESIAN_POINT('Origin',(40.162361854341,16.4830954176946,47.5824317919394));
#17743=CARTESIAN_POINT('',(29.625935174466,16.4830954176946,48.8324317919394));
#17744=CARTESIAN_POINT('',(29.625935174466,16.4830954176946,48.8324317919394));
#17745=CARTESIAN_POINT('',(28.9657696190223,16.4830954176946,46.5209792779729));
#17746=CARTESIAN_POINT('Origin',(29.625935174466,16.4830954176946,47.5824317919394));
#17747=CARTESIAN_POINT('',(46.5220740543956,16.4830954176946,28.9646748425997));
#17748=CARTESIAN_POINT('Origin',(0.0835265683620477,16.4830954176946,0.0824317919394229));
#17749=CARTESIAN_POINT('',(48.8335265683621,16.4830954176946,29.6248403980433));
#17750=CARTESIAN_POINT('Origin',(47.583526568362,16.4830954176946,29.6248403980433));
#17751=CARTESIAN_POINT('',(48.8335265683621,16.4830954176946,35.8884670232579));
#17752=CARTESIAN_POINT('',(48.8335265683621,16.4830954176946,40.1612670779183));
#17753=CARTESIAN_POINT('',(48.8335265683621,16.4830954176946,36.6697170232579));
#17754=CARTESIAN_POINT('',(48.8335265683619,16.4830954176946,0.0824317919392537));
#17755=CARTESIAN_POINT('',(49.7710265683619,16.4830954176946,36.6697170232579));
#17756=CARTESIAN_POINT('',(0.0835265683620477,16.4830954176946,36.6697170232579));
#17757=CARTESIAN_POINT('',(49.7710265683622,16.4830954176946,-44.2925682080604));
#17758=CARTESIAN_POINT('',(49.7710265683622,16.4830954176946,-44.2925682080604));
#17759=CARTESIAN_POINT('',(44.4585265683622,16.4830954176946,-49.6050682080606));
#17760=CARTESIAN_POINT('Origin',(44.4585265683622,16.4830954176946,-44.2925682080604));
#17761=CARTESIAN_POINT('',(-44.2914734316379,16.4830954176946,-49.6050682080606));
#17762=CARTESIAN_POINT('',(-44.2914734316379,16.4830954176946,-49.6050682080606));
#17763=CARTESIAN_POINT('',(-49.603973431638,16.4830954176946,-44.2925682080605));
#17764=CARTESIAN_POINT('Origin',(-44.291473431638,16.4830954176946,-44.2925682080606));
#17765=CARTESIAN_POINT('',(-49.6039734316384,16.4830954176946,44.4574317919389));
#17766=CARTESIAN_POINT('',(-49.603973431638,16.4830954176946,44.4574317919389));
#17767=CARTESIAN_POINT('',(-44.2914734316384,16.4830954176946,49.7699317919394));
#17768=CARTESIAN_POINT('Origin',(-44.2914734316384,16.4830954176946,44.457431791939));
#17769=CARTESIAN_POINT('',(44.458526568362,16.4830954176946,49.7699317919394));
#17770=CARTESIAN_POINT('',(44.458526568362,16.4830954176946,49.7699317919394));
#17771=CARTESIAN_POINT('Origin',(44.4585265683621,16.4830954176946,44.4574317919394));
#17772=CARTESIAN_POINT('',(-46.3550209176718,16.4830954176946,28.9646748425992));
#17773=CARTESIAN_POINT('',(-28.7987164822987,16.4830954176946,46.5209792779726));
#17774=CARTESIAN_POINT('Origin',(0.0835265683620477,16.4830954176946,0.0824317919394229));
#17775=CARTESIAN_POINT('',(-29.4588820377424,16.4830954176946,48.8324317919391));
#17776=CARTESIAN_POINT('Origin',(-29.4588820377423,16.4830954176946,47.5824317919391));
#17777=CARTESIAN_POINT('',(-39.9953087176173,16.4830954176946,48.832431791939));
#17778=CARTESIAN_POINT('',(-39.9953087176173,16.4830954176946,48.832431791939));
#17779=CARTESIAN_POINT('',(-41.0061710032694,16.4830954176946,46.8471376742919));
#17780=CARTESIAN_POINT('Origin',(-39.9953087176173,16.4830954176946,47.582431791939));
#17781=CARTESIAN_POINT('Origin',(-44.2914734316384,16.4830954176946,44.457431791939));
#17782=CARTESIAN_POINT('',(-48.6664734316382,16.4830954176946,29.6248403980428));
#17783=CARTESIAN_POINT('',(-48.6664734316382,16.4830954176946,29.6248403980428));
#17784=CARTESIAN_POINT('Origin',(-47.4164734316383,16.4830954176946,29.6248403980429));
#17785=CARTESIAN_POINT('',(28.9657696190224,16.4830954176946,-46.356115694094));
#17786=CARTESIAN_POINT('Origin',(0.0835265683620477,16.4830954176946,0.0824317919394229));
#17787=CARTESIAN_POINT('',(29.6259351744661,16.4830954176946,-48.6675682080605));
#17788=CARTESIAN_POINT('Origin',(29.6259351744661,16.4830954176946,-47.4175682080605));
#17789=CARTESIAN_POINT('',(40.1623618543411,16.4830954176946,-48.6675682080604));
#17790=CARTESIAN_POINT('',(40.1623618543411,16.4830954176946,-48.6675682080604));
#17791=CARTESIAN_POINT('Origin',(40.1623618543411,16.4830954176946,-47.4175682080604));
#17792=CARTESIAN_POINT('',(48.8335265683622,16.4830954176946,-39.9964034940393));
#17793=CARTESIAN_POINT('Origin',(47.5835265683622,16.4830954176946,-39.9964034940393));
#17794=CARTESIAN_POINT('',(48.8335265683621,16.4830954176946,-29.4599768141643));
#17795=CARTESIAN_POINT('',(-28.7987164822982,16.4830954176946,-46.3561156940941));
#17796=CARTESIAN_POINT('Origin',(0.0835265683620477,16.4830954176946,0.0824317919394229));
#17797=CARTESIAN_POINT('',(-48.6664734316379,16.4830954176946,-39.9964034940395));
#17798=CARTESIAN_POINT('',(-48.6664734316379,16.4830954176946,-39.9964034940395));
#17799=CARTESIAN_POINT('Origin',(-47.4164734316379,16.4830954176946,-39.9964034940395));
#17800=CARTESIAN_POINT('',(-39.9953087176169,16.4830954176946,-48.6675682080606));
#17801=CARTESIAN_POINT('Origin',(-39.9953087176169,16.4830954176946,-47.4175682080606));
#17802=CARTESIAN_POINT('',(-29.4588820377419,16.4830954176946,-48.6675682080606));
#17803=CARTESIAN_POINT('',(-29.4588820377419,16.4830954176946,-48.6675682080606));
#17804=CARTESIAN_POINT('Origin',(-29.4588820377419,16.4830954176946,-47.4175682080606));
#17805=CARTESIAN_POINT('',(48.6088737900632,16.4830954176946,22.7696071163714));
#17806=CARTESIAN_POINT('',(48.833526568362,16.4830954176946,21.5181263879131));
#17807=CARTESIAN_POINT('Ctrl Pts',(48.6088737900632,16.4830954176946,22.7696071163714));
#17808=CARTESIAN_POINT('Ctrl Pts',(48.6546862755533,16.4830954176946,22.6716193001842));
#17809=CARTESIAN_POINT('Ctrl Pts',(48.6897381335915,16.4830954176946,22.5688627245672));
#17810=CARTESIAN_POINT('Ctrl Pts',(48.746344156916,16.4830954176946,22.3629081987095));
#17811=CARTESIAN_POINT('Ctrl Pts',(48.7679585435476,16.4830954176946,22.258923921387));
#17812=CARTESIAN_POINT('Ctrl Pts',(48.8185384277345,16.4830954176946,21.9448236639213));
#17813=CARTESIAN_POINT('Ctrl Pts',(48.8335265683619,16.4830954176946,21.7326033051433));
#17814=CARTESIAN_POINT('Ctrl Pts',(48.833526568362,16.4830954176946,21.5181263879131));
#17815=CARTESIAN_POINT('',(22.7707018927938,16.4830954176946,48.6077790136406));
#17816=CARTESIAN_POINT('Origin',(0.0835265683620477,16.4830954176946,0.0824317919394229));
#17817=CARTESIAN_POINT('',(21.5192211643356,16.4830954176946,48.8324317919394));
#17818=CARTESIAN_POINT('Ctrl Pts',(21.5192211643356,16.4830954176946,48.8324317919394));
#17819=CARTESIAN_POINT('Ctrl Pts',(21.7332984919314,16.4830954176946,48.8324317919394));
#17820=CARTESIAN_POINT('Ctrl Pts',(21.9465891291831,16.4830954176946,48.8173905539921));
#17821=CARTESIAN_POINT('Ctrl Pts',(22.2609747321794,16.4830954176946,48.7666821942729));
#17822=CARTESIAN_POINT('Ctrl Pts',(22.3650002683796,16.4830954176946,48.745019785418));
#17823=CARTESIAN_POINT('Ctrl Pts',(22.570892003613,16.4830954176946,48.6883415841153));
#17824=CARTESIAN_POINT('Ctrl Pts',(22.6731778206313,16.4830954176946,48.6533746837426));
#17825=CARTESIAN_POINT('Ctrl Pts',(22.7707018927938,16.4830954176946,48.6077790136406));
#17826=CARTESIAN_POINT('',(-21.3521680276115,16.4830954176946,48.8324317919394));
#17827=CARTESIAN_POINT('',(-44.291473431638,16.4830954176946,48.8324317919394));
#17828=CARTESIAN_POINT('',(-22.6036487560697,16.4830954176946,48.6077790136406));
#17829=CARTESIAN_POINT('Ctrl Pts',(-22.6036487560697,16.4830954176946,48.6077790136407));
#17830=CARTESIAN_POINT('Ctrl Pts',(-22.5442911026821,16.4830954176946,48.6355306057096));
#17831=CARTESIAN_POINT('Ctrl Pts',(-22.483475353007,16.4830954176946,48.6595286545756));
#17832=CARTESIAN_POINT('Ctrl Pts',(-22.4216836912354,16.4830954176946,48.680466078412));
#17833=CARTESIAN_POINT('Ctrl Pts',(-22.3548812712597,16.4830954176946,48.7031013424626));
#17834=CARTESIAN_POINT('Ctrl Pts',(-22.2869375438441,16.4830954176946,48.7221589140917));
#17835=CARTESIAN_POINT('Ctrl Pts',(-22.2184316516974,16.4830954176945,48.7384583526655));
#17836=CARTESIAN_POINT('Ctrl Pts',(-22.1424085678882,16.4830954176944,48.756546338179));
#17837=CARTESIAN_POINT('Ctrl Pts',(-22.0656917788855,16.4830954176943,48.7712365700779));
#17838=CARTESIAN_POINT('Ctrl Pts',(-21.9890537694626,16.483095417693,48.783595693684));
#17839=CARTESIAN_POINT('Ctrl Pts',(-21.988813152617,16.483095417693,48.7836344970579));
#17840=CARTESIAN_POINT('Ctrl Pts',(-21.9885725320674,16.483095417693,48.7836732756889));
#17841=CARTESIAN_POINT('Ctrl Pts',(-21.9883319078107,16.483095417693,48.7837120295832));
#17842=CARTESIAN_POINT('Ctrl Pts',(-21.7932700913188,16.4830954176898,48.8151278358004));
#17843=CARTESIAN_POINT('Ctrl Pts',(-21.5961370769475,16.4830954176946,48.8302373326079));
#17844=CARTESIAN_POINT('Ctrl Pts',(-21.3973353133493,16.4830954176946,48.8322086727425));
#17845=CARTESIAN_POINT('Ctrl Pts',(-21.3822890539765,16.4830954176946,48.8323578731039));
#17846=CARTESIAN_POINT('Ctrl Pts',(-21.3672332341099,16.4830954176946,48.8324317919394));
#17847=CARTESIAN_POINT('Ctrl Pts',(-21.3521680276115,16.4830954176946,48.8324317919394));
#17848=CARTESIAN_POINT('',(-48.4418206533391,16.4830954176946,22.7696071163712));
#17849=CARTESIAN_POINT('Origin',(0.0835265683620477,16.4830954176946,0.0824317919394229));
#17850=CARTESIAN_POINT('',(-48.6664734316379,16.4830954176946,21.5181263879129));
#17851=CARTESIAN_POINT('Ctrl Pts',(-48.6664734316379,16.4830954176946,21.5181263879129));
#17852=CARTESIAN_POINT('Ctrl Pts',(-48.6664734316379,16.4830954176946,21.6670631867632));
#17853=CARTESIAN_POINT('Ctrl Pts',(-48.6591650713411,16.4830954176948,21.8157113579154));
#17854=CARTESIAN_POINT('Ctrl Pts',(-48.6433862740522,16.4830954176944,21.9626800039502));
#17855=CARTESIAN_POINT('Ctrl Pts',(-48.6364163282529,16.4830954176942,22.0276002560013));
#17856=CARTESIAN_POINT('Ctrl Pts',(-48.6277942051812,16.4830954176938,22.0921928653205));
#17857=CARTESIAN_POINT('Ctrl Pts',(-48.6174230355526,16.4830954176928,22.1563387307969));
#17858=CARTESIAN_POINT('Ctrl Pts',(-48.617413607667,16.4830954176928,22.1563970424342));
#17859=CARTESIAN_POINT('Ctrl Pts',(-48.6174041785652,16.4830954176928,22.1564553538403));
#17860=CARTESIAN_POINT('Ctrl Pts',(-48.6173947482465,16.4830954176928,22.1565136650151));
#17861=CARTESIAN_POINT('Ctrl Pts',(-48.6004607795326,16.4830954176911,22.2612227048913));
#17862=CARTESIAN_POINT('Ctrl Pts',(-48.5796176356208,16.4830954176926,22.3651301096173));
#17863=CARTESIAN_POINT('Ctrl Pts',(-48.5514944830101,16.4830954176936,22.4675457567853));
#17864=CARTESIAN_POINT('Ctrl Pts',(-48.5306835096382,16.4830954176943,22.5433327546222));
#17865=CARTESIAN_POINT('Ctrl Pts',(-48.5058864570286,16.4830954176946,22.6183030588211));
#17866=CARTESIAN_POINT('Ctrl Pts',(-48.4756998063479,16.4830954176946,22.6921687122293));
#17867=CARTESIAN_POINT('Ctrl Pts',(-48.4650933730757,16.4830954176946,22.7181222746919));
#17868=CARTESIAN_POINT('Ctrl Pts',(-48.4538211421634,16.4830954176946,22.7439393637239));
#17869=CARTESIAN_POINT('Ctrl Pts',(-48.4418206533392,16.4830954176946,22.7696071163711));
#17870=CARTESIAN_POINT('',(-48.6664734316379,16.4830954176946,-21.3532628040342));
#17871=CARTESIAN_POINT('',(-48.6664734316379,16.4830954176946,-44.2925682080606));
#17872=CARTESIAN_POINT('',(-48.4418206533391,16.4830954176946,-22.6047435324924));
#17873=CARTESIAN_POINT('Ctrl Pts',(-48.4418206533392,16.4830954176946,-22.6047435324923));
#17874=CARTESIAN_POINT('Ctrl Pts',(-48.4698886928407,16.4830954176946,-22.5447090321936));
#17875=CARTESIAN_POINT('Ctrl Pts',(-48.4941170616729,16.4830954176946,-22.4831875953525));
#17876=CARTESIAN_POINT('Ctrl Pts',(-48.5152210475791,16.4830954176946,-22.4206776899558));
#17877=CARTESIAN_POINT('Ctrl Pts',(-48.5380549774177,16.4830954176946,-22.3530436988988));
#17878=CARTESIAN_POINT('Ctrl Pts',(-48.5572307441801,16.4830954176946,-22.2842518491799));
#17879=CARTESIAN_POINT('Ctrl Pts',(-48.5735983779025,16.4830954176945,-22.2149034817008));
#17880=CARTESIAN_POINT('Ctrl Pts',(-48.5911862340032,16.4830954176944,-22.1403851286675));
#17881=CARTESIAN_POINT('Ctrl Pts',(-48.6055304232494,16.4830954176942,-22.0652228656951));
#17882=CARTESIAN_POINT('Ctrl Pts',(-48.6176377678211,16.4830954176929,-21.9901456057825));
#17883=CARTESIAN_POINT('Ctrl Pts',(-48.6176781949277,16.4830954176929,-21.9898949185755));
#17884=CARTESIAN_POINT('Ctrl Pts',(-48.6177185951685,16.4830954176929,-21.9896442273897));
#17885=CARTESIAN_POINT('Ctrl Pts',(-48.6177589685505,16.4830954176929,-21.9893935322219));
#17886=CARTESIAN_POINT('Ctrl Pts',(-48.6490360664948,16.4830954176895,-21.7951809860257));
#17887=CARTESIAN_POINT('Ctrl Pts',(-48.6641532259573,16.4830954176946,-21.5988820000785));
#17888=CARTESIAN_POINT('Ctrl Pts',(-48.6662251385255,16.4830954176946,-21.4008987475353));
#17889=CARTESIAN_POINT('Ctrl Pts',(-48.6663911974825,16.4830954176946,-21.3850308518833));
#17890=CARTESIAN_POINT('Ctrl Pts',(-48.6664734316364,16.4830954176946,-21.369152135278));
#17891=CARTESIAN_POINT('Ctrl Pts',(-48.6664734316379,16.4830954176946,-21.3532628040342));
#17892=CARTESIAN_POINT('',(-22.6036487560697,16.4830954176946,-48.4429154297618));
#17893=CARTESIAN_POINT('Origin',(0.0835265683620477,16.4830954176946,0.0824317919394229));
#17894=CARTESIAN_POINT('',(-21.3521680276115,16.4830954176946,-48.6675682080606));
#17895=CARTESIAN_POINT('Ctrl Pts',(-21.3521680276115,16.4830954176946,-48.6675682080606));
#17896=CARTESIAN_POINT('Ctrl Pts',(-21.5662453552073,16.4830954176946,-48.6675682080605));
#17897=CARTESIAN_POINT('Ctrl Pts',(-21.779535992459,16.4830954176946,-48.6525269701133));
#17898=CARTESIAN_POINT('Ctrl Pts',(-22.0939215954554,16.4830954176946,-48.601818610394));
#17899=CARTESIAN_POINT('Ctrl Pts',(-22.1979471316555,16.4830954176946,-48.5801562015391));
#17900=CARTESIAN_POINT('Ctrl Pts',(-22.4038388668889,16.4830954176946,-48.5234780002364));
#17901=CARTESIAN_POINT('Ctrl Pts',(-22.5061246839072,16.4830954176946,-48.4885110998637));
#17902=CARTESIAN_POINT('Ctrl Pts',(-22.6036487560697,16.4830954176946,-48.4429154297618));
#17903=CARTESIAN_POINT('',(21.5192211643356,16.4830954176946,-48.6675682080606));
#17904=CARTESIAN_POINT('',(-44.291473431638,16.4830954176946,-48.6675682080606));
#17905=CARTESIAN_POINT('',(22.7707018927938,16.4830954176946,-48.4429154297618));
#17906=CARTESIAN_POINT('Ctrl Pts',(22.7707018927938,16.4830954176946,-48.4429154297618));
#17907=CARTESIAN_POINT('Ctrl Pts',(22.7113442394013,16.4830954176946,-48.4706670218339));
#17908=CARTESIAN_POINT('Ctrl Pts',(22.6505284897208,16.4830954176946,-48.4946650707021));
#17909=CARTESIAN_POINT('Ctrl Pts',(22.5887368279435,16.4830954176946,-48.5156024945398));
#17910=CARTESIAN_POINT('Ctrl Pts',(22.5219344079612,16.4830954176946,-48.5382377585921));
#17911=CARTESIAN_POINT('Ctrl Pts',(22.4539906805388,16.4830954176946,-48.5572953302219));
#17912=CARTESIAN_POINT('Ctrl Pts',(22.3854847883852,16.4830954176945,-48.573594768796));
#17913=CARTESIAN_POINT('Ctrl Pts',(22.3094617045878,16.4830954176944,-48.5916827543053));
#17914=CARTESIAN_POINT('Ctrl Pts',(22.2327449155974,16.4830954176943,-48.6063729862011));
#17915=CARTESIAN_POINT('Ctrl Pts',(22.1561069061867,16.483095417693,-48.6187321098052));
#17916=CARTESIAN_POINT('Ctrl Pts',(22.1558662893411,16.483095417693,-48.6187709131791));
#17917=CARTESIAN_POINT('Ctrl Pts',(22.1556256687915,16.483095417693,-48.6188096918101));
#17918=CARTESIAN_POINT('Ctrl Pts',(22.1553850445348,16.483095417693,-48.6188484457044));
#17919=CARTESIAN_POINT('Ctrl Pts',(21.960323227055,16.4830954176898,-48.6502642520806));
#17920=CARTESIAN_POINT('Ctrl Pts',(21.763190211675,16.4830954176946,-48.6653737488822));
#17921=CARTESIAN_POINT('Ctrl Pts',(21.5643884470531,16.4830954176946,-48.6673450888936));
#17922=CARTESIAN_POINT('Ctrl Pts',(21.5493421886858,16.4830954176946,-48.667494289235));
#17923=CARTESIAN_POINT('Ctrl Pts',(21.534286369826,16.4830954176946,-48.6675682080606));
#17924=CARTESIAN_POINT('Ctrl Pts',(21.5192211643356,16.4830954176946,-48.6675682080606));
#17925=CARTESIAN_POINT('',(48.6088737900633,16.4830954176946,-22.6047435324922));
#17926=CARTESIAN_POINT('Origin',(0.0835265683620477,16.4830954176946,0.0824317919394229));
#17927=CARTESIAN_POINT('',(48.8335265683621,16.4830954176946,-21.353262804034));
#17928=CARTESIAN_POINT('Ctrl Pts',(48.8335265683621,16.4830954176946,-21.353262804034));
#17929=CARTESIAN_POINT('Ctrl Pts',(48.8335265683621,16.4830954176946,-21.5205271356));
#17930=CARTESIAN_POINT('Ctrl Pts',(48.8242872408348,16.4830954176954,-21.6876151718335));
#17931=CARTESIAN_POINT('Ctrl Pts',(48.8041808326122,16.4830954176937,-21.8523364174683));
#17932=CARTESIAN_POINT('Ctrl Pts',(48.798489466322,16.4830954176932,-21.8989627932144));
#17933=CARTESIAN_POINT('Ctrl Pts',(48.7919270859958,16.4830954176924,-21.9453996267745));
#17934=CARTESIAN_POINT('Ctrl Pts',(48.7844559810354,16.483095417691,-21.9915973363727));
#17935=CARTESIAN_POINT('Ctrl Pts',(48.7844427023226,16.483095417691,-21.9916794455283));
#17936=CARTESIAN_POINT('Ctrl Pts',(48.7844294211923,16.483095417691,-21.991761554233));
#17937=CARTESIAN_POINT('Ctrl Pts',(48.7844161376429,16.483095417691,-21.9918436624863));
#17938=CARTESIAN_POINT('Ctrl Pts',(48.7674708494511,16.4830954176877,-22.0965858496438));
#17939=CARTESIAN_POINT('Ctrl Pts',(48.7466093475409,16.4830954176906,-22.2005030769087));
#17940=CARTESIAN_POINT('Ctrl Pts',(48.7184834265343,16.4830954176926,-22.3028911433133));
#17941=CARTESIAN_POINT('Ctrl Pts',(48.6974913278267,16.4830954176941,-22.3793096327179));
#17942=CARTESIAN_POINT('Ctrl Pts',(48.672452993622,16.4830954176945,-22.454876484413));
#17943=CARTESIAN_POINT('Ctrl Pts',(48.6419388604506,16.4830954176946,-22.5292903869264));
#17944=CARTESIAN_POINT('Ctrl Pts',(48.6315691300731,16.4830954176946,-22.5545787377723));
#17945=CARTESIAN_POINT('Ctrl Pts',(48.6205666139332,16.4830954176946,-22.5797338420621));
#17946=CARTESIAN_POINT('Ctrl Pts',(48.6088737900634,16.4830954176946,-22.6047435324921));
#17947=CARTESIAN_POINT('',(48.8335265683622,16.4830954176946,-44.2925682080603));
#17948=CARTESIAN_POINT('Origin',(50.0835265683621,16.4830954176946,0.0824317919395974));
#17949=CARTESIAN_POINT('',(50.0835265683619,-8.87385981233827,37.6072170232579));
#17950=CARTESIAN_POINT('',(50.0835265683619,-14.4544045823054,37.6072170232579));
#17951=CARTESIAN_POINT('',(50.0835265683619,16.4830954176946,37.6072170232579));
#17952=CARTESIAN_POINT('',(50.0835265683621,-8.87385981233827,44.4574317919394));
#17953=CARTESIAN_POINT('',(50.0835265683621,-8.87385981233827,0.0824317919395974));
#17954=CARTESIAN_POINT('',(50.0835265683621,-14.4544045823054,44.4574317919394));
#17955=CARTESIAN_POINT('',(50.0835265683621,16.4830954176946,44.4574317919394));
#17956=CARTESIAN_POINT('',(50.0835265683621,-14.4544045823054,0.0824317919395974));
#17957=CARTESIAN_POINT('Origin',(50.0835265683621,16.4830954176946,0.0824317919395974));
#17958=CARTESIAN_POINT('',(50.0835265683619,16.1705954176946,37.6072170232579));
#17959=CARTESIAN_POINT('',(50.0835265683619,13.4386401876617,37.6072170232579));
#17960=CARTESIAN_POINT('',(50.0835265683619,16.4830954176946,37.6072170232579));
#17961=CARTESIAN_POINT('',(50.0835265683621,16.1705954176946,44.4574317919394));
#17962=CARTESIAN_POINT('',(50.0835265683619,16.1705954176946,44.4574317919394));
#17963=CARTESIAN_POINT('',(50.0835265683621,13.4386401876617,44.4574317919394));
#17964=CARTESIAN_POINT('',(50.0835265683621,16.4830954176946,44.4574317919394));
#17965=CARTESIAN_POINT('',(50.0835265683621,13.4386401876617,0.0824317919395974));
#17966=CARTESIAN_POINT('Origin',(68.5210265683621,-8.56135981233827,0.0824317919394229));
#17967=CARTESIAN_POINT('',(46.9585265683621,-8.56135981233827,38.3884670232579));
#17968=CARTESIAN_POINT('',(46.9585265683621,-8.56135981233827,36.5987899438301));
#17969=CARTESIAN_POINT('',(46.9585265683619,-8.56135981233827,0.0824317919394977));
#17970=CARTESIAN_POINT('',(44.4818701996542,-8.56135981233827,35.7821111511702));
#17971=CARTESIAN_POINT('',(46.9585265683621,-8.56135981233827,36.5987899438301));
#17972=CARTESIAN_POINT('',(45.272154845105,-8.56135981233827,33.3854975524836));
#17973=CARTESIAN_POINT('',(44.4818701996542,-8.56135981233827,35.7821111511702));
#17974=CARTESIAN_POINT('',(48.8335265683621,-8.56135981233827,34.5598618267976));
#17975=CARTESIAN_POINT('',(45.272154845105,-8.56135981233827,33.3854975524836));
#17976=CARTESIAN_POINT('',(48.8335265683621,-8.56135981233827,36.6697170232579));
#17977=CARTESIAN_POINT('',(48.8335265683619,-8.56135981233827,0.0824317919394912));
#17978=CARTESIAN_POINT('',(49.7710265683619,-8.56135981233827,36.6697170232579));
#17979=CARTESIAN_POINT('',(68.5210265683621,-8.56135981233827,36.6697170232579));
#17980=CARTESIAN_POINT('',(49.771026568362,-8.56135981233827,22.7876789472104));
#17981=CARTESIAN_POINT('',(49.7710265683621,-8.56135981233827,0.0824317919393611));
#17982=CARTESIAN_POINT('',(39.5861451654569,-8.56135981233827,37.8172834360679));
#17983=CARTESIAN_POINT('Origin',(0.0835265683620477,-8.56135981233827,0.0824317919394229));
#17984=CARTESIAN_POINT('',(40.7421664865885,-8.56135981233827,38.9733047571995));
#17985=CARTESIAN_POINT('',(40.7421664865885,-8.56135981233827,38.9733047571995));
#17986=CARTESIAN_POINT('',(38.9743995336222,-8.56135981233827,40.7410717101659));
#17987=CARTESIAN_POINT('Origin',(39.8582830101054,-8.56135981233827,39.8571882336827));
#17988=CARTESIAN_POINT('',(37.8183782124906,-8.56135981233827,39.5850503890343));
#17989=CARTESIAN_POINT('',(37.7312605880988,-8.56135981233827,39.4979327646425));
#17990=CARTESIAN_POINT('',(22.7887737236329,-8.56135981233827,49.7699317919394));
#17991=CARTESIAN_POINT('Origin',(0.0835265683620477,-8.56135981233827,0.0824317919394229));
#17992=CARTESIAN_POINT('',(44.458526568362,-8.56135981233827,49.7699317919394));
#17993=CARTESIAN_POINT('',(68.5210265683621,-8.56135981233827,49.7699317919394));
#17994=CARTESIAN_POINT('',(49.7710265683619,-8.56135981233827,44.4574317919394));
#17995=CARTESIAN_POINT('Origin',(44.4585265683621,-8.56135981233827,44.4574317919394));
#17996=CARTESIAN_POINT('',(49.7710265683619,-8.56135981233827,37.6072170232579));
#17997=CARTESIAN_POINT('',(49.7710265683621,-8.56135981233827,0.0824317919393611));
#17998=CARTESIAN_POINT('',(48.8335265683621,-8.56135981233827,37.6072170232579));
#17999=CARTESIAN_POINT('',(68.5210265683621,-8.56135981233827,37.6072170232579));
#18000=CARTESIAN_POINT('',(48.8335265683621,-8.56135981233827,38.3884670232579));
#18001=CARTESIAN_POINT('',(48.8335265683619,-8.56135981233827,0.0824317919394912));
#18002=CARTESIAN_POINT('',(68.5210265683621,-8.56135981233827,38.3884670232579));
#18003=CARTESIAN_POINT('Origin',(50.833526568362,13.1261401876617,0.0824317919394229));
#18004=CARTESIAN_POINT('',(49.771026568362,13.1261401876617,37.6072170232579));
#18005=CARTESIAN_POINT('',(48.8335265683621,13.1261401876617,37.6072170232579));
#18006=CARTESIAN_POINT('',(50.833526568362,13.1261401876617,37.6072170232579));
#18007=CARTESIAN_POINT('',(49.7710265683619,13.1261401876617,44.4574317919394));
#18008=CARTESIAN_POINT('',(49.7710265683621,13.1261401876617,0.0824317919394194));
#18009=CARTESIAN_POINT('',(44.458526568362,13.1261401876617,49.7699317919394));
#18010=CARTESIAN_POINT('Origin',(44.4585265683621,13.1261401876617,44.4574317919394));
#18011=CARTESIAN_POINT('',(11.0320394968433,13.1261401876617,49.7699317919394));
#18012=CARTESIAN_POINT('',(50.8335265683621,13.1261401876617,49.7699317919394));
#18013=CARTESIAN_POINT('',(35.1659821576993,13.1261401876617,36.932654334243));
#18014=CARTESIAN_POINT('Origin',(0.0835265683620477,13.1261401876617,0.0824317919394229));
#18015=CARTESIAN_POINT('',(38.9743995336222,13.1261401876617,40.7410717101659));
#18016=CARTESIAN_POINT('',(36.9337491106657,13.1261401876617,35.1648873812767));
#18017=CARTESIAN_POINT('',(36.846955706336,13.1261401876617,35.078093976947));
#18018=CARTESIAN_POINT('',(49.771026568362,13.1261401876617,11.0309447204208));
#18019=CARTESIAN_POINT('Origin',(0.0835265683620477,13.1261401876617,0.0824317919394229));
#18020=CARTESIAN_POINT('',(49.771026568362,13.1261401876617,36.6697170232579));
#18021=CARTESIAN_POINT('',(49.7710265683621,13.1261401876617,0.0824317919394194));
#18022=CARTESIAN_POINT('',(48.8335265683621,13.1261401876617,36.6697170232579));
#18023=CARTESIAN_POINT('',(50.833526568362,13.1261401876617,36.6697170232579));
#18024=CARTESIAN_POINT('',(48.8335265683621,13.1261401876617,35.8884670232579));
#18025=CARTESIAN_POINT('',(48.8335265683619,13.1261401876617,0.0824317919394298));
#18026=CARTESIAN_POINT('',(46.958526568362,13.1261401876617,35.8884670232579));
#18027=CARTESIAN_POINT('',(50.833526568362,13.1261401876617,35.8884670232579));
#18028=CARTESIAN_POINT('',(46.9585265683621,13.1261401876617,38.3884670232579));
#18029=CARTESIAN_POINT('',(46.9585265683619,13.1261401876617,0.0824317919394363));
#18030=CARTESIAN_POINT('',(48.8335265683621,13.1261401876617,38.3884670232579));
#18031=CARTESIAN_POINT('',(50.833526568362,13.1261401876617,38.3884670232579));
#18032=CARTESIAN_POINT('',(48.8335265683619,13.1261401876617,0.0824317919394298));
#18033=CARTESIAN_POINT('Origin',(48.5210265683621,15.5455954176946,42.8336341598436));
#18034=CARTESIAN_POINT('',(48.5210265683621,15.8580954176946,38.3884670232579));
#18035=CARTESIAN_POINT('',(48.5210265683621,16.1705954176946,38.3884670232579));
#18036=CARTESIAN_POINT('',(48.5210265683621,15.5455954176946,38.3884670232579));
#18037=CARTESIAN_POINT('',(48.5210265683621,15.8580954176946,42.8336341598436));
#18038=CARTESIAN_POINT('',(48.5210265683621,16.4830954176946,40.1612670779183));
#18039=CARTESIAN_POINT('',(48.5210265683621,16.1705954176946,29.6248403980433));
#18040=CARTESIAN_POINT('Origin',(49.7710265683621,13.4386401876617,0.0824317919395964));
#18041=CARTESIAN_POINT('Origin',(49.7710265683619,13.4386401876617,37.6072170232579));
#18042=CARTESIAN_POINT('Origin',(49.7710265683619,13.4386401876617,44.4574317919394));
#18043=CARTESIAN_POINT('Origin',(49.7710265683621,-8.87385981233827,0.0824317919395964));
#18044=CARTESIAN_POINT('Origin',(49.7710265683619,-8.87385981233827,37.6072170232579));
#18045=CARTESIAN_POINT('Origin',(49.7710265683619,-8.87385981233827,44.4574317919394));
#18046=CARTESIAN_POINT('Origin',(49.7710265683621,-14.4544045823054,0.0824317919395964));
#18047=CARTESIAN_POINT('',(49.7710265683619,-14.7669045823054,37.6072170232579));
#18048=CARTESIAN_POINT('',(49.7710265683619,-14.7669045823054,44.4574317919394));
#18049=CARTESIAN_POINT('',(49.7710265683622,-14.7669045823054,-44.2925682080603));
#18050=CARTESIAN_POINT('Origin',(49.7710265683619,-14.4544045823054,37.6072170232579));
#18051=CARTESIAN_POINT('Origin',(49.7710265683619,-14.4544045823054,44.4574317919394));
#18052=CARTESIAN_POINT('Origin',(49.7710265683622,16.1705954176946,-44.2925682080603));
#18053=CARTESIAN_POINT('Origin',(49.7710265683619,16.1705954176946,37.6072170232579));
#18054=CARTESIAN_POINT('Origin',(49.7710265683619,16.1705954176946,44.4574317919394));
#18055=CARTESIAN_POINT('Origin',(48.8335265683621,16.1705954176946,42.8336341598436));
#18056=CARTESIAN_POINT('Origin',(48.8335265683621,16.1705954176946,38.3884670232579));
#18057=CARTESIAN_POINT('Origin',(48.2085265683621,15.8580954176946,0.0824317919394229));
#18058=CARTESIAN_POINT('',(48.2085265683621,15.5455954176946,38.3884670232579));
#18059=CARTESIAN_POINT('Origin',(48.2085265683621,15.8580954176946,38.3884670232579));
#18060=CARTESIAN_POINT('',(48.2085265683621,15.5455954176946,0.0824317919394229));
#18061=CARTESIAN_POINT('Origin',(-4.89277133898972,-11.0169045823054,15.1735300494181));
#18062=CARTESIAN_POINT('',(10.111699809421,-11.3294045823054,20.1212626201575));
#18063=CARTESIAN_POINT('',(15.8818970466764,-11.3294045823054,22.02398831625));
#18064=CARTESIAN_POINT('',(-4.89277133898972,-11.3294045823054,15.1735300494181));
#18065=CARTESIAN_POINT('',(15.8818970466764,-14.4544045823054,22.02398831625));
#18066=CARTESIAN_POINT('',(15.8818970466764,-11.0169045823054,22.02398831625));
#18067=CARTESIAN_POINT('',(10.111699809421,-14.4544045823054,20.1212626201575));
#18068=CARTESIAN_POINT('',(-4.89277133898972,-14.4544045823054,15.1735300494181));
#18069=CARTESIAN_POINT('',(10.111699809421,-11.0169045823054,20.1212626201575));
#18070=CARTESIAN_POINT('Origin',(-4.99063502851588,-14.4544045823054,15.4703110263562));
#18071=CARTESIAN_POINT('',(15.7840333571502,-14.7669045823054,22.3207692931881));
#18072=CARTESIAN_POINT('Origin',(15.7840333571502,-14.4544045823054,22.3207692931881));
#18073=CARTESIAN_POINT('',(10.0138361198949,-14.7669045823054,20.4180435970956));
#18074=CARTESIAN_POINT('',(-58.2113397045057,-14.7669045823054,-2.07924545974433));
#18075=CARTESIAN_POINT('Origin',(10.0138361198949,-14.4544045823054,20.4180435970956));
#18076=CARTESIAN_POINT('Origin',(-4.99063502851588,-11.3294045823054,15.4703110263562));
#18077=CARTESIAN_POINT('',(15.7840333571502,-11.0169045823054,22.3207692931881));
#18078=CARTESIAN_POINT('Origin',(15.7840333571502,-11.3294045823054,22.3207692931881));
#18079=CARTESIAN_POINT('',(10.0138361198949,-11.0169045823054,20.4180435970956));
#18080=CARTESIAN_POINT('Origin',(10.0138361198949,-11.3294045823054,20.4180435970956));
#18081=CARTESIAN_POINT('',(-4.99063502851588,-11.0169045823054,15.4703110263562));
#18082=CARTESIAN_POINT('Origin',(0.0835265683620477,-12.5794045823054,0.0824317919394229));
#18083=CARTESIAN_POINT('',(15.3925785990455,-12.5794045823054,23.5078932009404));
#18084=CARTESIAN_POINT('',(7.67510093260532,-12.5794045823054,20.9630507178886));
#18085=CARTESIAN_POINT('',(-5.38208978662056,-12.5794045823054,16.6574349341085));
#18086=CARTESIAN_POINT('',(7.59696574233659,-12.5794045823054,18.6174859267129));
#18087=CARTESIAN_POINT('Origin',(8.06655569071,-12.5794045823054,19.7759268101363));
#18088=CARTESIAN_POINT('',(-6.17974956131282,-12.5794045823054,19.076414315977));
#18089=CARTESIAN_POINT('Origin',(0.0835265683620477,-12.5794045823054,0.0824317919394229));
#18090=CARTESIAN_POINT('',(14.5949188243533,-12.5794045823054,25.9268725828089));
#18091=CARTESIAN_POINT('',(-6.17974956131282,-12.5794045823054,19.076414315977));
#18092=CARTESIAN_POINT('',(20.8581949540281,-12.5794045823054,6.93289005877128));
#18093=CARTESIAN_POINT('Origin',(0.083526568362047,-85.4775827009602,-48.3550682080606));
#18094=CARTESIAN_POINT('',(0.0835265683620966,-6.14692278878557,-48.3550682080606));
#18095=CARTESIAN_POINT('',(4.28505819640517,-6.32940458230551,-48.3550682080606));
#18096=CARTESIAN_POINT('Origin',(0.0819794890372154,-78.8840761885053,-48.3550682139743));
#18097=CARTESIAN_POINT('',(-4.11800505968097,-6.32940458230551,-48.3550682080606));
#18098=CARTESIAN_POINT('Origin',(0.0850736528295037,-78.8840761674478,-48.3550682141158));
#18099=CARTESIAN_POINT('',(-29.3897661934246,-14.4544067125512,-48.3550682080518));
#18100=CARTESIAN_POINT('Ctrl Pts',(-4.11800505968098,-6.32940458230551,
-48.3550682080575));
#18101=CARTESIAN_POINT('Ctrl Pts',(-7.23028203564418,-6.60009089469845,
-48.355068207831));
#18102=CARTESIAN_POINT('Ctrl Pts',(-10.2832623655178,-7.16548762139643,
-48.3550682009245));
#18103=CARTESIAN_POINT('Ctrl Pts',(-13.2881929703542,-7.96970396804477,
-48.3550682035663));
#18104=CARTESIAN_POINT('Ctrl Pts',(-14.5634332304672,-8.310999391452,-48.3550682046874));
#18105=CARTESIAN_POINT('Ctrl Pts',(-15.8300197329982,-8.69530573227847,
-48.3550682067606));
#18106=CARTESIAN_POINT('Ctrl Pts',(-17.0888126926591,-9.1183486423787,-48.3550682076745));
#18107=CARTESIAN_POINT('Ctrl Pts',(-17.2519209468127,-9.17316448001821,
-48.3550682077929));
#18108=CARTESIAN_POINT('Ctrl Pts',(-17.4148784256617,-9.22862227451152,
-48.3550682078197));
#18109=CARTESIAN_POINT('Ctrl Pts',(-17.5776977494185,-9.28471651645609,
-48.3550682078142));
#18110=CARTESIAN_POINT('Ctrl Pts',(-18.1582353086448,-9.48472234840386,
-48.3550682077949));
#18111=CARTESIAN_POINT('Ctrl Pts',(-18.7377862785179,-9.69311870418431,
-48.3550682069701));
#18112=CARTESIAN_POINT('Ctrl Pts',(-19.3151335384121,-9.9089582081689,-48.3550682065996));
#18113=CARTESIAN_POINT('Ctrl Pts',(-19.6244384053913,-10.0245908849067,
-48.3550682064011));
#18114=CARTESIAN_POINT('Ctrl Pts',(-19.9331105403827,-10.1423607380609,
-48.3550682065513));
#18115=CARTESIAN_POINT('Ctrl Pts',(-20.2409594146601,-10.2621272193483,
-48.3550682071088));
#18116=CARTESIAN_POINT('Ctrl Pts',(-20.4551588435133,-10.3454600297986,
-48.3550682074966));
#18117=CARTESIAN_POINT('Ctrl Pts',(-20.6689790522681,-10.4297627624244,
-48.3550682076939));
#18118=CARTESIAN_POINT('Ctrl Pts',(-20.8823303370506,-10.5149781806565,
-48.355068207817));
#18119=CARTESIAN_POINT('Ctrl Pts',(-21.7084873705318,-10.8449565878889,
-48.3550682082937));
#18120=CARTESIAN_POINT('Ctrl Pts',(-22.5282779369094,-11.1887405793905,
-48.3550682080817));
#18121=CARTESIAN_POINT('Ctrl Pts',(-23.3424573486984,-11.5450903892485,
-48.3550682080254));
#18122=CARTESIAN_POINT('Ctrl Pts',(-23.6003183388764,-11.6579509129724,
-48.3550682080076));
#18123=CARTESIAN_POINT('Ctrl Pts',(-23.8576082226002,-11.7720687209439,
-48.3550682079892));
#18124=CARTESIAN_POINT('Ctrl Pts',(-24.1143473570555,-11.8874012527357,
-48.355068207977));
#18125=CARTESIAN_POINT('Ctrl Pts',(-25.0059583796815,-12.2879313738297,
-48.3550682079346));
#18126=CARTESIAN_POINT('Ctrl Pts',(-25.8909652612289,-12.70304390055,-48.3550682079832));
#18127=CARTESIAN_POINT('Ctrl Pts',(-26.7699903573938,-13.1313454185227,
-48.3550682080198));
#18128=CARTESIAN_POINT('Ctrl Pts',(-27.6490154535586,-13.5596469364954,
-48.3550682080564));
#18129=CARTESIAN_POINT('Ctrl Pts',(-28.5220589757606,-14.0011371004764,
-48.3550682080606));
#18130=CARTESIAN_POINT('Ctrl Pts',(-29.3897729325326,-14.4543739218821,
-48.3550682080606));
#18131=CARTESIAN_POINT('',(29.5568215162337,-14.4544045823054,-48.3550682080606));
#18132=CARTESIAN_POINT('',(30.4844928359005,-14.4544045823054,-48.3550682080606));
#18133=CARTESIAN_POINT('Ctrl Pts',(29.5568262308554,-14.4543736123985,-48.3550682080606));
#18134=CARTESIAN_POINT('Ctrl Pts',(28.6887755859948,-14.0009603589244,-48.3550682080606));
#18135=CARTESIAN_POINT('Ctrl Pts',(27.8153643667776,-13.5592886344723,-48.3550682080563));
#18136=CARTESIAN_POINT('Ctrl Pts',(26.9359347762758,-13.1308037218343,-48.3550682080188));
#18137=CARTESIAN_POINT('Ctrl Pts',(26.056505185774,-12.7023188091962,-48.3550682079813));
#18138=CARTESIAN_POINT('Ctrl Pts',(25.1710570057786,-12.2870210611749,-48.3550682079315));
#18139=CARTESIAN_POINT('Ctrl Pts',(24.2789629867541,-11.8863062114338,-48.3550682079749));
#18140=CARTESIAN_POINT('Ctrl Pts',(24.0216212267556,-11.7707122689897,-48.3550682079874));
#18141=CARTESIAN_POINT('Ctrl Pts',(23.7637232181357,-11.6563375248582,-48.3550682080063));
#18142=CARTESIAN_POINT('Ctrl Pts',(23.5052482767864,-11.5432249100067,-48.3550682080246));
#18143=CARTESIAN_POINT('Ctrl Pts',(22.7812340028694,-11.2263851139127,-48.3550682080758));
#18144=CARTESIAN_POINT('Ctrl Pts',(22.0529935081657,-10.9195690669471,-48.3550682081345));
#18145=CARTESIAN_POINT('Ctrl Pts',(21.3194160810682,-10.6234156296954,-48.3550682079765));
#18146=CARTESIAN_POINT('Ctrl Pts',(21.2279594902917,-10.5864935779565,-48.3550682079568));
#18147=CARTESIAN_POINT('Ctrl Pts',(21.1364199114277,-10.5497373133991,-48.3550682079309));
#18148=CARTESIAN_POINT('Ctrl Pts',(21.044795160316,-10.5131481250887,-48.3550682078952));
#18149=CARTESIAN_POINT('Ctrl Pts',(20.8306342211836,-10.4276256561536,-48.3550682078117));
#18150=CARTESIAN_POINT('Ctrl Pts',(20.6160433656434,-10.343038687593,-48.3550682076774));
#18151=CARTESIAN_POINT('Ctrl Pts',(20.4010822779403,-10.2594333452067,-48.3550682074127));
#18152=CARTESIAN_POINT('Ctrl Pts',(19.8668935038345,-10.0516699968013,-48.355068206755));
#18153=CARTESIAN_POINT('Ctrl Pts',(19.3307765011361,-9.85012639361532,-48.3550682071424));
#18154=CARTESIAN_POINT('Ctrl Pts',(18.7933371416024,-9.6553764716246,-48.3550682075041));
#18155=CARTESIAN_POINT('Ctrl Pts',(18.4431914865909,-9.52849547977083,-48.3550682077397));
#18156=CARTESIAN_POINT('Ctrl Pts',(18.092483769791,-9.4044988724651,-48.3550682078824));
#18157=CARTESIAN_POINT('Ctrl Pts',(17.741376829569,-9.28355639505756,-48.3550682078902));
#18158=CARTESIAN_POINT('Ctrl Pts',(17.5775565924851,-9.2271267918435,-48.3550682078938));
#18159=CARTESIAN_POINT('Ctrl Pts',(17.4135884308508,-9.17133865071493,-48.3550682078751));
#18160=CARTESIAN_POINT('Ctrl Pts',(17.2494553456226,-9.11619658428714,-48.3550682077922));
#18161=CARTESIAN_POINT('Ctrl Pts',(15.6417454071451,-8.57607118482318,-48.3550682069807));
#18162=CARTESIAN_POINT('Ctrl Pts',(14.0213893603513,-8.09914440993566,-48.3550682048256));
#18163=CARTESIAN_POINT('Ctrl Pts',(12.386600966108,-7.69433778621075,-48.3550682041081));
#18164=CARTESIAN_POINT('Ctrl Pts',(10.8104759197869,-7.30405739223667,-48.3550682034163));
#18165=CARTESIAN_POINT('Ctrl Pts',(9.22093586202024,-6.98081413681076,-48.3550682041519));
#18166=CARTESIAN_POINT('Ctrl Pts',(7.61638998568351,-6.73255660071286,-48.3550682056399));
#18167=CARTESIAN_POINT('Ctrl Pts',(6.51321047809351,-6.56187115602289,-48.355068206663));
#18168=CARTESIAN_POINT('Ctrl Pts',(5.40293781007535,-6.42663073301706,-48.3550682079868));
#18169=CARTESIAN_POINT('Ctrl Pts',(4.28505819640523,-6.32940458230469,-48.3550682080579));
#18170=CARTESIAN_POINT('Origin',(48.5210265683621,-85.4775827009602,0.0824317919395913));
#18171=CARTESIAN_POINT('',(48.5210265683621,-6.14692278878556,0.0824317919396692));
#18172=CARTESIAN_POINT('',(48.521026568362,-6.32940458230551,4.28396341998264));
#18173=CARTESIAN_POINT('Origin',(48.5210265743607,-78.8840761814646,0.0808847117366288));
#18174=CARTESIAN_POINT('',(48.5210265683621,-6.32940458230548,-4.1190998361033));
#18175=CARTESIAN_POINT('Origin',(48.5210265744032,-78.8840761438039,0.0839788755104842));
#18176=CARTESIAN_POINT('',(48.5210265683534,-14.454406712551,-29.390860969846));
#18177=CARTESIAN_POINT('Ctrl Pts',(48.5210265683589,-6.32940458230548,-4.1190998361033));
#18178=CARTESIAN_POINT('Ctrl Pts',(48.5210265681324,-6.60009087956923,-7.23137663811504));
#18179=CARTESIAN_POINT('Ctrl Pts',(48.521026561226,-7.16548755819356,-10.2843568006686));
#18180=CARTESIAN_POINT('Ctrl Pts',(48.5210265638678,-7.96970383319668,-13.2892872429231));
#18181=CARTESIAN_POINT('Ctrl Pts',(48.5210265649889,-8.31099929022391,-14.5645276732667));
#18182=CARTESIAN_POINT('Ctrl Pts',(48.5210265670621,-8.69530567656249,-15.8311143436352));
#18183=CARTESIAN_POINT('Ctrl Pts',(48.521026567976,-9.11834864237817,-17.0899074690816));
#18184=CARTESIAN_POINT('Ctrl Pts',(48.5210265680944,-9.17316448001765,-17.2530157232352));
#18185=CARTESIAN_POINT('Ctrl Pts',(48.5210265681212,-9.22862227451093,-17.4159732020842));
#18186=CARTESIAN_POINT('Ctrl Pts',(48.5210265681158,-9.28471651645553,-17.578792525841));
#18187=CARTESIAN_POINT('Ctrl Pts',(48.5210265680965,-9.48472234837756,-18.1593300849925));
#18188=CARTESIAN_POINT('Ctrl Pts',(48.5210265672717,-9.69311870413019,-18.7388810547907));
#18189=CARTESIAN_POINT('Ctrl Pts',(48.5210265669012,-9.90895820808511,-19.3162283146108));
#18190=CARTESIAN_POINT('Ctrl Pts',(48.5210265667027,-10.0245908848499,-19.6255331816648));
#18191=CARTESIAN_POINT('Ctrl Pts',(48.5210265668528,-10.1423607380321,-19.9342053167309));
#18192=CARTESIAN_POINT('Ctrl Pts',(48.5210265674103,-10.2621272193483,-20.2420541910824));
#18193=CARTESIAN_POINT('Ctrl Pts',(48.5210265677982,-10.3454600297987,-20.4562536199356));
#18194=CARTESIAN_POINT('Ctrl Pts',(48.5210265679954,-10.4297627624243,-20.6700738286905));
#18195=CARTESIAN_POINT('Ctrl Pts',(48.5210265681185,-10.5149781806561,-20.8834251134732));
#18196=CARTESIAN_POINT('Ctrl Pts',(48.5210265685952,-10.8449565878873,-21.7095821469555));
#18197=CARTESIAN_POINT('Ctrl Pts',(48.5210265683833,-11.1887405793895,-22.5293727133321));
#18198=CARTESIAN_POINT('Ctrl Pts',(48.521026568327,-11.5450903892478,-23.3435521251211));
#18199=CARTESIAN_POINT('Ctrl Pts',(48.5210265683092,-11.6579509129718,-23.6014131152991));
#18200=CARTESIAN_POINT('Ctrl Pts',(48.5210265682908,-11.7720687209433,-23.8587029990229));
#18201=CARTESIAN_POINT('Ctrl Pts',(48.5210265682786,-11.8874012527351,-24.1154421334782));
#18202=CARTESIAN_POINT('Ctrl Pts',(48.5210265682361,-12.287931373829,-25.0070531561044));
#18203=CARTESIAN_POINT('Ctrl Pts',(48.5210265682847,-12.7030439005514,-25.8920600376509));
#18204=CARTESIAN_POINT('Ctrl Pts',(48.5210265683213,-13.1313454185256,-26.7710851338149));
#18205=CARTESIAN_POINT('Ctrl Pts',(48.521026568358,-13.5596469364998,-27.6501102299789));
#18206=CARTESIAN_POINT('Ctrl Pts',(48.5210265683622,-14.0011371004819,-28.5231537521802));
#18207=CARTESIAN_POINT('Ctrl Pts',(48.5210265683622,-14.4543739218857,-29.3908677089532));
#18208=CARTESIAN_POINT('',(48.5210265683619,-14.4544045823054,29.5557267398091));
#18209=CARTESIAN_POINT('',(48.5210265683619,-14.4544045823054,30.4833980594777));
#18210=CARTESIAN_POINT('Ctrl Pts',(48.5210265683619,-14.4543736124042,29.55573145443));
#18211=CARTESIAN_POINT('Ctrl Pts',(48.5210265683619,-14.0009603589333,28.687680809568));
#18212=CARTESIAN_POINT('Ctrl Pts',(48.5210265683577,-13.5592886344784,27.8142695903511));
#18213=CARTESIAN_POINT('Ctrl Pts',(48.5210265683202,-13.1308037218372,26.9348399998503));
#18214=CARTESIAN_POINT('Ctrl Pts',(48.5210265682827,-12.702318809196,26.0554104093494));
#18215=CARTESIAN_POINT('Ctrl Pts',(48.5210265682328,-12.2870210611714,25.1699622293556));
#18216=CARTESIAN_POINT('Ctrl Pts',(48.5210265682762,-11.8863062114323,24.2778682103323));
#18217=CARTESIAN_POINT('Ctrl Pts',(48.5210265682888,-11.7707122689886,24.0205264503339));
#18218=CARTESIAN_POINT('Ctrl Pts',(48.5210265683076,-11.656337524857,23.762628441714));
#18219=CARTESIAN_POINT('Ctrl Pts',(48.5210265683259,-11.5432249100052,23.5041535003646));
#18220=CARTESIAN_POINT('Ctrl Pts',(48.5210265683772,-11.2263851140862,22.7801392268488));
#18221=CARTESIAN_POINT('Ctrl Pts',(48.5210265684358,-10.9195690672826,22.051898732552));
#18222=CARTESIAN_POINT('Ctrl Pts',(48.5210265682779,-10.6234156301853,21.3183213058656));
#18223=CARTESIAN_POINT('Ctrl Pts',(48.5210265682582,-10.5864935782812,21.2268647146834));
#18224=CARTESIAN_POINT('Ctrl Pts',(48.5210265682323,-10.54973731356,21.135325135413));
#18225=CARTESIAN_POINT('Ctrl Pts',(48.5210265681966,-10.5131481250875,21.043700383894));
#18226=CARTESIAN_POINT('Ctrl Pts',(48.5210265681131,-10.4276256561534,20.8295394447612));
#18227=CARTESIAN_POINT('Ctrl Pts',(48.5210265679788,-10.3430386875933,20.6149485892208));
#18228=CARTESIAN_POINT('Ctrl Pts',(48.5210265677141,-10.2594333452069,20.3999875015178));
#18229=CARTESIAN_POINT('Ctrl Pts',(48.5210265670564,-10.0516699968362,19.8657987275014));
#18230=CARTESIAN_POINT('Ctrl Pts',(48.5210265674438,-9.85012639368244,19.3296817248934));
#18231=CARTESIAN_POINT('Ctrl Pts',(48.5210265678055,-9.65537647172188,18.7922423654503));
#18232=CARTESIAN_POINT('Ctrl Pts',(48.5210265680411,-9.52849547983389,18.4420967103491));
#18233=CARTESIAN_POINT('Ctrl Pts',(48.5210265681838,-9.40449887249552,18.0913889934592));
#18234=CARTESIAN_POINT('Ctrl Pts',(48.5210265681916,-9.2835563950572,17.7402820531467));
#18235=CARTESIAN_POINT('Ctrl Pts',(48.5210265681952,-9.2271267918433,17.5764618160627));
#18236=CARTESIAN_POINT('Ctrl Pts',(48.5210265681765,-9.17133865071483,17.4124936544283));
#18237=CARTESIAN_POINT('Ctrl Pts',(48.5210265680936,-9.11619658428705,17.2483605692001));
#18238=CARTESIAN_POINT('Ctrl Pts',(48.5210265672821,-8.57607118524294,15.6406506319723));
#18239=CARTESIAN_POINT('Ctrl Pts',(48.521026565127,-8.09914441067713,14.020294586448));
#18240=CARTESIAN_POINT('Ctrl Pts',(48.5210265644095,-7.69433778715491,12.3855061934978));
#18241=CARTESIAN_POINT('Ctrl Pts',(48.5210265637178,-7.30405739322943,10.8093811478304));
#18242=CARTESIAN_POINT('Ctrl Pts',(48.5210265644534,-6.98081413779193,9.21984109072944));
#18243=CARTESIAN_POINT('Ctrl Pts',(48.5210265659414,-6.73255660161266,7.6152952150723));
#18244=CARTESIAN_POINT('Ctrl Pts',(48.5210265669644,-6.56187115649859,6.51211570557005));
#18245=CARTESIAN_POINT('Ctrl Pts',(48.5210265682882,-6.42663073318859,5.40184303561563));
#18246=CARTESIAN_POINT('Ctrl Pts',(48.5210265683593,-6.32940458230551,4.28396341998264));
#18247=CARTESIAN_POINT('Origin',(-48.3539734316379,-85.4775827009602,-44.2925682080605));
#18248=CARTESIAN_POINT('',(-48.3539734316379,11.6131136241746,0.0824317919394229));
#18249=CARTESIAN_POINT('',(-48.3539734316379,11.7955954176947,4.28396341998245));
#18250=CARTESIAN_POINT('Origin',(-48.3539734376649,84.3502670064654,0.0808847007703356));
#18251=CARTESIAN_POINT('',(-48.3539734316379,11.7955954176947,-4.11909983610361));
#18252=CARTESIAN_POINT('Origin',(-48.3539734316379,84.3502670509921,0.0839788788605111));
#18253=CARTESIAN_POINT('',(-48.3539734315249,16.1706033824528,-21.353305195093));
#18254=CARTESIAN_POINT('Ctrl Pts',(-48.3539734316379,11.7955954176947,-4.11909983610361));
#18255=CARTESIAN_POINT('Ctrl Pts',(-48.353973431634,11.9012754521151,-5.3341798859156));
#18256=CARTESIAN_POINT('Ctrl Pts',(-48.3539734314967,12.0520583764943,-6.54394408577816));
#18257=CARTESIAN_POINT('Ctrl Pts',(-48.3539734315406,12.2455340422119,-7.74867686713406));
#18258=CARTESIAN_POINT('Ctrl Pts',(-48.3539734315501,12.2874241550106,-8.00951789805218));
#18259=CARTESIAN_POINT('Ctrl Pts',(-48.3539734315666,12.3313158172651,-8.27012304299333));
#18260=CARTESIAN_POINT('Ctrl Pts',(-48.3539734315853,12.3771848834513,-8.53049515220305));
#18261=CARTESIAN_POINT('Ctrl Pts',(-48.3539734315909,12.3910255799847,-8.60906076622044));
#18262=CARTESIAN_POINT('Ctrl Pts',(-48.3539734315881,12.4050450140598,-8.68760078593728));
#18263=CARTESIAN_POINT('Ctrl Pts',(-48.3539734315757,12.4192427232385,-8.7661163838354));
#18264=CARTESIAN_POINT('Ctrl Pts',(-48.3539734314889,12.5191317203699,-9.31851848156123));
#18265=CARTESIAN_POINT('Ctrl Pts',(-48.3539734306321,12.6280707956224,-9.8704261542129));
#18266=CARTESIAN_POINT('Ctrl Pts',(-48.3539734253286,12.7454889374165,-10.4210002063411));
#18267=CARTESIAN_POINT('Ctrl Pts',(-48.3539734198873,12.8659559514451,-10.9858704303805));
#18268=CARTESIAN_POINT('Ctrl Pts',(-48.3539734095596,12.9953485174401,-11.5493381718557));
#18269=CARTESIAN_POINT('Ctrl Pts',(-48.3539734075923,13.1331031833232,-12.1104878242374));
#18270=CARTESIAN_POINT('Ctrl Pts',(-48.3539734066747,13.1973553945651,-12.3722220150321));
#18271=CARTESIAN_POINT('Ctrl Pts',(-48.3539734078578,13.2634275010588,-12.6334516466247));
#18272=CARTESIAN_POINT('Ctrl Pts',(-48.3539734114491,13.3312657045535,-12.8940818979516));
#18273=CARTESIAN_POINT('Ctrl Pts',(-48.3539734141449,13.3821877700732,-13.089721376163));
#18274=CARTESIAN_POINT('Ctrl Pts',(-48.353973416395,13.4341067575185,-13.2850480331676));
#18275=CARTESIAN_POINT('Ctrl Pts',(-48.3539734183061,13.4869947668895,-13.4800014094153));
#18276=CARTESIAN_POINT('Ctrl Pts',(-48.3539734261861,13.7050584674933,-14.2838179110258));
#18277=CARTESIAN_POINT('Ctrl Pts',(-48.3539734286587,13.9395350033133,-15.0824829261137));
#18278=CARTESIAN_POINT('Ctrl Pts',(-48.3539734300256,14.1892982822773,-15.8762917931586));
#18279=CARTESIAN_POINT('Ctrl Pts',(-48.3539734314172,14.4435598427712,-16.6843973005252));
#18280=CARTESIAN_POINT('Ctrl Pts',(-48.3539734315029,14.7136635661991,-17.487470208706));
#18281=CARTESIAN_POINT('Ctrl Pts',(-48.3539734315848,14.9983707523295,-18.2858425197307));
#18282=CARTESIAN_POINT('Ctrl Pts',(-48.3539734316691,15.2915959446077,-19.108100916477));
#18283=CARTESIAN_POINT('Ctrl Pts',(-48.3539734316379,15.6003113763674,-19.9253732888144));
#18284=CARTESIAN_POINT('Ctrl Pts',(-48.353973431638,15.9231126704198,-20.738043122766));
#18285=CARTESIAN_POINT('Ctrl Pts',(-48.353973431638,16.0046899473676,-20.9434183592749));
#18286=CARTESIAN_POINT('Ctrl Pts',(-48.353973431638,16.0871665857534,-21.1484997497311));
#18287=CARTESIAN_POINT('Ctrl Pts',(-48.353973431638,16.1705194395641,-21.3532936780839));
#18288=CARTESIAN_POINT('',(-48.3539734315243,16.1706033612909,21.5181686663419));
#18289=CARTESIAN_POINT('',(-48.3539734316379,16.1705954176946,-44.2925682080605));
#18290=CARTESIAN_POINT('Ctrl Pts',(-48.3539734316379,16.1705196413371,21.5181571799855));
#18291=CARTESIAN_POINT('Ctrl Pts',(-48.3539734316379,15.8435202227306,20.7147347555301));
#18292=CARTESIAN_POINT('Ctrl Pts',(-48.3539734316511,15.5300086685144,19.9068834941557));
#18293=CARTESIAN_POINT('Ctrl Pts',(-48.3539734316247,15.231367963442,19.0942317333251));
#18294=CARTESIAN_POINT('Ctrl Pts',(-48.3539734315988,14.9390610385349,18.2988152572923));
#18295=CARTESIAN_POINT('Ctrl Pts',(-48.3539734316217,14.661001060423,17.498799666427));
#18296=CARTESIAN_POINT('Ctrl Pts',(-48.3539734308659,14.3984390229057,16.6938550497342));
#18297=CARTESIAN_POINT('Ctrl Pts',(-48.3539734301297,14.1426624799502,15.9097129350739));
#18298=CARTESIAN_POINT('Ctrl Pts',(-48.3539734287875,13.9015932981126,15.1208932392611));
#18299=CARTESIAN_POINT('Ctrl Pts',(-48.3539734237001,13.6763418781396,14.327109601817));
#18300=CARTESIAN_POINT('Ctrl Pts',(-48.3539734222457,13.611948351827,14.100187491624));
#18301=CARTESIAN_POINT('Ctrl Pts',(-48.3539734204628,13.5488472152034,13.8728598288434));
#18302=CARTESIAN_POINT('Ctrl Pts',(-48.3539734182148,13.4870636734944,13.6451202163981));
#18303=CARTESIAN_POINT('Ctrl Pts',(-48.3539734162904,13.4341751304698,13.4501683577308));
#18304=CARTESIAN_POINT('Ctrl Pts',(-48.3539734140247,13.3822549873807,13.2548408272286));
#18305=CARTESIAN_POINT('Ctrl Pts',(-48.3539734113102,13.3313312754875,13.0591984279295));
#18306=CARTESIAN_POINT('Ctrl Pts',(-48.3539734035448,13.1856558716878,12.4995321259522));
#18307=CARTESIAN_POINT('Ctrl Pts',(-48.3539734087768,13.0481153498403,11.9370799621826));
#18308=CARTESIAN_POINT('Ctrl Pts',(-48.3539734159749,12.9192577967628,11.3727821628695));
#18309=CARTESIAN_POINT('Ctrl Pts',(-48.3539734230251,12.7930466643237,10.8200736674549));
#18310=CARTESIAN_POINT('Ctrl Pts',(-48.3539734290975,12.675165032771,10.2655932894663));
#18311=CARTESIAN_POINT('Ctrl Pts',(-48.3539734306761,12.5661734819508,9.71020714836219));
#18312=CARTESIAN_POINT('Ctrl Pts',(-48.3539734314138,12.515246017069,9.45069704887183));
#18313=CARTESIAN_POINT('Ctrl Pts',(-48.3539734315343,12.4662602455005,9.19098905945248));
#18314=CARTESIAN_POINT('Ctrl Pts',(-48.3539734315754,12.4192773203286,8.9311713748959));
#18315=CARTESIAN_POINT('Ctrl Pts',(-48.3539734315878,12.4050773744282,8.85264503684491));
#18316=CARTESIAN_POINT('Ctrl Pts',(-48.3539734315907,12.3910557938715,8.77409450616072));
#18317=CARTESIAN_POINT('Ctrl Pts',(-48.353973431585,12.3772130393338,8.695518620036));
#18318=CARTESIAN_POINT('Ctrl Pts',(-48.3539734314988,12.1658567957286,7.49579322693565));
#18319=CARTESIAN_POINT('Ctrl Pts',(-48.3539734315723,11.9964818470948,6.29113564323276));
#18320=CARTESIAN_POINT('Ctrl Pts',(-48.3539734316199,11.8714667021317,5.08126600825786));
#18321=CARTESIAN_POINT('Ctrl Pts',(-48.3539734316303,11.8440311371517,4.81575052213465));
#18322=CARTESIAN_POINT('Ctrl Pts',(-48.353973431637,11.8187322169269,4.54998399158691));
#18323=CARTESIAN_POINT('Ctrl Pts',(-48.3539734316379,11.7955954176945,4.28396341998246));
#18324=CARTESIAN_POINT('Origin',(0.0835265683620484,-85.4775827009602,48.5199317919394));
#18325=CARTESIAN_POINT('',(0.0835265683620147,-6.14692278878557,48.5199317919394));
#18326=CARTESIAN_POINT('',(-4.11800505968107,-6.32940458230551,48.5199317919394));
#18327=CARTESIAN_POINT('Origin',(0.0850736476760322,-78.8840761880214,48.5199317979381));
#18328=CARTESIAN_POINT('',(4.2850581964051,-6.32940458230551,48.5199317919394));
#18329=CARTESIAN_POINT('Origin',(0.0819794837711729,-78.8840761734555,48.5199317979947));
#18330=CARTESIAN_POINT('',(29.5568193301503,-14.4544067125516,48.5199317919306));
#18331=CARTESIAN_POINT('Ctrl Pts',(4.2850581964051,-6.3294045823055,48.5199317919363));
#18332=CARTESIAN_POINT('Ctrl Pts',(7.39733506399622,-6.60009088527294,48.5199317917098));
#18333=CARTESIAN_POINT('Ctrl Pts',(10.450315289629,-7.16548758202087,48.5199317848033));
#18334=CARTESIAN_POINT('Ctrl Pts',(13.4552457931766,-7.96970388403428,48.5199317874451));
#18335=CARTESIAN_POINT('Ctrl Pts',(14.7304861593436,-8.3109993283869,48.5199317885663));
#18336=CARTESIAN_POINT('Ctrl Pts',(15.9970727664377,-8.69530569756759,48.5199317906394));
#18337=CARTESIAN_POINT('Ctrl Pts',(17.2558658293831,-9.11834864237876,48.5199317915533));
#18338=CARTESIAN_POINT('Ctrl Pts',(17.4189740835368,-9.17316448001826,48.5199317916717));
#18339=CARTESIAN_POINT('Ctrl Pts',(17.5819315623858,-9.2286222745116,48.5199317916985));
#18340=CARTESIAN_POINT('Ctrl Pts',(17.7447508861427,-9.28471651645626,48.5199317916931));
#18341=CARTESIAN_POINT('Ctrl Pts',(18.3252884455851,-9.48472234847866,48.5199317916738));
#18342=CARTESIAN_POINT('Ctrl Pts',(18.9048394156729,-9.69311870433946,48.519931790849));
#18343=CARTESIAN_POINT('Ctrl Pts',(19.4821866757799,-9.90895820840961,48.5199317904785));
#18344=CARTESIAN_POINT('Ctrl Pts',(19.7914915425436,-10.0245908850701,48.51993179028));
#18345=CARTESIAN_POINT('Ctrl Pts',(20.1001636773203,-10.142360738144,48.5199317904301));
#18346=CARTESIAN_POINT('Ctrl Pts',(20.4080125513842,-10.2621272193482,48.5199317909876));
#18347=CARTESIAN_POINT('Ctrl Pts',(20.6222119802371,-10.3454600297985,48.5199317913755));
#18348=CARTESIAN_POINT('Ctrl Pts',(20.836032188992,-10.4297627624242,48.5199317915727));
#18349=CARTESIAN_POINT('Ctrl Pts',(21.049383473775,-10.5149781806563,48.5199317916958));
#18350=CARTESIAN_POINT('Ctrl Pts',(21.8755405072593,-10.8449565878891,48.5199317921725));
#18351=CARTESIAN_POINT('Ctrl Pts',(22.6953310736331,-11.1887405793906,48.5199317919606));
#18352=CARTESIAN_POINT('Ctrl Pts',(23.5095104854225,-11.5450903892486,48.5199317919043));
#18353=CARTESIAN_POINT('Ctrl Pts',(23.7673714756,-11.6579509129722,48.5199317918865));
#18354=CARTESIAN_POINT('Ctrl Pts',(24.0246613593238,-11.7720687209435,48.5199317918681));
#18355=CARTESIAN_POINT('Ctrl Pts',(24.2814004937799,-11.8874012527353,48.5199317918559));
#18356=CARTESIAN_POINT('Ctrl Pts',(25.1730115164114,-12.2879313738302,48.5199317918134));
#18357=CARTESIAN_POINT('Ctrl Pts',(26.0580183979601,-12.7030439005477,48.519931791862));
#18358=CARTESIAN_POINT('Ctrl Pts',(26.9370434941245,-13.1313454185182,48.5199317918986));
#18359=CARTESIAN_POINT('Ctrl Pts',(27.8160685902889,-13.5596469364886,48.5199317919352));
#18360=CARTESIAN_POINT('Ctrl Pts',(28.6891121124888,-14.001137100468,48.5199317919394));
#18361=CARTESIAN_POINT('Ctrl Pts',(29.5568260692594,-14.4543739218769,48.5199317919394));
#18362=CARTESIAN_POINT('',(-29.3897683795096,-14.4544045823054,48.5199317919394));
#18363=CARTESIAN_POINT('',(-30.3174396991767,-14.4544045823054,48.5199317919394));
#18364=CARTESIAN_POINT('Ctrl Pts',(-29.3897730941313,-14.4543736123985,
48.5199317919394));
#18365=CARTESIAN_POINT('Ctrl Pts',(-28.5217224492708,-14.0009603589245,
48.5199317919394));
#18366=CARTESIAN_POINT('Ctrl Pts',(-27.6483112300529,-13.5592886344715,
48.5199317919352));
#18367=CARTESIAN_POINT('Ctrl Pts',(-26.7688816395507,-13.1308037218328,
48.5199317918976));
#18368=CARTESIAN_POINT('Ctrl Pts',(-25.8894520490486,-12.702318809194,48.5199317918601));
#18369=CARTESIAN_POINT('Ctrl Pts',(-25.0040038690532,-12.2870210611724,
48.5199317918103));
#18370=CARTESIAN_POINT('Ctrl Pts',(-24.1119098500306,-11.8863062114326,
48.5199317918537));
#18371=CARTESIAN_POINT('Ctrl Pts',(-23.8545680900323,-11.7707122689887,
48.5199317918662));
#18372=CARTESIAN_POINT('Ctrl Pts',(-23.5966700814124,-11.656337524857,48.5199317918851));
#18373=CARTESIAN_POINT('Ctrl Pts',(-23.338195140063,-11.5432249100053,48.5199317919034));
#18374=CARTESIAN_POINT('Ctrl Pts',(-22.614180866145,-11.2263851139103,48.5199317919547));
#18375=CARTESIAN_POINT('Ctrl Pts',(-21.8859403714393,-10.9195690669419,
48.5199317920133));
#18376=CARTESIAN_POINT('Ctrl Pts',(-21.1523629443404,-10.6234156296919,
48.5199317918553));
#18377=CARTESIAN_POINT('Ctrl Pts',(-21.0609063535652,-10.5864935779538,
48.5199317918356));
#18378=CARTESIAN_POINT('Ctrl Pts',(-20.9693667747026,-10.5497373133972,
48.5199317918098));
#18379=CARTESIAN_POINT('Ctrl Pts',(-20.8777420235922,-10.5131481250878,
48.5199317917741));
#18380=CARTESIAN_POINT('Ctrl Pts',(-20.6635810844597,-10.4276256561535,
48.5199317916905));
#18381=CARTESIAN_POINT('Ctrl Pts',(-20.4489902289193,-10.3430386875933,
48.5199317915563));
#18382=CARTESIAN_POINT('Ctrl Pts',(-20.2340291412162,-10.2594333452069,
48.5199317912916));
#18383=CARTESIAN_POINT('Ctrl Pts',(-19.6998403673666,-10.051669996901,48.5199317906338));
#18384=CARTESIAN_POINT('Ctrl Pts',(-19.1637233649263,-9.85012639380828,
48.5199317910213));
#18385=CARTESIAN_POINT('Ctrl Pts',(-18.6262840056516,-9.6553764719043,48.5199317913829));
#18386=CARTESIAN_POINT('Ctrl Pts',(-18.2761383503831,-9.52849547995278,
48.5199317916186));
#18387=CARTESIAN_POINT('Ctrl Pts',(-17.9254306333254,-9.40449887255358,
48.5199317917613));
#18388=CARTESIAN_POINT('Ctrl Pts',(-17.574323692845,-9.28355639505737,48.519931791769));
#18389=CARTESIAN_POINT('Ctrl Pts',(-17.410503455761,-9.22712679184346,48.5199317917726));
#18390=CARTESIAN_POINT('Ctrl Pts',(-17.2465352941267,-9.17133865071499,
48.5199317917539));
#18391=CARTESIAN_POINT('Ctrl Pts',(-17.0824022088985,-9.11619658428719,
48.5199317916711));
#18392=CARTESIAN_POINT('Ctrl Pts',(-15.4746922696518,-8.57607118456477,
48.5199317908595));
#18393=CARTESIAN_POINT('Ctrl Pts',(-13.8543362220765,-8.09914440947939,
48.5199317887045));
#18394=CARTESIAN_POINT('Ctrl Pts',(-12.219547827037,-7.69433778562994,48.519931787987));
#18395=CARTESIAN_POINT('Ctrl Pts',(-10.6434227803378,-7.30405739163223,
48.5199317872952));
#18396=CARTESIAN_POINT('Ctrl Pts',(-9.0538827221862,-6.98081413621769,48.5199317880308));
#18397=CARTESIAN_POINT('Ctrl Pts',(-7.44933684545642,-6.73255660017158,
48.5199317895188));
#18398=CARTESIAN_POINT('Ctrl Pts',(-6.34615733901905,-6.56187115573737,
48.5199317905419));
#18399=CARTESIAN_POINT('Ctrl Pts',(-5.23588467216803,-6.42663073291497,
48.5199317918656));
#18400=CARTESIAN_POINT('Ctrl Pts',(-4.11800505968107,-6.3294045823055,48.5199317919367));
#18401=CARTESIAN_POINT('Origin',(0.0835265683620477,-6.01690458230549,0.0824317919394229));
#18402=CARTESIAN_POINT('',(-45.805095386722,-13.2959337131846,-31.5176630410747));
#18403=CARTESIAN_POINT('',(-46.7085547781037,-13.2959337131846,-30.163770311099));
#18404=CARTESIAN_POINT('Origin',(0.0835265683620477,-13.2959337131846,0.0824317919394229));
#18405=CARTESIAN_POINT('',(-46.4447277393149,-12.6709337131846,-29.4166890942607));
#18406=CARTESIAN_POINT('Ctrl Pts',(-46.7085547781037,-13.2959337131846,
-30.163770311099));
#18407=CARTESIAN_POINT('Ctrl Pts',(-46.7308018048241,-13.2959337131846,
-30.129353273202));
#18408=CARTESIAN_POINT('Ctrl Pts',(-46.7494092222397,-13.2919430659168,
-30.0931246196562));
#18409=CARTESIAN_POINT('Ctrl Pts',(-46.7639937886785,-13.2842290832231,
-30.0561954407828));
#18410=CARTESIAN_POINT('Ctrl Pts',(-46.7786223726414,-13.2764918190406,
-30.0191548063493));
#18411=CARTESIAN_POINT('Ctrl Pts',(-46.7892044314641,-13.2650083398592,
-29.9814076918208));
#18412=CARTESIAN_POINT('Ctrl Pts',(-46.7953183242711,-13.2500137812566,
-29.9440648720613));
#18413=CARTESIAN_POINT('Ctrl Pts',(-46.7975557030175,-13.2445265233364,
-29.9303992691638));
#18414=CARTESIAN_POINT('Ctrl Pts',(-46.7991943226864,-13.2385687578685,
-29.9167878375396));
#18415=CARTESIAN_POINT('Ctrl Pts',(-46.800212090454,-13.2321510039651,-29.9032853674899));
#18416=CARTESIAN_POINT('Ctrl Pts',(-46.8002328818205,-13.2320198995248,
-29.9030095336383));
#18417=CARTESIAN_POINT('Ctrl Pts',(-46.8002534141945,-13.2318886036913,
-29.9027337461559));
#18418=CARTESIAN_POINT('Ctrl Pts',(-46.8002736873875,-13.2317571165657,
-29.9024580055318));
#18419=CARTESIAN_POINT('Ctrl Pts',(-46.8037330656023,-13.2093204091686,
-29.855406161685));
#18420=CARTESIAN_POINT('Ctrl Pts',(-46.7999626260835,-13.182136836623,-29.8107688763396));
#18421=CARTESIAN_POINT('Ctrl Pts',(-46.7906793329817,-13.1520894283718,
-29.7694085048952));
#18422=CARTESIAN_POINT('Ctrl Pts',(-46.7828212048694,-13.1266548782729,
-29.7343977501966));
#18423=CARTESIAN_POINT('Ctrl Pts',(-46.7710141350354,-13.0991694705396,
-29.7017353456062));
#18424=CARTESIAN_POINT('Ctrl Pts',(-46.7563177878289,-13.0707895719797,
-29.6719424887082));
#18425=CARTESIAN_POINT('Ctrl Pts',(-46.7561779609415,-13.0705195543472,
-29.6716590276285));
#18426=CARTESIAN_POINT('Ctrl Pts',(-46.7560378601023,-13.0702494422352,
-29.6713758206481));
#18427=CARTESIAN_POINT('Ctrl Pts',(-46.7558974863178,-13.0699792367999,
-29.6710928683671));
#18428=CARTESIAN_POINT('Ctrl Pts',(-46.7457918813678,-13.0505269623226,
-29.6507229397278));
#18429=CARTESIAN_POINT('Ctrl Pts',(-46.73431142011,-13.0305367697067,-29.6315119049251));
#18430=CARTESIAN_POINT('Ctrl Pts',(-46.7216707893827,-13.0101903794928,
-29.6134615953136));
#18431=CARTESIAN_POINT('Ctrl Pts',(-46.7142947412409,-12.9983178743173,
-29.6029288967844));
#18432=CARTESIAN_POINT('Ctrl Pts',(-46.7065242359664,-12.9863240855344,
-29.5927905109074));
#18433=CARTESIAN_POINT('Ctrl Pts',(-46.6984056317191,-12.9742444051773,
-29.5830396522533));
#18434=CARTESIAN_POINT('Ctrl Pts',(-46.6872931082818,-12.9577100691025,
-29.5696929436287));
#18435=CARTESIAN_POINT('Ctrl Pts',(-46.6755261223313,-12.9410147689399,
-29.5570758028062));
#18436=CARTESIAN_POINT('Ctrl Pts',(-46.6632182383888,-12.9242496162066,
-29.5451798612475));
#18437=CARTESIAN_POINT('Ctrl Pts',(-46.6570642964176,-12.9158670398399,
-29.5392318904681));
#18438=CARTESIAN_POINT('Ctrl Pts',(-46.6507751298663,-12.9074670004228,
-29.5334642194506));
#18439=CARTESIAN_POINT('Ctrl Pts',(-46.6443649334478,-12.8990608878296,
-29.5278758016581));
#18440=CARTESIAN_POINT('Ctrl Pts',(-46.6379547370293,-12.8906547752363,
-29.5222873838655));
#18441=CARTESIAN_POINT('Ctrl Pts',(-46.6314235107303,-12.8822425894822,
-29.5168782192877));
#18442=CARTESIAN_POINT('Ctrl Pts',(-46.6247854486351,-12.8738357211132,
-29.5116472610983));
#18443=CARTESIAN_POINT('Ctrl Pts',(-46.6039049055347,-12.8473912596424,
-29.4951928733019));
#18444=CARTESIAN_POINT('Ctrl Pts',(-46.58177099161,-12.8207472740161,-29.4803404238949));
#18445=CARTESIAN_POINT('Ctrl Pts',(-46.5586011720367,-12.7940681980357,
-29.467056051049));
#18446=CARTESIAN_POINT('Ctrl Pts',(-46.5523076389907,-12.7868214585527,
-29.4634476656131));
#18447=CARTESIAN_POINT('Ctrl Pts',(-46.5459376589846,-12.7795722581759,
-29.4599552418543));
#18448=CARTESIAN_POINT('Ctrl Pts',(-46.5394956075852,-12.7723242153339,
-29.4565786810166));
#18449=CARTESIAN_POINT('Ctrl Pts',(-46.5160864719647,-12.7459862668529,
-29.4443089293986));
#18450=CARTESIAN_POINT('Ctrl Pts',(-46.4917263584107,-12.7196622748126,
-29.433565514209));
#18451=CARTESIAN_POINT('Ctrl Pts',(-46.4666223821401,-12.6935087390694,
-29.4243162909518));
#18452=CARTESIAN_POINT('Ctrl Pts',(-46.4593842022175,-12.6859679417358,
-29.4216494806681));
#18453=CARTESIAN_POINT('Ctrl Pts',(-46.4520842494196,-12.6784415052693,
-29.4191071382984));
#18454=CARTESIAN_POINT('Ctrl Pts',(-46.4447277393149,-12.6709337131846,
-29.4166890942607));
#18455=CARTESIAN_POINT('',(-39.9859592520698,-6.10843371318466,-27.2946201763046));
#18456=CARTESIAN_POINT('Origin',(-197.331032377167,-177.510314406253,-79.3434317434775));
#18457=CARTESIAN_POINT('',(-48.261606955145,-6.10843371318471,-4.13831849444347));
#18458=CARTESIAN_POINT('Origin',(0.0835265683620477,-6.10843371318469,0.0824317919394229));
#18459=CARTESIAN_POINT('',(-48.2284487824326,-14.6753754514266,-30.3462212704581));
#18460=CARTESIAN_POINT('Ctrl Pts',(-48.2616069550931,-6.10843371318472,
-4.13831849503754));
#18461=CARTESIAN_POINT('Ctrl Pts',(-48.2597772986175,-6.50994980321316,
-8.77579754148006));
#18462=CARTESIAN_POINT('Ctrl Pts',(-48.2550176567395,-7.55645913600449,
-13.2581019939041));
#18463=CARTESIAN_POINT('Ctrl Pts',(-48.2459144235836,-9.80534906153842,
-19.8181734642193));
#18464=CARTESIAN_POINT('Ctrl Pts',(-48.2425547211608,-10.6692546575742,
-21.9792831240841));
#18465=CARTESIAN_POINT('Ctrl Pts',(-48.2356129829617,-12.5596572871779,
-26.217495153478));
#18466=CARTESIAN_POINT('Ctrl Pts',(-48.2320290688777,-13.58630787804,-28.2970230681186));
#18467=CARTESIAN_POINT('Ctrl Pts',(-48.2284487824325,-14.6753754514262,
-30.3462212704574));
#18468=CARTESIAN_POINT('',(-47.1694990908375,-14.6753754514262,-31.9659918126394));
#18469=CARTESIAN_POINT('Origin',(0.0835265683620477,-14.6753754514262,0.0824317919394229));
#18470=CARTESIAN_POINT('Origin',(1241.62995219148,-1402.95413115888,321.769152191711));
#18471=CARTESIAN_POINT('Origin',(0.0835265683620477,-11.0169045823054,0.0824317919394229));
#18472=CARTESIAN_POINT('',(15.3925785990456,-11.0169045823054,23.5078932009404));
#18473=CARTESIAN_POINT('',(7.67510093260532,-11.0169045823054,20.9630507178886));
#18474=CARTESIAN_POINT('',(-5.38208978662056,-11.0169045823054,16.6574349341085));
#18475=CARTESIAN_POINT('',(14.5949188243533,-11.0169045823054,25.9268725828089));
#18476=CARTESIAN_POINT('',(9.92432302202933,-11.0169045823054,19.2683675629017));
#18477=CARTESIAN_POINT('Origin',(10.2095634989472,-11.0169045823054,19.8244816432194));
#18478=CARTESIAN_POINT('',(20.56141397709,-11.0169045823054,6.83502636924522));
#18479=CARTESIAN_POINT('Origin',(0.0835265683620477,-11.0169045823054,0.0824317919394229));
#18480=CARTESIAN_POINT('',(34.0350086811056,-11.0169045823054,-34.02493526194));
#18481=CARTESIAN_POINT('',(34.0952935222086,-11.0169045823054,-34.2077547951474));
#18482=CARTESIAN_POINT('',(29.6625358445444,-11.0169045823054,-37.8793626234925));
#18483=CARTESIAN_POINT('Origin',(0.0835265683620477,-11.0169045823054,0.0824317919394229));
#18484=CARTESIAN_POINT('',(20.4191383735183,-11.0169045823054,-9.84787775959334));
#18485=CARTESIAN_POINT('',(15.4714058027788,-11.0169045823054,5.15659338881741));
#18486=CARTESIAN_POINT('',(19.2694623393243,-11.0169045823054,-9.75836466172779));
#18487=CARTESIAN_POINT('Origin',(19.8255764196421,-11.0169045823054,-10.0436051386457));
#18488=CARTESIAN_POINT('',(6.83612114566777,-11.0169045823054,-20.3954556167886));
#18489=CARTESIAN_POINT('Origin',(0.0835265683620477,-11.0169045823054,0.0824317919394229));
#18490=CARTESIAN_POINT('',(-34.0238404855175,-11.0169045823054,-33.869050320804));
#18491=CARTESIAN_POINT('',(-34.2066600187249,-11.0169045823054,-33.9293351619071));
#18492=CARTESIAN_POINT('',(-37.87826784707,-11.0169045823054,-29.4965774842428));
#18493=CARTESIAN_POINT('Origin',(0.0835265683620477,-11.0169045823054,0.0824317919394229));
#18494=CARTESIAN_POINT('',(-9.84678298317079,-11.0169045823054,-20.2531800132168));
#18495=CARTESIAN_POINT('',(5.15768816523998,-11.0169045823054,-15.3054474424773));
#18496=CARTESIAN_POINT('',(-9.75726988530523,-11.0169045823054,-19.1035039790228));
#18497=CARTESIAN_POINT('Origin',(-10.0425103622231,-11.0169045823054,-19.6596180593406));
#18498=CARTESIAN_POINT('',(-20.394360840366,-11.0169045823054,-6.6701627853663));
#18499=CARTESIAN_POINT('Origin',(0.0835265683620477,-11.0169045823054,0.0824317919394229));
#18500=CARTESIAN_POINT('',(-33.8679555443817,-11.0169045823054,34.1897988458186));
#18501=CARTESIAN_POINT('',(-33.9282403854848,-11.0169045823054,34.372618379026));
#18502=CARTESIAN_POINT('',(-29.4954827078206,-11.0169045823054,38.0442262073711));
#18503=CARTESIAN_POINT('Origin',(0.0835265683620477,-11.0169045823054,0.0824317919394229));
#18504=CARTESIAN_POINT('',(-15.3043526660546,-11.0169045823054,-4.99172980493867));
#18505=CARTESIAN_POINT('',(-6.66906800894368,-11.0169045823054,20.5603192006674));
#18506=CARTESIAN_POINT('Origin',(0.0835265683620477,-11.0169045823054,0.0824317919394229));
#18507=CARTESIAN_POINT('',(34.1908936222416,-11.0169045823054,34.0339139046828));
#18508=CARTESIAN_POINT('',(34.373713155449,-11.0169045823054,34.0941987457859));
#18509=CARTESIAN_POINT('',(38.0453209837941,-11.0169045823054,29.6614410681217));
#18510=CARTESIAN_POINT('Origin',(0.0835265683620477,-11.0169045823054,0.0824317919394229));
#18511=CARTESIAN_POINT('',(18.7518431265311,-11.0169045823054,23.2994061884498));
#18512=CARTESIAN_POINT('',(-4.99063502851588,-11.0169045823054,15.4703110263562));
#18513=CARTESIAN_POINT('',(17.9541833518389,-11.0169045823054,25.7183855703182));
#18514=CARTESIAN_POINT('',(-6.17974956131282,-11.0169045823054,19.076414315977));
#18515=CARTESIAN_POINT('',(-6.17974956131282,-11.0169045823054,19.076414315977));
#18516=CARTESIAN_POINT('',(7.59696574233659,-11.0169045823054,18.6174859267129));
#18517=CARTESIAN_POINT('Origin',(0.0835265683620477,-11.0169045823054,0.0824317919394229));
#18518=CARTESIAN_POINT('Origin',(8.06655569071,-11.0169045823054,19.7759268101363));
#18519=CARTESIAN_POINT('Origin',(5.05982447571381,-11.0169045823054,-15.0086664655392));
#18520=CARTESIAN_POINT('',(-9.94464667269696,-14.4544045823054,-19.9563990362787));
#18521=CARTESIAN_POINT('',(-9.94464667269696,-11.3294045823054,-19.9563990362787));
#18522=CARTESIAN_POINT('',(-9.94464667269695,-11.0169045823054,-19.9563990362787));
#18523=CARTESIAN_POINT('',(5.05982447571381,-11.3294045823054,-15.0086664655392));
#18524=CARTESIAN_POINT('',(-38.8106378122313,-13.5169045823054,-29.4749754082874));
#18525=CARTESIAN_POINT('Ctrl Pts',(-38.8106378122313,-13.5169045823054,
-29.4749754082875));
#18526=CARTESIAN_POINT('Ctrl Pts',(-38.7753398292788,-13.516904574972,-29.4633358790959));
#18527=CARTESIAN_POINT('Ctrl Pts',(-38.740120224442,-13.5137764691087,-29.4517221951311));
#18528=CARTESIAN_POINT('Ctrl Pts',(-38.7054177666676,-13.5077394335821,
-29.4402790406912));
#18529=CARTESIAN_POINT('Ctrl Pts',(-38.6681956028728,-13.5012640557669,
-29.4280050118123));
#18530=CARTESIAN_POINT('Ctrl Pts',(-38.6315672874808,-13.4914421681932,
-29.4159268047662));
#18531=CARTESIAN_POINT('Ctrl Pts',(-38.5960538527439,-13.4784883891798,
-29.4042162302247));
#18532=CARTESIAN_POINT('Ctrl Pts',(-38.5599884642765,-13.4653332811001,
-29.3923236486385));
#18533=CARTESIAN_POINT('Ctrl Pts',(-38.5250713397532,-13.4489478321153,
-29.3808097077152));
#18534=CARTESIAN_POINT('Ctrl Pts',(-38.4918489021924,-13.4295031815242,
-29.3698545907503));
#18535=CARTESIAN_POINT('Ctrl Pts',(-38.4597058287231,-13.4106902683721,
-29.3592553946852));
#18536=CARTESIAN_POINT('Ctrl Pts',(-38.4291478346119,-13.3890130654893,
-29.3491788794119));
#18537=CARTESIAN_POINT('Ctrl Pts',(-38.4006911147723,-13.3645846069462,
-29.3397952604838));
#18538=CARTESIAN_POINT('Ctrl Pts',(-38.3914518672752,-13.3566532439598,
-29.3367486135694));
#18539=CARTESIAN_POINT('Ctrl Pts',(-38.3824343769285,-13.3484315569496,
-29.3337750911969));
#18540=CARTESIAN_POINT('Ctrl Pts',(-38.3736571535326,-13.3399225829037,
-29.3308807969828));
#18541=CARTESIAN_POINT('Ctrl Pts',(-38.3735625124312,-13.3398308342221,
-29.3308495890278));
#18542=CARTESIAN_POINT('Ctrl Pts',(-38.3734678995551,-13.3397390509054,
-29.3308183903802));
#18543=CARTESIAN_POINT('Ctrl Pts',(-38.3733733149185,-13.3396472329757,
-29.3307872010446));
#18544=CARTESIAN_POINT('Ctrl Pts',(-38.3385278839172,-13.3058210699866,
-29.3192969011185));
#18545=CARTESIAN_POINT('Ctrl Pts',(-38.3076591439821,-13.2674403223333,
-29.3091179172323));
#18546=CARTESIAN_POINT('Ctrl Pts',(-38.2814620639506,-13.2257618864376,
-29.3004794157585));
#18547=CARTESIAN_POINT('Ctrl Pts',(-38.267671485342,-13.2038216646339,-29.295931964917));
#18548=CARTESIAN_POINT('Ctrl Pts',(-38.2551759277532,-13.1809667714821,
-29.2918115479652));
#18549=CARTESIAN_POINT('Ctrl Pts',(-38.244080552279,-13.1573764603981,-29.2881528418319));
#18550=CARTESIAN_POINT('Ctrl Pts',(-38.2261880905563,-13.1193345988063,
-29.2822527927891));
#18551=CARTESIAN_POINT('Ctrl Pts',(-38.2119311974999,-13.0793753611319,
-29.2775515745033));
#18552=CARTESIAN_POINT('Ctrl Pts',(-38.2017729510058,-13.0382175960144,
-29.2742018871638));
#18553=CARTESIAN_POINT('Ctrl Pts',(-38.1918154952388,-12.9978733667359,
-29.2709184106765));
#18554=CARTESIAN_POINT('Ctrl Pts',(-38.1857967255739,-12.9563778844919,
-29.2689337180864));
#18555=CARTESIAN_POINT('Ctrl Pts',(-38.1841997911564,-12.9144212113995,
-29.2684071280885));
#18556=CARTESIAN_POINT('Ctrl Pts',(-38.1839146266109,-12.9069290091652,
-29.2683130949236));
#18557=CARTESIAN_POINT('Ctrl Pts',(-38.1837705844942,-12.8994221374466,
-29.2682655969568));
#18558=CARTESIAN_POINT('Ctrl Pts',(-38.1837705810014,-12.8919045823054,
-29.2682655958051));
#18559=CARTESIAN_POINT('',(-45.5252381517553,-13.5169045823054,-31.689118544074));
#18560=CARTESIAN_POINT('',(5.05982447571381,-13.5169045823054,-15.0086664655392));
#18561=CARTESIAN_POINT('',(-46.4522196376124,-14.4544045724558,-31.9947911962243));
#18562=CARTESIAN_POINT('Origin',(1220.3812882873,-1402.30169205975,385.744251110796));
#18563=CARTESIAN_POINT('',(5.05982447571381,-14.4544045823054,-15.0086664655392));
#18564=CARTESIAN_POINT('Origin',(6.93398483519394,-11.0169045823054,-20.6922365937267));
#18565=CARTESIAN_POINT('',(-33.623065834026,-12.8919045823054,-34.0659462422992));
#18566=CARTESIAN_POINT('',(-33.623065834026,-11.3294045823054,-34.0659462422992));
#18567=CARTESIAN_POINT('',(-33.623065834026,-11.0169045823054,-34.0659462422992));
#18568=CARTESIAN_POINT('',(6.93398483519395,-11.3294045823054,-20.6922365937267));
#18569=CARTESIAN_POINT('',(6.93398483519401,-11.3294045823054,-20.6922365937267));
#18570=CARTESIAN_POINT('',(6.93398483519395,-14.4544045823054,-20.6922365937267));
#18571=CARTESIAN_POINT('',(6.93398483519395,-11.0169045823054,-20.6922365937267));
#18572=CARTESIAN_POINT('',(-42.3443728514905,-14.4544045474394,-36.9418020030986));
#18573=CARTESIAN_POINT('',(-43.2465796510443,-14.4544045823054,-37.2393051888733));
#18574=CARTESIAN_POINT('',(-41.3745486405956,-13.5169045823054,-36.6220019389143));
#18575=CARTESIAN_POINT('Origin',(530.074081345601,-669.972711183026,151.813496477798));
#18576=CARTESIAN_POINT('',(-34.2908051207842,-13.5169045823054,-34.2861336374548));
#18577=CARTESIAN_POINT('',(-34.1087963291987,-13.5169045823054,-34.2261161388451));
#18578=CARTESIAN_POINT('Ctrl Pts',(-33.6230658340261,-12.8919045823054,
-34.0659462422992));
#18579=CARTESIAN_POINT('Ctrl Pts',(-33.6230658340261,-12.9240089539717,
-34.0659462422992));
#18580=CARTESIAN_POINT('Ctrl Pts',(-33.6256783091265,-12.9558011838052,
-34.066807707393));
#18581=CARTESIAN_POINT('Ctrl Pts',(-33.630814373568,-12.987039082263,-34.0685013274527));
#18582=CARTESIAN_POINT('Ctrl Pts',(-33.6360742275513,-13.019029877259,-34.0702357671816));
#18583=CARTESIAN_POINT('Ctrl Pts',(-33.6439806080066,-13.0504387215005,
-34.0728429004626));
#18584=CARTESIAN_POINT('Ctrl Pts',(-33.6543863713838,-13.0810143824775,
-34.0762742066298));
#18585=CARTESIAN_POINT('Ctrl Pts',(-33.6616724148322,-13.1024232485325,
-34.0786767834434));
#18586=CARTESIAN_POINT('Ctrl Pts',(-33.6701827293343,-13.1234238076968,
-34.0814830643069));
#18587=CARTESIAN_POINT('Ctrl Pts',(-33.6798531673154,-13.1439346499851,
-34.0846718965225));
#18588=CARTESIAN_POINT('Ctrl Pts',(-33.6798967429698,-13.1440270732421,
-34.0846862656184));
#18589=CARTESIAN_POINT('Ctrl Pts',(-33.6799403391956,-13.1441194808469,
-34.0847006414977));
#18590=CARTESIAN_POINT('Ctrl Pts',(-33.6799839559855,-13.1442118727969,
-34.084715024158));
#18591=CARTESIAN_POINT('Ctrl Pts',(-33.7146023119914,-13.2175427490685,
-34.0961304459929));
#18592=CARTESIAN_POINT('Ctrl Pts',(-33.7623907865948,-13.2814833076131,
-34.1118887216388));
#18593=CARTESIAN_POINT('Ctrl Pts',(-33.8207273804618,-13.3355724234755,
-34.1311252453856));
#18594=CARTESIAN_POINT('Ctrl Pts',(-33.8247694769424,-13.3393202155624,
-34.1324581289117));
#18595=CARTESIAN_POINT('Ctrl Pts',(-33.8288622293082,-13.3430206975035,
-34.1338077162437));
#18596=CARTESIAN_POINT('Ctrl Pts',(-33.8330047712751,-13.3466737099125,
-34.135173721724));
#18597=CARTESIAN_POINT('Ctrl Pts',(-33.8330549933399,-13.3467179971708,
-34.1351902824773));
#18598=CARTESIAN_POINT('Ctrl Pts',(-33.8331052202197,-13.3467622754629,
-34.1352068448184));
#18599=CARTESIAN_POINT('Ctrl Pts',(-33.833155451914,-13.3468065447896,-34.1352234087471));
#18600=CARTESIAN_POINT('Ctrl Pts',(-33.8971289942698,-13.4031865990188,
-34.156318719343));
#18601=CARTESIAN_POINT('Ctrl Pts',(-33.9688832036395,-13.4450083105498,
-34.179979709142));
#18602=CARTESIAN_POINT('Ctrl Pts',(-34.0475696763434,-13.4738659092279,
-34.2059266165677));
#18603=CARTESIAN_POINT('Ctrl Pts',(-34.1262997844951,-13.5027395108376,
-34.2318879128062));
#18604=CARTESIAN_POINT('Ctrl Pts',(-34.2074475252744,-13.5169045582356,
-34.2586464247271));
#18605=CARTESIAN_POINT('Ctrl Pts',(-34.2908051207842,-13.5169045823054,
-34.2861336374548));
#18606=CARTESIAN_POINT('Origin',(0.0835265683620477,-6.01690458230549,0.0824317919394229));
#18607=CARTESIAN_POINT('',(-4.13722357323051,-6.1084342262812,-48.2627019018071));
#18608=CARTESIAN_POINT('',(-32.0390884399918,-6.10843371299758,-36.2934430895344));
#18609=CARTESIAN_POINT('Origin',(0.0835265683620477,-6.10843371318469,0.0824317919394229));
#18610=CARTESIAN_POINT('',(-39.1269295149477,-12.6709337131846,-38.6166213711206));
#18611=CARTESIAN_POINT('Ctrl Pts',(-32.0390884396323,-6.10843371318765,
-36.2934430901055));
#18612=CARTESIAN_POINT('Ctrl Pts',(-32.5225298437675,-6.54712953976947,
-36.4517920085165));
#18613=CARTESIAN_POINT('Ctrl Pts',(-33.0050570127847,-6.98698298247917,
-36.609758923213));
#18614=CARTESIAN_POINT('Ctrl Pts',(-33.4866867369723,-7.42790908709951,
-36.7674553177767));
#18615=CARTESIAN_POINT('Ctrl Pts',(-33.9664335523027,-7.86711141175758,
-36.924535205669));
#18616=CARTESIAN_POINT('Ctrl Pts',(-34.4452900133375,-8.30737802767764,
-37.0813467433358));
#18617=CARTESIAN_POINT('Ctrl Pts',(-34.9232986528203,-8.74862497312586,
-37.2379554426264));
#18618=CARTESIAN_POINT('Ctrl Pts',(-35.4003758146033,-9.18901207702346,
-37.3942589643555));
#18619=CARTESIAN_POINT('Ctrl Pts',(-35.8766085225511,-9.63037569350826,
-37.5503604966855));
#18620=CARTESIAN_POINT('Ctrl Pts',(-36.3520638137852,-10.0726323507299,
-37.7062796845329));
#18621=CARTESIAN_POINT('Ctrl Pts',(-36.826174045008,-10.5136378666659,-37.8617577779841));
#18622=CARTESIAN_POINT('Ctrl Pts',(-37.2995113121353,-10.9555313776728,
-38.0170545978434));
#18623=CARTESIAN_POINT('Ctrl Pts',(-37.7721657694013,-11.3982301183219,
-38.1721436168242));
#18624=CARTESIAN_POINT('Ctrl Pts',(-38.2243455601687,-11.8217518281934,
-38.3205144172578));
#18625=CARTESIAN_POINT('Ctrl Pts',(-38.675900600911,-12.2460105160849,-38.4686947735073));
#18626=CARTESIAN_POINT('Ctrl Pts',(-39.1269295149477,-12.6709337131846,
-38.6166213711206));
#18627=CARTESIAN_POINT('',(-40.2726585348436,-13.2959337131846,-38.3325384971017));
#18628=CARTESIAN_POINT('Ctrl Pts',(-40.2726585348435,-13.2959337131846,
-38.3325384971018));
#18629=CARTESIAN_POINT('Ctrl Pts',(-40.2396336815792,-13.2959336603245,
-38.3672321109749));
#18630=CARTESIAN_POINT('Ctrl Pts',(-40.203931177053,-13.2916605128733,-38.3984485109642));
#18631=CARTESIAN_POINT('Ctrl Pts',(-40.1665336587125,-13.2840750781675,
-38.4265635639867));
#18632=CARTESIAN_POINT('Ctrl Pts',(-40.1233293436535,-13.2753118359676,
-38.4590441044767));
#18633=CARTESIAN_POINT('Ctrl Pts',(-40.0778617899977,-13.262127307608,-38.487385683028));
#18634=CARTESIAN_POINT('Ctrl Pts',(-40.0316115052285,-13.2459526170016,
-38.512130144461));
#18635=CARTESIAN_POINT('Ctrl Pts',(-40.0180845510295,-13.2412219585828,
-38.5193672284736));
#18636=CARTESIAN_POINT('Ctrl Pts',(-40.0044905078433,-13.2362352705449,
-38.5262963859028));
#18637=CARTESIAN_POINT('Ctrl Pts',(-39.9908662064094,-13.2310278528739,
-38.5329306481798));
#18638=CARTESIAN_POINT('Ctrl Pts',(-39.9908210967496,-13.2310106112677,
-38.5329526140264));
#18639=CARTESIAN_POINT('Ctrl Pts',(-39.9907759867598,-13.230993367242,-38.5329745766387));
#18640=CARTESIAN_POINT('Ctrl Pts',(-39.9907308764414,-13.2309761207982,
-38.5329965360173));
#18641=CARTESIAN_POINT('Ctrl Pts',(-39.9008654396959,-13.1966190321654,
-38.5767423843686));
#18642=CARTESIAN_POINT('Ctrl Pts',(-39.8096589826388,-13.1525556483329,
-38.6075525746423));
#18643=CARTESIAN_POINT('Ctrl Pts',(-39.7201449624174,-13.1028429779769,
-38.6282896284184));
#18644=CARTESIAN_POINT('Ctrl Pts',(-39.7095659381455,-13.0969677916652,
-38.6307403930549));
#18645=CARTESIAN_POINT('Ctrl Pts',(-39.6990105689488,-13.091013739855,-38.6330505050437));
#18646=CARTESIAN_POINT('Ctrl Pts',(-39.6884838737899,-13.0849875486837,
-38.6352247206687));
#18647=CARTESIAN_POINT('Ctrl Pts',(-39.6883620970893,-13.0849178354768,
-38.6352498727987));
#18648=CARTESIAN_POINT('Ctrl Pts',(-39.6882403231401,-13.0848481114876,
-38.6352750062405));
#18649=CARTESIAN_POINT('Ctrl Pts',(-39.6881185519542,-13.0847783767298,
-38.6353001210018));
#18650=CARTESIAN_POINT('Ctrl Pts',(-39.6633307896687,-13.0705831581647,
-38.6404124858695));
#18651=CARTESIAN_POINT('Ctrl Pts',(-39.6385397905417,-13.0558793142743,
-38.6447819668785));
#18652=CARTESIAN_POINT('Ctrl Pts',(-39.6138315388079,-13.0407301262923,
-38.6484136767956));
#18653=CARTESIAN_POINT('Ctrl Pts',(-39.576587090328,-13.0178947125452,-38.6538880031203));
#18654=CARTESIAN_POINT('Ctrl Pts',(-39.5395279799376,-12.9940463246918,
-38.6576871593004));
#18655=CARTESIAN_POINT('Ctrl Pts',(-39.5029368702493,-12.9693962501975,
-38.6598334969272));
#18656=CARTESIAN_POINT('Ctrl Pts',(-39.4663457605609,-12.9447461757032,
-38.6619798345541));
#18657=CARTESIAN_POINT('Ctrl Pts',(-39.4302226608903,-12.9192944015675,
-38.662473362689));
#18658=CARTESIAN_POINT('Ctrl Pts',(-39.3948503116026,-12.8932521061511,
-38.6613365091335));
#18659=CARTESIAN_POINT('Ctrl Pts',(-39.3647901092163,-12.8711207892725,
-38.6603703859144));
#18660=CARTESIAN_POINT('Ctrl Pts',(-39.3352090913624,-12.8485482515871,
-38.6582701011378));
#18661=CARTESIAN_POINT('Ctrl Pts',(-39.3061311012479,-12.8255048446002,
-38.6549739360498));
#18662=CARTESIAN_POINT('Ctrl Pts',(-39.2895870067339,-12.8123941618599,
-38.6530985634214));
#18663=CARTESIAN_POINT('Ctrl Pts',(-39.2732062544516,-12.7991308725972,
-38.6508352926566));
#18664=CARTESIAN_POINT('Ctrl Pts',(-39.2569980022231,-12.7857088195892,
-38.6481669486584));
#18665=CARTESIAN_POINT('Ctrl Pts',(-39.2280783717813,-12.7617604748022,
-38.6434059465941));
#18666=CARTESIAN_POINT('Ctrl Pts',(-39.1997054209728,-12.7373067239667,
-38.637357958912));
#18667=CARTESIAN_POINT('Ctrl Pts',(-39.1719053122653,-12.7123167139494,
-38.6299576805737));
#18668=CARTESIAN_POINT('Ctrl Pts',(-39.1567397038309,-12.6986840799665,
-38.6259206559431));
#18669=CARTESIAN_POINT('Ctrl Pts',(-39.1417450242042,-12.684891691096,-38.62148049444));
#18670=CARTESIAN_POINT('Ctrl Pts',(-39.1269295149477,-12.6709337131846,
-38.6166213711206));
#18671=CARTESIAN_POINT('',(-41.4413720390587,-13.2959337131846,-37.0661134559641));
#18672=CARTESIAN_POINT('Origin',(0.0835265683620477,-13.2959337131846,0.0824317919394229));
#18673=CARTESIAN_POINT('',(-42.868890621412,-14.6753754514262,-37.5345822714215));
#18674=CARTESIAN_POINT('Origin',(537.351619142406,-671.736419815441,133.622883040623));
#18675=CARTESIAN_POINT('',(-30.3451265715159,-14.675375306047,-48.2295436818698));
#18676=CARTESIAN_POINT('Origin',(0.0835265683620477,-14.6753754514262,0.0824317919394229));
#18677=CARTESIAN_POINT('Ctrl Pts',(-30.3451268039573,-14.6753748699083,
-48.2295440509134));
#18678=CARTESIAN_POINT('Ctrl Pts',(-29.4817793367662,-14.2165313285487,
-48.2310581461111));
#18679=CARTESIAN_POINT('Ctrl Pts',(-28.6133029132634,-13.7688961381484,
-48.2325674328801));
#18680=CARTESIAN_POINT('Ctrl Pts',(-27.7390368044124,-13.3339028932971,
-48.2340665432468));
#18681=CARTESIAN_POINT('Ctrl Pts',(-26.8896562709457,-12.9112915274605,
-48.2355229821389));
#18682=CARTESIAN_POINT('Ctrl Pts',(-26.0348108991148,-12.5006127526482,
-48.2369698132499));
#18683=CARTESIAN_POINT('Ctrl Pts',(-25.1739206375199,-12.103139198304,-48.2384019171115));
#18684=CARTESIAN_POINT('Ctrl Pts',(-24.8546574836089,-11.9557352070903,
-48.2389330161563));
#18685=CARTESIAN_POINT('Ctrl Pts',(-24.5345632331656,-11.8101469176186,
-48.239462087945));
#18686=CARTESIAN_POINT('Ctrl Pts',(-24.2136092696096,-11.6664376689277,
-48.2399888653929));
#18687=CARTESIAN_POINT('Ctrl Pts',(-24.1814220403843,-11.6520256252871,
-48.2400416938617));
#18688=CARTESIAN_POINT('Ctrl Pts',(-24.1492261126984,-11.6376325718391,
-48.240094498393));
#18689=CARTESIAN_POINT('Ctrl Pts',(-24.1170214462916,-11.6232585917442,
-48.240147278535));
#18690=CARTESIAN_POINT('Ctrl Pts',(-23.3441962477099,-11.2783218089513,
-48.2414138596948));
#18691=CARTESIAN_POINT('Ctrl Pts',(-22.566326590449,-10.9443666876212,-48.242664919568));
#18692=CARTESIAN_POINT('Ctrl Pts',(-21.7829239437866,-10.6225428072345,
-48.2438912877425));
#18693=CARTESIAN_POINT('Ctrl Pts',(-21.51280683996,-10.511577986165,-48.2443141392875));
#18694=CARTESIAN_POINT('Ctrl Pts',(-21.2420321676512,-10.4020550272744,
-48.2447340583014));
#18695=CARTESIAN_POINT('Ctrl Pts',(-20.9705806532939,-10.2940198074422,
-48.2451506784524));
#18696=CARTESIAN_POINT('Ctrl Pts',(-20.9543075471883,-10.2875432600572,
-48.2451756541979));
#18697=CARTESIAN_POINT('Ctrl Pts',(-20.9380317506347,-10.2810720136179,
-48.2452006183239));
#18698=CARTESIAN_POINT('Ctrl Pts',(-20.9217533048638,-10.274606093873,-48.2452255706762));
#18699=CARTESIAN_POINT('Ctrl Pts',(-20.4658680493351,-10.0935250793455,
-48.2459243726188));
#18700=CARTESIAN_POINT('Ctrl Pts',(-20.0079420683559,-9.91663263844885,
-48.2466145458997));
#18701=CARTESIAN_POINT('Ctrl Pts',(-19.5482069672317,-9.74425107317444,
-48.2472938116465));
#18702=CARTESIAN_POINT('Ctrl Pts',(-19.1078591483264,-9.57913893337382,
-48.2479444323828));
#18703=CARTESIAN_POINT('Ctrl Pts',(-18.6658501180235,-9.41816464536872,
-48.2485850503878));
#18704=CARTESIAN_POINT('Ctrl Pts',(-18.2223680178153,-9.26165511807674,
-48.2492135577687));
#18705=CARTESIAN_POINT('Ctrl Pts',(-18.0367076056395,-9.19613359345863,
-48.249476677609));
#18706=CARTESIAN_POINT('Ctrl Pts',(-17.8507889517602,-9.1313951604908,-48.2497376732635));
#18707=CARTESIAN_POINT('Ctrl Pts',(-17.6646259020658,-9.06746659619127,
-48.2499963816089));
#18708=CARTESIAN_POINT('Ctrl Pts',(-17.6610247716672,-9.0662299646652,-48.2500013860525));
#18709=CARTESIAN_POINT('Ctrl Pts',(-17.6574235801825,-9.06499364665118,
-48.2500063895844));
#18710=CARTESIAN_POINT('Ctrl Pts',(-17.6538223280036,-9.06375764243259,
-48.2500113922032));
#18711=CARTESIAN_POINT('Ctrl Pts',(-16.7856068602355,-8.76577296168996,
-48.2512174590869));
#18712=CARTESIAN_POINT('Ctrl Pts',(-15.912148956512,-8.48534970224392,-48.2523723989392));
#18713=CARTESIAN_POINT('Ctrl Pts',(-15.0330164282587,-8.22405492508236,
-48.2534642885946));
#18714=CARTESIAN_POINT('Ctrl Pts',(-14.806881310249,-8.15684330070286,-48.253745150226));
#18715=CARTESIAN_POINT('Ctrl Pts',(-14.5803706794578,-8.09089757133394,
-48.2540218379708));
#18716=CARTESIAN_POINT('Ctrl Pts',(-14.3534770702195,-8.02624496071179,
-48.2542941443476));
#18717=CARTESIAN_POINT('Ctrl Pts',(-13.8350297076525,-7.87851503754358,
-48.2549163589764));
#18718=CARTESIAN_POINT('Ctrl Pts',(-13.3142751741925,-7.73745329658206,
-48.2555159228595));
#18719=CARTESIAN_POINT('Ctrl Pts',(-12.791639486122,-7.60353311379642,-48.2560895730586));
#18720=CARTESIAN_POINT('Ctrl Pts',(-12.289610378971,-7.47489316186051,-48.2566406052667));
#18721=CARTESIAN_POINT('Ctrl Pts',(-11.7858455328013,-7.35284273127803,
-48.2571677252085));
#18722=CARTESIAN_POINT('Ctrl Pts',(-11.2807318563516,-7.2377561198086,-48.2576681937696));
#18723=CARTESIAN_POINT('Ctrl Pts',(-11.1005031779102,-7.19669227842297,
-48.257846765033));
#18724=CARTESIAN_POINT('Ctrl Pts',(-10.9201009710423,-7.15651419448117,
-48.2580219465406));
#18725=CARTESIAN_POINT('Ctrl Pts',(-10.7395560300484,-7.1172401230684,-48.2581936074901));
#18726=CARTESIAN_POINT('Ctrl Pts',(-9.65047242716134,-6.88033098034299,
-48.2592291010593));
#18727=CARTESIAN_POINT('Ctrl Pts',(-8.5559911237925,-6.67627260249923,-48.2601366679466));
#18728=CARTESIAN_POINT('Ctrl Pts',(-7.45572847150844,-6.50737682460517,
-48.2608950409414));
#18729=CARTESIAN_POINT('Ctrl Pts',(-6.35546581922438,-6.33848104671112,
-48.2616534139363));
#18730=CARTESIAN_POINT('Ctrl Pts',(-5.24942178111159,-6.20474805617039,
-48.2622625913705));
#18731=CARTESIAN_POINT('Ctrl Pts',(-4.13722359825051,-6.10843510301128,
-48.262701707337));
#18732=CARTESIAN_POINT('Origin',(0.0835265683620477,-8.56135981233827,0.0824317919394229));
#18733=CARTESIAN_POINT('',(-39.2593077130565,-8.46983068145907,37.6646495687126));
#18734=CARTESIAN_POINT('',(-35.984538282875,-3.84038894321748,34.3905421902094));
#18735=CARTESIAN_POINT('Ctrl Pts',(-39.2593077130565,-8.46983068145907,
37.6646495687126));
#18736=CARTESIAN_POINT('Ctrl Pts',(-39.1551178801364,-8.32253590125116,
37.5604790152082));
#18737=CARTESIAN_POINT('Ctrl Pts',(-39.0509278602785,-8.17524127521395,
37.4563084306819));
#18738=CARTESIAN_POINT('Ctrl Pts',(-38.5299768032981,-7.43876893481715,
36.9354553491631));
#18739=CARTESIAN_POINT('Ctrl Pts',(-38.1132128963777,-6.84959358714927,
36.5187723760457));
#18740=CARTESIAN_POINT('Ctrl Pts',(-37.1258164844502,-5.45373818194081,
35.5315743934649));
#18741=CARTESIAN_POINT('Ctrl Pts',(-36.5551810303102,-4.64706055617428,
34.961058895205));
#18742=CARTESIAN_POINT('Ctrl Pts',(-35.984538282875,-3.84038894321748,34.3905421902094));
#18743=CARTESIAN_POINT('',(-35.9845382828747,-3.84038894321748,-34.2256786063309));
#18744=CARTESIAN_POINT('Origin',(0.0835265683620477,-3.84038894321747,0.0824317919394229));
#18745=CARTESIAN_POINT('',(-39.2593077130561,-8.46983068145907,-37.4997859848342));
#18746=CARTESIAN_POINT('Ctrl Pts',(-35.9845382828747,-3.84038894321748,
-34.2256786063309));
#18747=CARTESIAN_POINT('Ctrl Pts',(-36.0887325923582,-3.98768003220409,
-34.3298499015818));
#18748=CARTESIAN_POINT('Ctrl Pts',(-36.1929266581883,-4.13497132206384,
-34.4340211565197));
#18749=CARTESIAN_POINT('Ctrl Pts',(-36.7138958007323,-4.87142874967365,
-34.9548772348263));
#18750=CARTESIAN_POINT('Ctrl Pts',(-37.1306673216522,-5.46059781902367,
-35.3715614696892));
#18751=CARTESIAN_POINT('Ctrl Pts',(-38.1180656564427,-6.85645163869055,
-36.358759770908));
#18752=CARTESIAN_POINT('Ctrl Pts',(-38.688689482493,-7.66313885272879,-36.9292733421747));
#18753=CARTESIAN_POINT('Ctrl Pts',(-39.2593077130561,-8.46983068145907,
-37.4997859848342));
#18754=CARTESIAN_POINT('',(-49.8065937787556,-8.46983068145906,-21.6260364650814));
#18755=CARTESIAN_POINT('Origin',(0.0835265683620477,-8.46983068145906,0.0824317919394229));
#18756=CARTESIAN_POINT('',(-49.8065937787556,-8.46983068145906,21.7909000489602));
#18757=CARTESIAN_POINT('Ctrl Pts',(-49.8065937787556,-8.46983068145906,
-21.6260364650814));
#18758=CARTESIAN_POINT('Ctrl Pts',(-49.8091724689568,-7.78020213595473,
-19.8916770737466));
#18759=CARTESIAN_POINT('Ctrl Pts',(-49.8116222102493,-7.15174092367616,
-18.13538723326));
#18760=CARTESIAN_POINT('Ctrl Pts',(-49.8160494956856,-6.04804272442583,
-14.5965921523776));
#18761=CARTESIAN_POINT('Ctrl Pts',(-49.8180308842616,-5.57158091815884,
-12.8110043255947));
#18762=CARTESIAN_POINT('Ctrl Pts',(-49.8213344689701,-4.79205582539579,
-9.20258923968633));
#18763=CARTESIAN_POINT('Ctrl Pts',(-49.8226553391186,-4.48906686350367,
-7.3797460175301));
#18764=CARTESIAN_POINT('Ctrl Pts',(-49.8240081829567,-4.18101117599353,
-4.61403398685641));
#18765=CARTESIAN_POINT('Ctrl Pts',(-49.8243546591215,-4.10271637230149,
-3.68689182696108));
#18766=CARTESIAN_POINT('Ctrl Pts',(-49.8248218054713,-3.99733451725048,
-1.82160999461689));
#18767=CARTESIAN_POINT('Ctrl Pts',(-49.8249413755347,-3.97048844752839,
-0.88414976855677));
#18768=CARTESIAN_POINT('Ctrl Pts',(-49.8249557340184,-3.96725979794587,
3.77506613399273));
#18769=CARTESIAN_POINT('Ctrl Pts',(-49.8230647514948,-4.38426661992436,
7.45640245004576));
#18770=CARTESIAN_POINT('Ctrl Pts',(-49.818921517886,-5.36130666529405,12.0080656973011));
#18771=CARTESIAN_POINT('Ctrl Pts',(-49.8180052418649,-5.57963087290763,
12.9171167524008));
#18772=CARTESIAN_POINT('Ctrl Pts',(-49.8160296339025,-6.05753886911523,
14.7247229136368));
#18773=CARTESIAN_POINT('Ctrl Pts',(-49.8149721493814,-6.31667893722832,
15.6219036997713));
#18774=CARTESIAN_POINT('Ctrl Pts',(-49.8116301976253,-7.14963222024195,
18.2952277610572));
#18775=CARTESIAN_POINT('Ctrl Pts',(-49.8091774529085,-7.77886925953041,
20.0531885824263));
#18776=CARTESIAN_POINT('Ctrl Pts',(-49.8065937787556,-8.46983068145906,
21.7909000489602));
#18777=CARTESIAN_POINT('Origin',(0.0835265683620477,-8.46983068145906,0.0824317919394229));
#18778=CARTESIAN_POINT('Origin',(0.0835265683620477,11.4830954176946,0.0824317919394229));
#18779=CARTESIAN_POINT('',(-35.918219620459,-3.61941807409668,34.3274595712494));
#18780=CARTESIAN_POINT('',(-35.918219620459,11.9341984494201,34.3274595712494));
#18781=CARTESIAN_POINT('',(-35.918219620459,11.4830954176946,34.3274595712494));
#18782=CARTESIAN_POINT('',(-35.9182196204586,11.9341984494201,-34.1625959873709));
#18783=CARTESIAN_POINT('Origin',(0.0835265683620477,11.9341984494201,0.0824317919394229));
#18784=CARTESIAN_POINT('',(-35.9182196204586,-3.61941807409668,-34.1625959873709));
#18785=CARTESIAN_POINT('',(-35.9182196204586,11.4830954176946,-34.1625959873709));
#18786=CARTESIAN_POINT('Origin',(0.0835265683620477,-3.61941807409668,0.0824317919394229));
#18787=CARTESIAN_POINT('Origin',(0.0835265683620477,11.4830954176946,0.0824317919394229));
#18788=CARTESIAN_POINT('Origin',(0.0835265683620477,11.9341984494201,0.0824317919394229));
#18789=CARTESIAN_POINT('Origin',(0.0835265683620477,-3.61941807409668,0.0824317919394229));
#18790=CARTESIAN_POINT('Origin',(0.0835265683620477,12.0636401876617,0.0824317919394229));
#18791=CARTESIAN_POINT('',(-36.6066544046101,13.0346110567823,-34.8476596904499));
#18792=CARTESIAN_POINT('',(-35.9845382828753,12.1551693185412,-34.2256786063306));
#18793=CARTESIAN_POINT('',(-36.6066544046107,13.0346110567825,-34.8476596904497));
#18794=CARTESIAN_POINT('',(-35.9845382828754,12.1551693185417,34.3905421902101));
#18795=CARTESIAN_POINT('Origin',(0.0835265683620477,12.1551693185409,0.0824317919394229));
#18796=CARTESIAN_POINT('',(-36.6066544046109,13.0346110567825,35.0125232743281));
#18797=CARTESIAN_POINT('',(-35.984538282875,12.1551693185409,34.3905421902094));
#18798=CARTESIAN_POINT('',(-49.8216584885785,13.0346110567825,8.78606179499423));
#18799=CARTESIAN_POINT('Origin',(0.0835265683620477,13.0346110567825,0.0824317919394229));
#18800=CARTESIAN_POINT('',(-49.8216584885785,13.0346110567825,-8.6211982111154));
#18801=CARTESIAN_POINT('Ctrl Pts',(-49.8216584885785,13.0346110567825,8.78606179499423));
#18802=CARTESIAN_POINT('Ctrl Pts',(-49.8223976721169,12.8633426645386,7.78497558757201));
#18803=CARTESIAN_POINT('Ctrl Pts',(-49.8230202078243,12.7204977856027,6.78145983735361));
#18804=CARTESIAN_POINT('Ctrl Pts',(-49.8235176993747,12.607033826209,5.77542487233127));
#18805=CARTESIAN_POINT('Ctrl Pts',(-49.8240131775891,12.4940290526656,4.77346130604461));
#18806=CARTESIAN_POINT('Ctrl Pts',(-49.8243846217383,12.4101678841265,3.76899887262193));
#18807=CARTESIAN_POINT('Ctrl Pts',(-49.8246240837851,12.3563452055187,2.76195712956022));
#18808=CARTESIAN_POINT('Ctrl Pts',(-49.8248351469452,12.308905601697,1.87434501959917));
#18809=CARTESIAN_POINT('Ctrl Pts',(-49.8249436813649,12.2848014527005,0.984729221390203));
#18810=CARTESIAN_POINT('Ctrl Pts',(-49.824944469213,12.2846123568863,0.0930599517194889));
#18811=CARTESIAN_POINT('Ctrl Pts',(-49.8249444697293,12.2846122329701,0.0924756330936691));
#18812=CARTESIAN_POINT('Ctrl Pts',(-49.8249444701992,12.284612119341,0.0918913167795029));
#18813=CARTESIAN_POINT('Ctrl Pts',(-49.8249444706228,12.2846120159986,0.0913070027769935));
#18814=CARTESIAN_POINT('Ctrl Pts',(-49.8249449290864,12.284500162369,-0.541130544723481));
#18815=CARTESIAN_POINT('Ctrl Pts',(-49.8248910995487,12.2964431061466,-1.17335603026734));
#18816=CARTESIAN_POINT('Ctrl Pts',(-49.8247846280076,12.3202812996977,-1.80503154627235));
#18817=CARTESIAN_POINT('Ctrl Pts',(-49.8246764726378,12.3444964900669,-2.44669689892658));
#18818=CARTESIAN_POINT('Ctrl Pts',(-49.8245139977477,12.3809861187555,-3.08779471686519));
#18819=CARTESIAN_POINT('Ctrl Pts',(-49.8242991879303,12.4295292879082,-3.72797704193668));
#18820=CARTESIAN_POINT('Ctrl Pts',(-49.8240822089778,12.4785626427164,-4.37462388504563));
#18821=CARTESIAN_POINT('Ctrl Pts',(-49.8238118339164,12.5398940970328,-5.02033662533801));
#18822=CARTESIAN_POINT('Ctrl Pts',(-49.8234903564628,12.6132427399653,-5.66476341594209));
#18823=CARTESIAN_POINT('Ctrl Pts',(-49.8231633549434,12.6878517597083,-6.32026363000007));
#18824=CARTESIAN_POINT('Ctrl Pts',(-49.8227834807396,12.774894442269,-6.97443328341991));
#18825=CARTESIAN_POINT('Ctrl Pts',(-49.8223533878003,12.8740215067224,-7.62690954257758));
#18826=CARTESIAN_POINT('Ctrl Pts',(-49.8221346202543,12.9244426660921,-7.95879276366675));
#18827=CARTESIAN_POINT('Ctrl Pts',(-49.8219028634911,12.9779895328919,-8.29023798040707));
#18828=CARTESIAN_POINT('Ctrl Pts',(-49.8216584885785,13.0346110567825,-8.62119821111539));
#18829=CARTESIAN_POINT('Origin',(0.0835265683620477,13.0346110567825,0.0824317919394229));
#18830=CARTESIAN_POINT('Origin',(0.0835265683620477,12.0636401876617,0.0824317919394229));
#18831=CARTESIAN_POINT('',(35.0136180507514,13.0346110567824,-36.6077491810329));
#18832=CARTESIAN_POINT('',(34.3916369666323,12.155169318541,-35.9856330592975));
#18833=CARTESIAN_POINT('',(35.0136180507513,13.0346110567825,-36.6077491810332));
#18834=CARTESIAN_POINT('',(-34.224583829909,12.1551693185417,-35.9856330592976));
#18835=CARTESIAN_POINT('Origin',(0.0835265683620477,12.1551693185409,0.0824317919394229));
#18836=CARTESIAN_POINT('',(-34.8465649140271,13.0346110567825,-36.6077491810333));
#18837=CARTESIAN_POINT('',(-34.2245838299083,12.1551693185409,-35.9856330592973));
#18838=CARTESIAN_POINT('',(-8.62010343469281,13.0346110567825,-49.8227532650011));
#18839=CARTESIAN_POINT('Origin',(0.0835265683620477,13.0346110567825,0.0824317919394229));
#18840=CARTESIAN_POINT('',(8.78715657141686,13.0346110567825,-49.8227532650011));
#18841=CARTESIAN_POINT('Ctrl Pts',(-8.62010343469281,13.0346110567825,-49.8227532650012));
#18842=CARTESIAN_POINT('Ctrl Pts',(-7.75844751180745,12.8871967547116,-49.8233894957965));
#18843=CARTESIAN_POINT('Ctrl Pts',(-6.89456295486043,12.7606786215472,-49.8239416754741));
#18844=CARTESIAN_POINT('Ctrl Pts',(-6.02838145460376,12.6558408127419,-49.824401445282));
#18845=CARTESIAN_POINT('Ctrl Pts',(-5.45188904034233,12.5860653655796,-49.8247074478998));
#18846=CARTESIAN_POINT('Ctrl Pts',(-4.87437937103337,12.5258925149287,-49.8249725252371));
#18847=CARTESIAN_POINT('Ctrl Pts',(-4.29583487440298,12.4755408811181,-49.8251943106573));
#18848=CARTESIAN_POINT('Ctrl Pts',(-4.29265435629997,12.4752640756454,-49.825195529911));
#18849=CARTESIAN_POINT('Ctrl Pts',(-4.28947377822589,12.4749875690291,-49.825196747846));
#18850=CARTESIAN_POINT('Ctrl Pts',(-4.28629314051264,12.4747113612835,-49.8251979644619));
#18851=CARTESIAN_POINT('Ctrl Pts',(-3.86378044609719,12.438020203936,-49.8253595784886));
#18852=CARTESIAN_POINT('Ctrl Pts',(-3.44050667647658,12.4066244502033,-49.8254981885894));
#18853=CARTESIAN_POINT('Ctrl Pts',(-3.01673651081865,12.3805167222789,-49.8256136721586));
#18854=CARTESIAN_POINT('Ctrl Pts',(-2.58887894632784,12.3541571769655,-49.8257302696038));
#18855=CARTESIAN_POINT('Ctrl Pts',(-2.1605141706406,12.3331879704997,-49.8258232933164));
#18856=CARTESIAN_POINT('Ctrl Pts',(-1.73189789250613,12.3176520559965,-49.8258923976071));
#18857=CARTESIAN_POINT('Ctrl Pts',(-1.31087896549224,12.3023915202026,-49.8259602770036));
#18858=CARTESIAN_POINT('Ctrl Pts',(-0.889616220769264,12.2923733967901,
-49.8260050775384));
#18859=CARTESIAN_POINT('Ctrl Pts',(-0.468353474323579,12.2876877721295,
-49.826026253509));
#18860=CARTESIAN_POINT('Ctrl Pts',(-0.284460199973243,12.2856423625402,
-49.8260354974277));
#18861=CARTESIAN_POINT('Ctrl Pts',(-0.100567045923406,12.2846137392999,
-49.8260402366669));
#18862=CARTESIAN_POINT('Ctrl Pts',(0.0833047732558613,12.2846124143579,
-49.8260404123309));
#18863=CARTESIAN_POINT('Ctrl Pts',(0.0872263894601545,12.2846123860995,
-49.8260404160775));
#18864=CARTESIAN_POINT('Ctrl Pts',(0.0911479501779279,12.2846128251744,
-49.8260404177092));
#18865=CARTESIAN_POINT('Ctrl Pts',(0.0950694548097551,12.2846137316609,
-49.8260404172258));
#18866=CARTESIAN_POINT('Ctrl Pts',(1.25176284833155,12.2848811103974,-49.8260402746341));
#18867=CARTESIAN_POINT('Ctrl Pts',(2.40624585563398,12.3254286614646,-49.8258561458821));
#18868=CARTESIAN_POINT('Ctrl Pts',(3.55854196309821,12.4051717612045,-49.8255020546121));
#18869=CARTESIAN_POINT('Ctrl Pts',(3.85537063385761,12.4257133894758,-49.8254108415634));
#18870=CARTESIAN_POINT('Ctrl Pts',(4.15205421108766,12.4488556287928,-49.825308352493));
#18871=CARTESIAN_POINT('Ctrl Pts',(4.44859314096187,12.4745793828298,-49.825194832241));
#18872=CARTESIAN_POINT('Ctrl Pts',(4.99533228329415,12.5220071631409,-49.8249855310028));
#18873=CARTESIAN_POINT('Ctrl Pts',(5.54164564607858,12.578220119787,-49.8247383049551));
#18874=CARTESIAN_POINT('Ctrl Pts',(6.08714324293855,12.643043269177,-49.8244545700796));
#18875=CARTESIAN_POINT('Ctrl Pts',(6.64034176769106,12.7087815434036,-49.824166829647));
#18876=CARTESIAN_POINT('Ctrl Pts',(7.19270133263586,12.7833747882158,-49.823841543167));
#18877=CARTESIAN_POINT('Ctrl Pts',(7.74382117374416,12.8665869343007,-49.8234804167539));
#18878=CARTESIAN_POINT('Ctrl Pts',(8.09212801691555,12.9191768752799,-49.8232521854481));
#18879=CARTESIAN_POINT('Ctrl Pts',(8.43993980678189,12.9752083234332,-49.8230096434377));
#18880=CARTESIAN_POINT('Ctrl Pts',(8.78715657141686,13.0346110567825,-49.8227532650012));
#18881=CARTESIAN_POINT('Origin',(0.0835265683620477,13.0346110567825,0.0824317919394229));
#18882=CARTESIAN_POINT('Origin',(-68.3539734316379,-8.56135981233827,0.0824317919394229));
#18883=CARTESIAN_POINT('',(-22.6217205869088,-8.56135981233827,-49.6050682080606));
#18884=CARTESIAN_POINT('',(-44.2914734316379,-8.56135981233827,-49.6050682080606));
#18885=CARTESIAN_POINT('',(-68.353973431638,-8.56135981233827,-49.6050682080606));
#18886=CARTESIAN_POINT('',(-49.603973431638,-8.56135981233827,-44.2925682080605));
#18887=CARTESIAN_POINT('Origin',(-44.291473431638,-8.56135981233827,-44.2925682080606));
#18888=CARTESIAN_POINT('',(-49.6039734316379,-8.56135981233827,-22.6228153633314));
#18889=CARTESIAN_POINT('',(-49.603973431638,-8.56135981233827,0.0824317919394229));
#18890=CARTESIAN_POINT('',(-39.4190920287328,-8.56135981233827,-37.6524198521891));
#18891=CARTESIAN_POINT('Origin',(0.0835265683620477,-8.56135981233827,0.0824317919394229));
#18892=CARTESIAN_POINT('',(-40.5751133498644,-8.56135981233827,-38.8084411733207));
#18893=CARTESIAN_POINT('',(-37.6513250757665,-8.56135981233827,-39.4201868051554));
#18894=CARTESIAN_POINT('',(-37.5642074513747,-8.56135981233827,-39.3330691807637));
#18895=CARTESIAN_POINT('Origin',(0.0835265683620477,-8.56135981233827,0.0824317919394229));
#18896=CARTESIAN_POINT('Origin',(-50.666473431638,13.1261401876617,0.0824317919394229));
#18897=CARTESIAN_POINT('',(-49.603973431638,13.1261401876617,-10.8660811365418));
#18898=CARTESIAN_POINT('',(-49.603973431638,13.1261401876617,-44.2925682080605));
#18899=CARTESIAN_POINT('',(-49.603973431638,13.1261401876617,0.0824317919394229));
#18900=CARTESIAN_POINT('',(-44.2914734316379,13.1261401876617,-49.6050682080606));
#18901=CARTESIAN_POINT('Origin',(-44.291473431638,13.1261401876617,-44.2925682080606));
#18902=CARTESIAN_POINT('',(-10.8649863601192,13.1261401876617,-49.6050682080606));
#18903=CARTESIAN_POINT('',(-50.666473431638,13.1261401876617,-49.6050682080606));
#18904=CARTESIAN_POINT('',(-34.9989290209752,13.1261401876617,-36.7677907503642));
#18905=CARTESIAN_POINT('Origin',(0.0835265683620477,13.1261401876617,0.0824317919394229));
#18906=CARTESIAN_POINT('',(-38.8073463968981,13.1261401876617,-40.576208126287));
#18907=CARTESIAN_POINT('',(-38.8073463968981,13.1261401876617,-40.576208126287));
#18908=CARTESIAN_POINT('',(-40.5751133498644,13.1261401876617,-38.8084411733207));
#18909=CARTESIAN_POINT('Origin',(-39.6912298733813,13.1261401876617,-39.6923246498039));
#18910=CARTESIAN_POINT('',(-36.7666959739416,13.1261401876617,-35.0000237973978));
#18911=CARTESIAN_POINT('',(-36.6799025696119,13.1261401876617,-34.9132303930681));
#18912=CARTESIAN_POINT('Origin',(0.0835265683620477,13.1261401876617,0.0824317919394229));
#18913=CARTESIAN_POINT('Origin',(0.0835265683620477,16.4830954176946,-49.9175682080606));
#18914=CARTESIAN_POINT('',(22.7887737236329,-8.87385981233827,-49.9175682080606));
#18915=CARTESIAN_POINT('',(21.7038295264614,-8.69080155057986,-49.9175682080606));
#18916=CARTESIAN_POINT('Ctrl Pts',(22.7887737236329,-8.87385981233827,-49.9175682080606));
#18917=CARTESIAN_POINT('Ctrl Pts',(22.7188372925805,-8.87385981188611,-49.9175682080606));
#18918=CARTESIAN_POINT('Ctrl Pts',(22.6488692798012,-8.87185808464265,-49.9175682080607));
#18919=CARTESIAN_POINT('Ctrl Pts',(22.5790744235432,-8.86782837150082,-49.9175682080605));
#18920=CARTESIAN_POINT('Ctrl Pts',(22.5081988311883,-8.8637362604018,-49.9175682080604));
#18921=CARTESIAN_POINT('Ctrl Pts',(22.4375001565979,-8.85755327620009,-49.9175682080604));
#18922=CARTESIAN_POINT('Ctrl Pts',(22.3671724444924,-8.84920383564249,-49.9175682080574));
#18923=CARTESIAN_POINT('Ctrl Pts',(22.3238948570106,-8.8440658376423,-49.9175682080556));
#18924=CARTESIAN_POINT('Ctrl Pts',(22.2807574487412,-8.83810648050698,-49.9175682080525));
#18925=CARTESIAN_POINT('Ctrl Pts',(22.2378058279894,-8.83129827231295,-49.9175682080462));
#18926=CARTESIAN_POINT('Ctrl Pts',(22.2374771383617,-8.83124617212726,-49.9175682080461));
#18927=CARTESIAN_POINT('Ctrl Pts',(22.2371484567731,-8.83119402657727,-49.9175682080461));
#18928=CARTESIAN_POINT('Ctrl Pts',(22.2368197832205,-8.83114183558492,-49.917568208046));
#18929=CARTESIAN_POINT('Ctrl Pts',(22.124266225982,-8.81326914154663,-49.9175682080295));
#18930=CARTESIAN_POINT('Ctrl Pts',(22.0129325594699,-8.79011900697469,-49.9175682080505));
#18931=CARTESIAN_POINT('Ctrl Pts',(21.9034992420944,-8.75874571241589,-49.917568208057));
#18932=CARTESIAN_POINT('Ctrl Pts',(21.8361694326296,-8.73944301744522,-49.917568208061));
#18933=CARTESIAN_POINT('Ctrl Pts',(21.7695591263239,-8.71702701269534,-49.9175682080606));
#18934=CARTESIAN_POINT('Ctrl Pts',(21.7038295264635,-8.69080155058071,-49.9175682080606));
#18935=CARTESIAN_POINT('',(44.4585265683622,-8.87385981233827,-49.9175682080604));
#18936=CARTESIAN_POINT('',(0.0835265683620477,-8.87385981233827,-49.9175682080606));
#18937=CARTESIAN_POINT('',(44.4585265683622,-14.4544045823054,-49.9175682080604));
#18938=CARTESIAN_POINT('',(44.4585265683622,16.4830954176946,-49.9175682080604));
#18939=CARTESIAN_POINT('',(-44.2914734316379,-14.4544045823054,-49.9175682080606));
#18940=CARTESIAN_POINT('',(0.0835265683620477,-14.4544045823054,-49.9175682080606));
#18941=CARTESIAN_POINT('',(-44.2914734316379,-8.87385981233827,-49.9175682080606));
#18942=CARTESIAN_POINT('',(-44.2914734316379,16.4830954176946,-49.9175682080606));
#18943=CARTESIAN_POINT('',(-22.6217205869088,-8.87385981233827,-49.9175682080606));
#18944=CARTESIAN_POINT('',(0.0835265683620477,-8.87385981233827,-49.9175682080606));
#18945=CARTESIAN_POINT('',(-21.5367763897373,-8.69080155057986,-49.9175682080606));
#18946=CARTESIAN_POINT('Ctrl Pts',(-21.5367763897373,-8.69080155057986,
-49.9175682080606));
#18947=CARTESIAN_POINT('Ctrl Pts',(-21.6469419836331,-8.73475654612936,
-49.9175682080606));
#18948=CARTESIAN_POINT('Ctrl Pts',(-21.7605113768685,-8.76821292000271,
-49.9175682080606));
#18949=CARTESIAN_POINT('Ctrl Pts',(-21.8753760693094,-8.79411643469424,
-49.9175682080606));
#18950=CARTESIAN_POINT('Ctrl Pts',(-21.9404607776001,-8.80879390138636,
-49.9175682080605));
#18951=CARTESIAN_POINT('Ctrl Pts',(-22.0059610421381,-8.8210476068981,-49.9175682080605));
#18952=CARTESIAN_POINT('Ctrl Pts',(-22.0714936521756,-8.83141832822413,
-49.9175682080604));
#18953=CARTESIAN_POINT('Ctrl Pts',(-22.0715976486236,-8.83143478595685,
-49.9175682080604));
#18954=CARTESIAN_POINT('Ctrl Pts',(-22.0717016456503,-8.83145123875071,
-49.9175682080604));
#18955=CARTESIAN_POINT('Ctrl Pts',(-22.0718056432557,-8.83146768660594,
-49.9175682080604));
#18956=CARTESIAN_POINT('Ctrl Pts',(-22.253099438842,-8.86014040550798,-49.91756820806));
#18957=CARTESIAN_POINT('Ctrl Pts',(-22.4364613235644,-8.87385980853305,
-49.9175682080606));
#18958=CARTESIAN_POINT('Ctrl Pts',(-22.6217205869088,-8.87385981233827,
-49.9175682080606));
#18959=CARTESIAN_POINT('Ctrl Pts',(-21.5367763897373,-8.69080155057986,
-49.9175682080606));
#18960=CARTESIAN_POINT('Ctrl Pts',(-20.6768191353961,-8.34768669239856,
-49.9175682080606));
#18961=CARTESIAN_POINT('Ctrl Pts',(-19.8120276459033,-8.01980178776443,
-49.9175682080606));
#18962=CARTESIAN_POINT('Ctrl Pts',(-18.9419176465726,-7.70866381791265,
-49.9175682080605));
#18963=CARTESIAN_POINT('Ctrl Pts',(-18.0718076472418,-7.39752584806087,
-49.9175682080604));
#18964=CARTESIAN_POINT('Ctrl Pts',(-17.1963790130006,-7.10313511035513,
-49.9175682080604));
#18965=CARTESIAN_POINT('Ctrl Pts',(-16.3151693873186,-6.82695644195446,
-49.9175682080605));
#18966=CARTESIAN_POINT('Ctrl Pts',(-16.3042756711398,-6.82354225770076,
-49.9175682080605));
#18967=CARTESIAN_POINT('Ctrl Pts',(-16.2933810694345,-6.8201308617252,-49.9175682080605));
#18968=CARTESIAN_POINT('Ctrl Pts',(-16.2824855811758,-6.81672225716408,
-49.9175682080605));
#18969=CARTESIAN_POINT('Ctrl Pts',(-15.5378838660857,-6.58377695521956,
-49.9175682080606));
#18970=CARTESIAN_POINT('Ctrl Pts',(-14.7891028645241,-6.3638606691259,-49.917568208062));
#18971=CARTESIAN_POINT('Ctrl Pts',(-14.0359286423201,-6.15798672782537,
-49.9175682080591));
#18972=CARTESIAN_POINT('Ctrl Pts',(-13.9037503637057,-6.1218568891102,-49.9175682080586));
#18973=CARTESIAN_POINT('Ctrl Pts',(-13.7714368304336,-6.08615941360799,
-49.9175682080578));
#18974=CARTESIAN_POINT('Ctrl Pts',(-13.6389869509882,-6.05089962282532,
-49.9175682080567));
#18975=CARTESIAN_POINT('Ctrl Pts',(-13.6273051545214,-6.04778978458984,
-49.9175682080566));
#18976=CARTESIAN_POINT('Ctrl Pts',(-13.6156219114651,-6.0446832728291,-49.9175682080565));
#18977=CARTESIAN_POINT('Ctrl Pts',(-13.6039372399092,-6.04158009539289,
-49.9175682080564));
#18978=CARTESIAN_POINT('Ctrl Pts',(-13.0752254251082,-5.90116651456622,
-49.9175682080514));
#18979=CARTESIAN_POINT('Ctrl Pts',(-12.5437410638479,-5.76761845979613,
-49.9175682080552));
#18980=CARTESIAN_POINT('Ctrl Pts',(-12.0106327436219,-5.6415312830481,-49.9175682080555));
#18981=CARTESIAN_POINT('Ctrl Pts',(-11.6460490610781,-5.55530241458691,
-49.9175682080557));
#18982=CARTESIAN_POINT('Ctrl Pts',(-11.2807047388469,-5.47256360694476,
-49.9175682080568));
#18983=CARTESIAN_POINT('Ctrl Pts',(-10.9149590454957,-5.39351662111492,
-49.9175682080423));
#18984=CARTESIAN_POINT('Ctrl Pts',(-10.9060718037445,-5.39159586118379,
-49.9175682080419));
#18985=CARTESIAN_POINT('Ctrl Pts',(-10.8971843893216,-5.38967730441873,
-49.9175682080416));
#18986=CARTESIAN_POINT('Ctrl Pts',(-10.8882968000924,-5.38776095106793,
-49.9175682080412));
#18987=CARTESIAN_POINT('Ctrl Pts',(-7.25039299962549,-4.60335148320457,
-49.9175682078867));
#18988=CARTESIAN_POINT('Ctrl Pts',(-3.57988304581191,-4.18752460344888,
-49.9175682079243));
#18989=CARTESIAN_POINT('Ctrl Pts',(0.127706037135239,-4.19081815795041,
-49.9175682080454));
#18990=CARTESIAN_POINT('Ctrl Pts',(0.134604712366228,-4.19082428623549,
-49.9175682080457));
#18991=CARTESIAN_POINT('Ctrl Pts',(0.14150351591446,-4.19083186535562,-49.9175682080459));
#18992=CARTESIAN_POINT('Ctrl Pts',(0.148402447809441,-4.19084089563809,
-49.9175682080461));
#18993=CARTESIAN_POINT('Ctrl Pts',(1.06843527170032,-4.19204516267696,-49.917568208075));
#18994=CARTESIAN_POINT('Ctrl Pts',(1.99072993137287,-4.2188222636332,-49.9175682080603));
#18995=CARTESIAN_POINT('Ctrl Pts',(2.91531018987283,-4.27143022964227,-49.9175682080605));
#18996=CARTESIAN_POINT('Ctrl Pts',(2.92625210297229,-4.27205281679694,-49.9175682080605));
#18997=CARTESIAN_POINT('Ctrl Pts',(2.93719445465181,-4.27267902824778,-49.9175682080605));
#18998=CARTESIAN_POINT('Ctrl Pts',(2.94813724502557,-4.27330886465573,-49.9175682080605));
#18999=CARTESIAN_POINT('Ctrl Pts',(3.86878242893392,-4.32629862648307,-49.9175682080607));
#19000=CARTESIAN_POINT('Ctrl Pts',(4.78362256361209,-4.40442769523306,-49.9175682080604));
#19001=CARTESIAN_POINT('Ctrl Pts',(5.69278120066898,-4.50641515619369,-49.9175682080605));
#19002=CARTESIAN_POINT('Ctrl Pts',(5.70666065356689,-4.50797212337509,-49.9175682080605));
#19003=CARTESIAN_POINT('Ctrl Pts',(5.72053877758951,-4.50953465011834,-49.9175682080605));
#19004=CARTESIAN_POINT('Ctrl Pts',(5.73441557288183,-4.51110273180188,-49.9175682080605));
#19005=CARTESIAN_POINT('Ctrl Pts',(6.81408656211051,-4.63310585044643,-49.9175682080606));
#19006=CARTESIAN_POINT('Ctrl Pts',(7.88583325609898,-4.78875206541689,-49.9175682080605));
#19007=CARTESIAN_POINT('Ctrl Pts',(8.95019649950668,-4.97573014441061,-49.9175682080605));
#19008=CARTESIAN_POINT('Ctrl Pts',(9.68564887908743,-5.10492802302684,-49.9175682080605));
#19009=CARTESIAN_POINT('Ctrl Pts',(10.4175763192467,-5.24908423889634,-49.9175682080604));
#19010=CARTESIAN_POINT('Ctrl Pts',(11.1461610317702,-5.40742232363211,-49.9175682080605));
#19011=CARTESIAN_POINT('Ctrl Pts',(11.1607824021305,-5.41059988107913,-49.9175682080605));
#19012=CARTESIAN_POINT('Ctrl Pts',(11.1754024252444,-5.41378314936595,-49.9175682080605));
#19013=CARTESIAN_POINT('Ctrl Pts',(11.1900211026185,-5.41697212217341,-49.9175682080605));
#19014=CARTESIAN_POINT('Ctrl Pts',(12.2995504913854,-5.65900900138633,-49.9175682080606));
#19015=CARTESIAN_POINT('Ctrl Pts',(13.4013634194074,-5.93379674455541,-49.9175682080606));
#19016=CARTESIAN_POINT('Ctrl Pts',(14.4960809935799,-6.23869144821723,-49.9175682080606));
#19017=CARTESIAN_POINT('Ctrl Pts',(15.6085307003123,-6.54852480768373,-49.9175682080606));
#19018=CARTESIAN_POINT('Ctrl Pts',(16.7136533733802,-6.88944821124417,-49.9175682080606));
#19019=CARTESIAN_POINT('Ctrl Pts',(17.8121149578433,-7.25863482928546,-49.9175682080606));
#19020=CARTESIAN_POINT('Ctrl Pts',(18.938442146212,-7.63718691646206,-49.9175682080606));
#19021=CARTESIAN_POINT('Ctrl Pts',(20.0577660356483,-8.04545424377254,-49.9175682080606));
#19022=CARTESIAN_POINT('Ctrl Pts',(21.1708187939427,-8.4803367087649,-49.9175682080606));
#19023=CARTESIAN_POINT('Ctrl Pts',(21.3486480781158,-8.54981664749443,-49.9175682080606));
#19024=CARTESIAN_POINT('Ctrl Pts',(21.526317316444,-8.61997584795984,-49.9175682080606));
#19025=CARTESIAN_POINT('Ctrl Pts',(21.7038295264614,-8.69080155057986,-49.9175682080606));
#19026=CARTESIAN_POINT('Origin',(-49.916473431638,16.4830954176946,0.0824317919394229));
#19027=CARTESIAN_POINT('',(-49.9164734316384,-8.87385981233827,44.4574317919389));
#19028=CARTESIAN_POINT('',(-49.9164734316384,-14.4544045823054,44.4574317919389));
#19029=CARTESIAN_POINT('',(-49.9164734316384,16.4830954176946,44.4574317919389));
#19030=CARTESIAN_POINT('',(-49.916473431638,-8.87385981233827,22.7876789472102));
#19031=CARTESIAN_POINT('',(-49.916473431638,-8.87385981233827,0.0824317919394229));
#19032=CARTESIAN_POINT('',(-49.916473431638,-8.69080155057986,21.7027347500388));
#19033=CARTESIAN_POINT('Ctrl Pts',(-49.916473431638,-8.69080155057985,21.7027347500388));
#19034=CARTESIAN_POINT('Ctrl Pts',(-49.916473431638,-8.73475654611729,21.8129003439043));
#19035=CARTESIAN_POINT('Ctrl Pts',(-49.916473431638,-8.76821291998423,21.9264697371077));
#19036=CARTESIAN_POINT('Ctrl Pts',(-49.916473431638,-8.79411643467275,22.0413344295164));
#19037=CARTESIAN_POINT('Ctrl Pts',(-49.9164734316379,-8.8087939013743,22.1064191378382));
#19038=CARTESIAN_POINT('Ctrl Pts',(-49.9164734316379,-8.82104760689287,
22.1719194024078));
#19039=CARTESIAN_POINT('Ctrl Pts',(-49.9164734316378,-8.83141832822398,
22.2374520124771));
#19040=CARTESIAN_POINT('Ctrl Pts',(-49.9164734316378,-8.8314347859567,22.2375560089251));
#19041=CARTESIAN_POINT('Ctrl Pts',(-49.9164734316378,-8.83145123875055,
22.2376600059518));
#19042=CARTESIAN_POINT('Ctrl Pts',(-49.9164734316378,-8.83146768660578,
22.2377640035571));
#19043=CARTESIAN_POINT('Ctrl Pts',(-49.9164734316374,-8.86014040550796,
22.4190577991434));
#19044=CARTESIAN_POINT('Ctrl Pts',(-49.916473431638,-8.87385980853305,22.6024196838659));
#19045=CARTESIAN_POINT('Ctrl Pts',(-49.916473431638,-8.87385981233827,22.7876789472102));
#19046=CARTESIAN_POINT('',(-49.916473431638,-8.69080155057987,-21.5378711661599));
#19047=CARTESIAN_POINT('Ctrl Pts',(-49.916473431638,-8.69080155057986,21.7027347500388));
#19048=CARTESIAN_POINT('Ctrl Pts',(-49.916473431638,-8.34822820653461,20.8441347059753));
#19049=CARTESIAN_POINT('Ctrl Pts',(-49.9164734316379,-8.02077061917538,
19.9805588353482));
#19050=CARTESIAN_POINT('Ctrl Pts',(-49.9164734316377,-7.70995711777993,
19.1115008037841));
#19051=CARTESIAN_POINT('Ctrl Pts',(-49.9164734316375,-7.4148561321092,18.2863761532518));
#19052=CARTESIAN_POINT('Ctrl Pts',(-49.9164734316374,-7.13475881039956,
17.4563096733183));
#19053=CARTESIAN_POINT('Ctrl Pts',(-49.9164734316377,-6.87092633632312,
16.6208886788675));
#19054=CARTESIAN_POINT('Ctrl Pts',(-49.9164734316377,-6.85687869806059,
16.5764070737578));
#19055=CARTESIAN_POINT('Ctrl Pts',(-49.9164734316378,-6.84287715903063,
16.5319102936858));
#19056=CARTESIAN_POINT('Ctrl Pts',(-49.9164734316378,-6.82892190575843,
16.4873982780546));
#19057=CARTESIAN_POINT('Ctrl Pts',(-49.9164734316378,-6.8242227389863,16.472409701299));
#19058=CARTESIAN_POINT('Ctrl Pts',(-49.9164734316378,-6.81952883192422,
16.4574193922089));
#19059=CARTESIAN_POINT('Ctrl Pts',(-49.9164734316378,-6.81484019286318,
16.4424273479626));
#19060=CARTESIAN_POINT('Ctrl Pts',(-49.9164734316381,-6.54248035969403,
15.571549761391));
#19061=CARTESIAN_POINT('Ctrl Pts',(-49.9164734316437,-6.28791975259315,
14.6948819543752));
#19062=CARTESIAN_POINT('Ctrl Pts',(-49.9164734316321,-6.05269948554821,
13.8117061511833));
#19063=CARTESIAN_POINT('Ctrl Pts',(-49.9164734316319,-6.04801972917164,
13.794135183985));
#19064=CARTESIAN_POINT('Ctrl Pts',(-49.9164734316317,-6.04334784544025,
13.7765622827464));
#19065=CARTESIAN_POINT('Ctrl Pts',(-49.9164734316314,-6.03868385436031,
13.758987494549));
#19066=CARTESIAN_POINT('Ctrl Pts',(-49.9164734316237,-5.8954927971015,13.2194168864696));
#19067=CARTESIAN_POINT('Ctrl Pts',(-49.9164734316301,-5.75970470970634,
12.6779353473642));
#19068=CARTESIAN_POINT('Ctrl Pts',(-49.9164734316267,-5.63181003590257,
12.135443265805));
#19069=CARTESIAN_POINT('Ctrl Pts',(-49.9164734316245,-5.55024150573681,
11.7894532382044));
#19070=CARTESIAN_POINT('Ctrl Pts',(-49.916473431624,-5.47188458180954,11.4430515684158));
#19071=CARTESIAN_POINT('Ctrl Pts',(-49.9164734315809,-5.39687731108541,
11.0964691595927));
#19072=CARTESIAN_POINT('Ctrl Pts',(-49.9164734315788,-5.39311846273983,
11.0791008338099));
#19073=CARTESIAN_POINT('Ctrl Pts',(-49.9164734315765,-5.38936791684796,
11.0617313708499));
#19074=CARTESIAN_POINT('Ctrl Pts',(-49.916473431574,-5.38562567685748,11.044360755025));
#19075=CARTESIAN_POINT('Ctrl Pts',(-49.9164734313206,-4.99630199552335,
9.23720992632475));
#19076=CARTESIAN_POINT('Ctrl Pts',(-49.9164734311946,-4.69745652901532,
7.41999756265195));
#19077=CARTESIAN_POINT('Ctrl Pts',(-49.9164734313608,-4.49601810718718,
5.59209844177902));
#19078=CARTESIAN_POINT('Ctrl Pts',(-49.9164734315186,-4.30470355970131,
3.85606571283916));
#19079=CARTESIAN_POINT('Ctrl Pts',(-49.9164734316221,-4.20125131727341,
2.11039336761343));
#19080=CARTESIAN_POINT('Ctrl Pts',(-49.9164734315923,-4.19154830182168,
0.35454703990375));
#19081=CARTESIAN_POINT('Ctrl Pts',(-49.9164734315908,-4.19103484317222,
0.261632163227361));
#19082=CARTESIAN_POINT('Ctrl Pts',(-49.9164734315888,-4.19078389395497,
0.168688797219065));
#19083=CARTESIAN_POINT('Ctrl Pts',(-49.9164734315863,-4.19079632233919,
0.0757168628223127));
#19084=CARTESIAN_POINT('Ctrl Pts',(-49.9164734315859,-4.19079846573759,
0.0596829285896319));
#19085=CARTESIAN_POINT('Ctrl Pts',(-49.9164734315854,-4.19080843354687,
0.0436473284827703));
#19086=CARTESIAN_POINT('Ctrl Pts',(-49.916473431585,-4.19082622399388,0.0276101156591523));
#19087=CARTESIAN_POINT('Ctrl Pts',(-49.9164734315646,-4.19162018413241,
-0.688105892081282));
#19088=CARTESIAN_POINT('Ctrl Pts',(-49.9164734316302,-4.20800554127586,
-1.40723120732015));
#19089=CARTESIAN_POINT('Ctrl Pts',(-49.9164734316362,-4.23981712342223,
-2.12474644065311));
#19090=CARTESIAN_POINT('Ctrl Pts',(-49.9164734316379,-4.24861125979728,
-2.32309956826786));
#19091=CARTESIAN_POINT('Ctrl Pts',(-49.9164734316379,-4.25858398530448,
-2.52132964566887));
#19092=CARTESIAN_POINT('Ctrl Pts',(-49.9164734316379,-4.26973111075349,
-2.71933074008867));
#19093=CARTESIAN_POINT('Ctrl Pts',(-49.9164734316379,-4.2706085974261,-2.73491711904427));
#19094=CARTESIAN_POINT('Ctrl Pts',(-49.9164734316379,-4.27149329106795,
-2.75050184046942));
#19095=CARTESIAN_POINT('Ctrl Pts',(-49.9164734316379,-4.27238518534672,
-2.76608490257921));
#19096=CARTESIAN_POINT('Ctrl Pts',(-49.9164734316378,-4.32475213351491,
-3.68103348474944));
#19097=CARTESIAN_POINT('Ctrl Pts',(-49.9164734316383,-4.40195367207473,
-4.59033598105189));
#19098=CARTESIAN_POINT('Ctrl Pts',(-49.9164734316376,-4.50277353999861,
-5.49426913991013));
#19099=CARTESIAN_POINT('Ctrl Pts',(-49.9164734316375,-4.50439146708877,
-5.5087751889213));
#19100=CARTESIAN_POINT('Ctrl Pts',(-49.9164734316375,-4.50601548028131,
-5.52327985438146));
#19101=CARTESIAN_POINT('Ctrl Pts',(-49.9164734316375,-4.50764557399692,
-5.53778313755417));
#19102=CARTESIAN_POINT('Ctrl Pts',(-49.9164734316361,-4.67191819991777,
-6.99935089187925));
#19103=CARTESIAN_POINT('Ctrl Pts',(-49.9164734316377,-4.89794158359744,
-8.4468800578816));
#19104=CARTESIAN_POINT('Ctrl Pts',(-49.9164734316379,-5.18003634705726,
-9.88166170717016));
#19105=CARTESIAN_POINT('Ctrl Pts',(-49.916473431638,-5.25026828473809,-10.2388732134829));
#19106=CARTESIAN_POINT('Ctrl Pts',(-49.916473431638,-5.32397599704584,-10.5952945281149));
#19107=CARTESIAN_POINT('Ctrl Pts',(-49.916473431638,-5.40107232558369,-10.9509454768652));
#19108=CARTESIAN_POINT('Ctrl Pts',(-49.916473431638,-5.4034198965424,-10.9617749917663));
#19109=CARTESIAN_POINT('Ctrl Pts',(-49.916473431638,-5.40577060663127,-10.9726037929874));
#19110=CARTESIAN_POINT('Ctrl Pts',(-49.916473431638,-5.40812445329306,-10.9834318811089));
#19111=CARTESIAN_POINT('Ctrl Pts',(-49.916473431638,-5.56766845157895,-11.7173609431609));
#19112=CARTESIAN_POINT('Ctrl Pts',(-49.916473431638,-5.74152740039569,-12.4475970185755));
#19113=CARTESIAN_POINT('Ctrl Pts',(-49.916473431638,-5.9289461269564,-13.1746186103254));
#19114=CARTESIAN_POINT('Ctrl Pts',(-49.916473431638,-6.12360434445706,-13.9297231280625));
#19115=CARTESIAN_POINT('Ctrl Pts',(-49.916473431638,-6.33289027977071,-14.681359999281));
#19116=CARTESIAN_POINT('Ctrl Pts',(-49.916473431638,-6.55601304252968,-15.4300534395904));
#19117=CARTESIAN_POINT('Ctrl Pts',(-49.916473431638,-6.64209054281505,-15.7188884245332));
#19118=CARTESIAN_POINT('Ctrl Pts',(-49.916473431638,-6.73022793651285,-16.0072852182616));
#19119=CARTESIAN_POINT('Ctrl Pts',(-49.916473431638,-6.82038180282843,-16.2952734904535));
#19120=CARTESIAN_POINT('Ctrl Pts',(-49.916473431638,-7.06758554760755,-17.0849432211904));
#19121=CARTESIAN_POINT('Ctrl Pts',(-49.916473431638,-7.33017880636613,-17.872095719996));
#19122=CARTESIAN_POINT('Ctrl Pts',(-49.916473431638,-7.60687660982169,-18.6562161182093));
#19123=CARTESIAN_POINT('Ctrl Pts',(-49.916473431638,-7.8961442096356,-19.4759574487281));
#19124=CARTESIAN_POINT('Ctrl Pts',(-49.916473431638,-8.20082770029567,-20.2923858276412));
#19125=CARTESIAN_POINT('Ctrl Pts',(-49.916473431638,-8.5195083391632,-21.1048868783802));
#19126=CARTESIAN_POINT('Ctrl Pts',(-49.916473431638,-8.57616615668215,-21.249340386539));
#19127=CARTESIAN_POINT('Ctrl Pts',(-49.916473431638,-8.63326651034672,-21.3936696719873));
#19128=CARTESIAN_POINT('Ctrl Pts',(-49.916473431638,-8.69080155057986,-21.5378711661599));
#19129=CARTESIAN_POINT('',(-49.916473431638,-8.87385981233827,-22.6228153633314));
#19130=CARTESIAN_POINT('Ctrl Pts',(-49.916473431638,-8.87385981233827,-22.6228153633314));
#19131=CARTESIAN_POINT('Ctrl Pts',(-49.916473431638,-8.87385981188611,-22.5528789322874));
#19132=CARTESIAN_POINT('Ctrl Pts',(-49.916473431638,-8.87185808464313,-22.4829109195166));
#19133=CARTESIAN_POINT('Ctrl Pts',(-49.9164734316379,-8.86782837150228,
-22.413116063267));
#19134=CARTESIAN_POINT('Ctrl Pts',(-49.9164734316378,-8.86373626040425,
-22.3422404709206));
#19135=CARTESIAN_POINT('Ctrl Pts',(-49.9164734316378,-8.85755327620405,
-22.2715417963385));
#19136=CARTESIAN_POINT('Ctrl Pts',(-49.9164734316348,-8.84920383564849,
-22.2012140842413));
#19137=CARTESIAN_POINT('Ctrl Pts',(-49.9164734316329,-8.84406583764695,
-22.1579364967426));
#19138=CARTESIAN_POINT('Ctrl Pts',(-49.9164734316298,-8.83810648050965,
-22.1147990884564));
#19139=CARTESIAN_POINT('Ctrl Pts',(-49.9164734316236,-8.83129827231297,
-22.0718474676879));
#19140=CARTESIAN_POINT('Ctrl Pts',(-49.9164734316235,-8.83124617212729,
-22.0715187780602));
#19141=CARTESIAN_POINT('Ctrl Pts',(-49.9164734316235,-8.83119402657729,
-22.0711900964716));
#19142=CARTESIAN_POINT('Ctrl Pts',(-49.9164734316234,-8.83114183558494,
-22.070861422919));
#19143=CARTESIAN_POINT('Ctrl Pts',(-49.9164734316069,-8.81326914156542,
-21.9583078657989));
#19144=CARTESIAN_POINT('Ctrl Pts',(-49.9164734316278,-8.79011900702328,
-21.8469741994026));
#19145=CARTESIAN_POINT('Ctrl Pts',(-49.9164734316343,-8.75874571251476,
-21.7375408821381));
#19146=CARTESIAN_POINT('Ctrl Pts',(-49.9164734316383,-8.73944301752175,
-21.6702110725558));
#19147=CARTESIAN_POINT('Ctrl Pts',(-49.916473431638,-8.71702701274011,-21.6036007661347));
#19148=CARTESIAN_POINT('Ctrl Pts',(-49.916473431638,-8.69080155058072,-21.5378711661621));
#19149=CARTESIAN_POINT('',(-49.916473431638,-8.87385981233827,-44.2925682080605));
#19150=CARTESIAN_POINT('',(-49.916473431638,-8.87385981233827,0.0824317919394229));
#19151=CARTESIAN_POINT('',(-49.916473431638,-14.4544045823054,-44.2925682080605));
#19152=CARTESIAN_POINT('',(-49.916473431638,16.4830954176946,-44.2925682080605));
#19153=CARTESIAN_POINT('',(-49.916473431638,-14.4544045823054,0.0824317919394229));
#19154=CARTESIAN_POINT('Origin',(-44.291473431638,16.4830954176946,-44.2925682080606));
#19155=CARTESIAN_POINT('Origin',(-44.291473431638,-8.87385981233827,-44.2925682080606));
#19156=CARTESIAN_POINT('Origin',(-44.291473431638,-14.4544045823054,-44.2925682080606));
#19157=CARTESIAN_POINT('Origin',(0.0835265683620477,16.4830954176946,-49.9175682080606));
#19158=CARTESIAN_POINT('',(44.4585265683622,16.1705954176946,-49.9175682080604));
#19159=CARTESIAN_POINT('',(44.4585265683622,13.4386401876617,-49.9175682080604));
#19160=CARTESIAN_POINT('',(44.4585265683622,16.4830954176946,-49.9175682080604));
#19161=CARTESIAN_POINT('',(11.0320394968432,13.4386401876617,-49.9175682080606));
#19162=CARTESIAN_POINT('',(0.0835265683620477,13.4386401876617,-49.9175682080606));
#19163=CARTESIAN_POINT('',(8.7491915745805,13.2555819259033,-49.9175682080606));
#19164=CARTESIAN_POINT('Ctrl Pts',(8.7491915745807,13.2555819259034,-49.9175682080606));
#19165=CARTESIAN_POINT('Ctrl Pts',(8.99003448998826,13.2969611280011,-49.9175682080606));
#19166=CARTESIAN_POINT('Ctrl Pts',(9.23206419125339,13.3294628821321,-49.9175682080606));
#19167=CARTESIAN_POINT('Ctrl Pts',(9.47484465594503,13.3553162053599,-49.9175682080606));
#19168=CARTESIAN_POINT('Ctrl Pts',(9.61194028432273,13.3699153107618,-49.9175682080606));
#19169=CARTESIAN_POINT('Ctrl Pts',(9.7492755379265,13.3823932020189,-49.9175682080606));
#19170=CARTESIAN_POINT('Ctrl Pts',(9.88677297754905,13.3931443825075,-49.9175682080606));
#19171=CARTESIAN_POINT('Ctrl Pts',(9.88683951929583,13.3931495855305,-49.9175682080606));
#19172=CARTESIAN_POINT('Ctrl Pts',(9.88690606106421,13.3931547881236,-49.9175682080606));
#19173=CARTESIAN_POINT('Ctrl Pts',(9.88697260285417,13.3931599902869,-49.9175682080606));
#19174=CARTESIAN_POINT('Ctrl Pts',(10.268028857282,13.4229505456848,-49.9175682080605));
#19175=CARTESIAN_POINT('Ctrl Pts',(10.6496949233627,13.4386401851025,-49.9175682080606));
#19176=CARTESIAN_POINT('Ctrl Pts',(11.0320394968432,13.4386401876617,-49.9175682080606));
#19177=CARTESIAN_POINT('',(-8.58213843785645,13.2555819259033,-49.9175682080606));
#19178=CARTESIAN_POINT('Ctrl Pts',(8.7491915745805,13.2555819259033,-49.9175682080606));
#19179=CARTESIAN_POINT('Ctrl Pts',(7.5422194222208,13.0482120850067,-49.9175682080606));
#19180=CARTESIAN_POINT('Ctrl Pts',(6.33247425101392,12.8826695784009,-49.9175682080606));
#19181=CARTESIAN_POINT('Ctrl Pts',(5.11985609192787,12.760436563551,-49.9175682080606));
#19182=CARTESIAN_POINT('Ctrl Pts',(3.91790295807075,12.6392785929576,-49.9175682080606));
#19183=CARTESIAN_POINT('Ctrl Pts',(2.7131271460502,12.5606716819903,-49.9175682080606));
#19184=CARTESIAN_POINT('Ctrl Pts',(1.50543703120817,12.5260083291905,-49.9175682080606));
#19185=CARTESIAN_POINT('Ctrl Pts',(1.03589406416592,12.5125314170909,-49.9175682080606));
#19186=CARTESIAN_POINT('Ctrl Pts',(0.565910630292547,12.5056965050877,-49.9175682080606));
#19187=CARTESIAN_POINT('Ctrl Pts',(0.0954815837620025,12.5055833090051,
-49.9175682080606));
#19188=CARTESIAN_POINT('Ctrl Pts',(0.0953271721160354,12.5055832718501,
-49.9175682080606));
#19189=CARTESIAN_POINT('Ctrl Pts',(0.0951727604441331,12.5055832354192,
-49.9175682080606));
#19190=CARTESIAN_POINT('Ctrl Pts',(0.0950183487462883,12.5055831997124,
-49.9175682080606));
#19191=CARTESIAN_POINT('Ctrl Pts',(-0.368415625222207,12.5054760332808,
-49.9175682080606));
#19192=CARTESIAN_POINT('Ctrl Pts',(-0.83251289115487,12.5119501585721,-49.9175682080609));
#19193=CARTESIAN_POINT('Ctrl Pts',(-1.29674624812002,12.5248910213237,-49.9175682080556));
#19194=CARTESIAN_POINT('Ctrl Pts',(-1.76348911659495,12.5379018386435,-49.9175682080503));
#19195=CARTESIAN_POINT('Ctrl Pts',(-2.23037087262208,12.5574495854659,-49.9175682080378));
#19196=CARTESIAN_POINT('Ctrl Pts',(-2.69685756803722,12.5834701483509,-49.9175682080287));
#19197=CARTESIAN_POINT('Ctrl Pts',(-3.15176140393925,12.6088446209459,-49.9175682080198));
#19198=CARTESIAN_POINT('Ctrl Pts',(-3.6062907130313,12.640374766738,-49.9175682080177));
#19199=CARTESIAN_POINT('Ctrl Pts',(-4.05993384799849,12.6780474220078,-49.9175682080302));
#19200=CARTESIAN_POINT('Ctrl Pts',(-4.12648203001281,12.6835738954108,-49.917568208032));
#19201=CARTESIAN_POINT('Ctrl Pts',(-4.19301109425748,12.689232634644,-49.9175682080341));
#19202=CARTESIAN_POINT('Ctrl Pts',(-4.25951937176003,12.6950236788102,-49.9175682080363));
#19203=CARTESIAN_POINT('Ctrl Pts',(-4.26518626359148,12.6955171094344,-49.9175682080365));
#19204=CARTESIAN_POINT('Ctrl Pts',(-4.27085296587595,12.6960114970058,-49.9175682080367));
#19205=CARTESIAN_POINT('Ctrl Pts',(-4.27651947671762,12.6965068414395,-49.9175682080369));
#19206=CARTESIAN_POINT('Ctrl Pts',(-5.12417205630176,12.7706053473349,-49.9175682080647));
#19207=CARTESIAN_POINT('Ctrl Pts',(-5.96958723650869,12.8659719414249,-49.9175682080601));
#19208=CARTESIAN_POINT('Ctrl Pts',(-6.81281170710773,12.9818931835264,-49.9175682080605));
#19209=CARTESIAN_POINT('Ctrl Pts',(-7.403656226973,13.0631188037732,-49.9175682080607));
#19210=CARTESIAN_POINT('Ctrl Pts',(-7.99342539485118,13.1544351597103,-49.9175682080606));
#19211=CARTESIAN_POINT('Ctrl Pts',(-8.58213843785645,13.2555819259033,-49.9175682080606));
#19212=CARTESIAN_POINT('',(-10.8649863601192,13.4386401876617,-49.9175682080606));
#19213=CARTESIAN_POINT('Ctrl Pts',(-10.8649863601192,13.4386401876617,-49.9175682080606));
#19214=CARTESIAN_POINT('Ctrl Pts',(-10.623898890525,13.4386401861139,-49.9175682080606));
#19215=CARTESIAN_POINT('Ctrl Pts',(-10.382962818652,13.4323889945158,-49.9175682080607));
#19216=CARTESIAN_POINT('Ctrl Pts',(-10.1423122637659,13.4203066131622,-49.9175682080605));
#19217=CARTESIAN_POINT('Ctrl Pts',(-10.0015635238242,13.4132400183986,-49.9175682080604));
#19218=CARTESIAN_POINT('Ctrl Pts',(-9.86091228790643,13.4041776979187,-49.9175682080602));
#19219=CARTESIAN_POINT('Ctrl Pts',(-9.72038472080964,13.3931955538157,-49.9175682080593));
#19220=CARTESIAN_POINT('Ctrl Pts',(-9.72013673011797,13.3931761734936,-49.9175682080593));
#19221=CARTESIAN_POINT('Ctrl Pts',(-9.71988874014172,13.3931567875853,-49.9175682080593));
#19222=CARTESIAN_POINT('Ctrl Pts',(-9.71964075088092,13.3931373960886,-49.9175682080593));
#19223=CARTESIAN_POINT('Ctrl Pts',(-9.33859499556313,13.363341559395,-49.917568208057));
#19224=CARTESIAN_POINT('Ctrl Pts',(-8.95909331010943,13.3203465159016,-49.9175682080606));
#19225=CARTESIAN_POINT('Ctrl Pts',(-8.58213843785645,13.2555819259033,-49.9175682080606));
#19226=CARTESIAN_POINT('',(-44.2914734316379,13.4386401876617,-49.9175682080606));
#19227=CARTESIAN_POINT('',(0.0835265683620477,13.4386401876617,-49.9175682080606));
#19228=CARTESIAN_POINT('',(-44.2914734316379,16.1705954176946,-49.9175682080606));
#19229=CARTESIAN_POINT('',(-44.2914734316379,16.4830954176946,-49.9175682080606));
#19230=CARTESIAN_POINT('',(44.4585265683622,16.1705954176946,-49.9175682080606));
#19231=CARTESIAN_POINT('Origin',(-49.916473431638,16.4830954176946,0.0824317919394229));
#19232=CARTESIAN_POINT('',(-49.916473431638,13.4386401876617,11.0309447204206));
#19233=CARTESIAN_POINT('',(-49.916473431638,13.2555819259033,8.74809679815787));
#19234=CARTESIAN_POINT('Ctrl Pts',(-49.916473431638,13.4386401876617,11.0309447204206));
#19235=CARTESIAN_POINT('Ctrl Pts',(-49.916473431638,13.4386401861139,10.7898572509304));
#19236=CARTESIAN_POINT('Ctrl Pts',(-49.916473431638,13.4323889945212,10.548921179161));
#19237=CARTESIAN_POINT('Ctrl Pts',(-49.9164734316379,13.4203066131778,10.3082706243783));
#19238=CARTESIAN_POINT('Ctrl Pts',(-49.9164734316378,13.413240018412,10.1675218843328));
#19239=CARTESIAN_POINT('Ctrl Pts',(-49.9164734316375,13.4041776979268,10.0268706483114));
#19240=CARTESIAN_POINT('Ctrl Pts',(-49.9164734316367,13.3931955538157,9.88634308111107));
#19241=CARTESIAN_POINT('Ctrl Pts',(-49.9164734316367,13.3931761734936,9.8860950904194));
#19242=CARTESIAN_POINT('Ctrl Pts',(-49.9164734316367,13.3931567875854,9.88584710044315));
#19243=CARTESIAN_POINT('Ctrl Pts',(-49.9164734316367,13.3931373960886,9.88559911118235));
#19244=CARTESIAN_POINT('Ctrl Pts',(-49.9164734316343,13.363341559395,9.50455335586456));
#19245=CARTESIAN_POINT('Ctrl Pts',(-49.9164734316379,13.3203465158881,9.12505167041318));
#19246=CARTESIAN_POINT('Ctrl Pts',(-49.9164734316379,13.2555819259033,8.74809679815787));
#19247=CARTESIAN_POINT('',(-49.9164734316384,13.4386401876617,44.4574317919389));
#19248=CARTESIAN_POINT('',(-49.916473431638,13.4386401876617,0.0824317919394229));
#19249=CARTESIAN_POINT('',(-49.9164734316384,16.1705954176946,44.4574317919389));
#19250=CARTESIAN_POINT('',(-49.9164734316384,16.4830954176946,44.4574317919389));
#19251=CARTESIAN_POINT('',(-49.916473431638,16.1705954176946,-44.2925682080605));
#19252=CARTESIAN_POINT('',(-49.916473431638,16.1705954176946,-44.2925682080605));
#19253=CARTESIAN_POINT('',(-49.916473431638,13.4386401876617,-44.2925682080605));
#19254=CARTESIAN_POINT('',(-49.916473431638,16.4830954176946,-44.2925682080605));
#19255=CARTESIAN_POINT('',(-49.916473431638,13.4386401876617,-10.8660811365418));
#19256=CARTESIAN_POINT('',(-49.916473431638,13.4386401876617,0.0824317919394229));
#19257=CARTESIAN_POINT('',(-49.916473431638,13.2555819259033,-8.58323321427904));
#19258=CARTESIAN_POINT('Ctrl Pts',(-49.916473431638,13.2555819259034,-8.58323321427923));
#19259=CARTESIAN_POINT('Ctrl Pts',(-49.916473431638,13.2969611279791,-8.82407612955931));
#19260=CARTESIAN_POINT('Ctrl Pts',(-49.916473431638,13.3294628820976,-9.06610583069568));
#19261=CARTESIAN_POINT('Ctrl Pts',(-49.916473431638,13.3553162053187,-9.308886295258));
#19262=CARTESIAN_POINT('Ctrl Pts',(-49.916473431638,13.3699153107383,-9.44598192376377));
#19263=CARTESIAN_POINT('Ctrl Pts',(-49.9164734316379,13.3823932020088,-9.58331717749613));
#19264=CARTESIAN_POINT('Ctrl Pts',(-49.9164734316379,13.3931443825075,-9.72081461724757));
#19265=CARTESIAN_POINT('Ctrl Pts',(-49.9164734316379,13.3931495855304,-9.72088115899436));
#19266=CARTESIAN_POINT('Ctrl Pts',(-49.9164734316379,13.3931547881236,-9.72094770076274));
#19267=CARTESIAN_POINT('Ctrl Pts',(-49.9164734316379,13.3931599902869,-9.7210142425527));
#19268=CARTESIAN_POINT('Ctrl Pts',(-49.9164734316379,13.4229505456848,-10.1020704969805));
#19269=CARTESIAN_POINT('Ctrl Pts',(-49.916473431638,13.4386401851025,-10.4837365630612));
#19270=CARTESIAN_POINT('Ctrl Pts',(-49.916473431638,13.4386401876617,-10.8660811365418));
#19271=CARTESIAN_POINT('Ctrl Pts',(-49.916473431638,13.2555819259033,-8.58323321427904));
#19272=CARTESIAN_POINT('Ctrl Pts',(-49.916473431638,12.96000054605,-6.86283601154779));
#19273=CARTESIAN_POINT('Ctrl Pts',(-49.9164734316353,12.7491268966531,-5.13488457809543));
#19274=CARTESIAN_POINT('Ctrl Pts',(-49.91647343163,12.627713447568,-3.39929723711238));
#19275=CARTESIAN_POINT('Ctrl Pts',(-49.9164734316266,12.5467548468234,-2.24200598433218));
#19276=CARTESIAN_POINT('Ctrl Pts',(-49.9164734316258,12.5055720509986,-1.08131859955897));
#19277=CARTESIAN_POINT('Ctrl Pts',(-49.9164734316312,12.5055798807548,0.0828009301210683));
#19278=CARTESIAN_POINT('Ctrl Pts',(-49.9164734316312,12.5055799036492,0.0862048405726741));
#19279=CARTESIAN_POINT('Ctrl Pts',(-49.9164734316312,12.5055802787149,0.0896088291256518));
#19280=CARTESIAN_POINT('Ctrl Pts',(-49.9164734316313,12.5055810060177,0.0930128957784022));
#19281=CARTESIAN_POINT('Ctrl Pts',(-49.9164734316359,12.5057958374954,1.09850968428123));
#19282=CARTESIAN_POINT('Ctrl Pts',(-49.9164734316369,12.5366929761477,2.10132408426752));
#19283=CARTESIAN_POINT('Ctrl Pts',(-49.9164734316374,12.5974162153564,3.1015486275048));
#19284=CARTESIAN_POINT('Ctrl Pts',(-49.916473431638,12.658429061564,4.10654353595992));
#19285=CARTESIAN_POINT('Ctrl Pts',(-49.9164734316379,12.7495531744451,5.10892382670438));
#19286=CARTESIAN_POINT('Ctrl Pts',(-49.916473431638,12.8698680207488,6.10879232242438));
#19287=CARTESIAN_POINT('Ctrl Pts',(-49.916473431638,12.9759630639947,6.99048809441394));
#19288=CARTESIAN_POINT('Ctrl Pts',(-49.916473431638,13.1047558095398,7.87023084868606));
#19289=CARTESIAN_POINT('Ctrl Pts',(-49.916473431638,13.2555819259033,8.74809679815787));
#19290=CARTESIAN_POINT('Origin',(-44.291473431638,-14.7669045823054,-44.2925682080606));
#19291=CARTESIAN_POINT('',(49.7710265683622,-14.7669045823054,-44.2925682080604));
#19292=CARTESIAN_POINT('',(49.7710265683619,-14.7669045823054,36.6697170232579));
#19293=CARTESIAN_POINT('',(49.7710265683622,-14.7669045823054,-44.2925682080603));
#19294=CARTESIAN_POINT('',(48.8335265683621,-14.7669045823054,36.6697170232579));
#19295=CARTESIAN_POINT('',(0.0835265683620477,-14.7669045823054,36.6697170232579));
#19296=CARTESIAN_POINT('',(48.8335265683621,-14.7669045823054,34.5598618267976));
#19297=CARTESIAN_POINT('',(48.8335265683621,-14.7669045823054,37.2170722197182));
#19298=CARTESIAN_POINT('',(18.353013239185,-14.7669045823054,24.508895879384));
#19299=CARTESIAN_POINT('',(48.8335265683621,-14.7669045823054,34.5598618267976));
#19300=CARTESIAN_POINT('',(18.7518431265311,-14.7669045823054,23.2994061884498));
#19301=CARTESIAN_POINT('',(32.6717093993989,-14.7669045823054,-18.9139165598666));
#19302=CARTESIAN_POINT('',(46.5214090713319,-14.7669045823054,32.4564357525968));
#19303=CARTESIAN_POINT('',(-58.2113397045057,-14.7669045823054,-2.07924545974433));
#19304=CARTESIAN_POINT('',(47.5194292675621,-14.7669045823054,32.2548881068839));
#19305=CARTESIAN_POINT('Ctrl Pts',(47.5194292675621,-14.7669045823054,32.2548881068839));
#19306=CARTESIAN_POINT('Ctrl Pts',(47.5162066872753,-14.7669045823054,32.2596395478179));
#19307=CARTESIAN_POINT('Ctrl Pts',(47.5129007460645,-14.7669045824339,32.2643216222363));
#19308=CARTESIAN_POINT('Ctrl Pts',(47.5095148041896,-14.7669045818319,32.2689345284333));
#19309=CARTESIAN_POINT('Ctrl Pts',(47.4966520226391,-14.7669045795448,32.2864583982804));
#19310=CARTESIAN_POINT('Ctrl Pts',(47.4826382204761,-14.766904560918,32.302996393618));
#19311=CARTESIAN_POINT('Ctrl Pts',(47.4676517348738,-14.7669044772679,32.3185353475));
#19312=CARTESIAN_POINT('Ctrl Pts',(47.4530508977656,-14.7669043957704,32.3336744361751));
#19313=CARTESIAN_POINT('Ctrl Pts',(47.4375274264405,-14.7669042476547,32.3478657656707));
#19314=CARTESIAN_POINT('Ctrl Pts',(47.4212585314406,-14.7669041441791,32.3611431655407));
#19315=CARTESIAN_POINT('Ctrl Pts',(47.4130166573114,-14.7669040917581,32.3678695386897));
#19316=CARTESIAN_POINT('Ctrl Pts',(47.40458270289,-14.7669040484303,32.3743583583499));
#19317=CARTESIAN_POINT('Ctrl Pts',(47.3959789550955,-14.7669040210232,32.3806110243808));
#19318=CARTESIAN_POINT('Ctrl Pts',(47.3927525496726,-14.7669040107455,32.3829557741424));
#19319=CARTESIAN_POINT('Ctrl Pts',(47.3895022670568,-14.7669040026344,32.3852673148));
#19320=CARTESIAN_POINT('Ctrl Pts',(47.3862292825356,-14.7669039967743,32.3875457201751));
#19321=CARTESIAN_POINT('Ctrl Pts',(47.3833654210796,-14.7669039916467,32.3895393248782));
#19322=CARTESIAN_POINT('Ctrl Pts',(47.3804841784773,-14.7669039882399,32.3915075603807));
#19323=CARTESIAN_POINT('Ctrl Pts',(47.3775863420797,-14.7669039865145,32.3934504761374));
#19324=CARTESIAN_POINT('Ctrl Pts',(47.357301487297,-14.7669039744365,32.4070508864343));
#19325=CARTESIAN_POINT('Ctrl Pts',(47.3362035365451,-14.7669040526285,32.4194106291601));
#19326=CARTESIAN_POINT('Ctrl Pts',(47.3145625513543,-14.7669041305354,32.430546667658));
#19327=CARTESIAN_POINT('Ctrl Pts',(47.2859543315849,-14.7669042335241,32.4452679122732));
#19328=CARTESIAN_POINT('Ctrl Pts',(47.2562626252597,-14.7669043748298,32.4579595038599));
#19329=CARTESIAN_POINT('Ctrl Pts',(47.2258539195548,-14.7669044578905,32.4687823727686));
#19330=CARTESIAN_POINT('Ctrl Pts',(47.2135323703003,-14.7669044915466,32.4731677785016));
#19331=CARTESIAN_POINT('Ctrl Pts',(47.2010930296491,-14.7669045170158,32.4772457401317));
#19332=CARTESIAN_POINT('Ctrl Pts',(47.188560256884,-14.7669045346655,32.4810246061808));
#19333=CARTESIAN_POINT('Ctrl Pts',(47.15181324702,-14.7669045864155,32.4921045188691));
#19334=CARTESIAN_POINT('Ctrl Pts',(47.1142633116265,-14.7669045820527,32.5006221872233));
#19335=CARTESIAN_POINT('Ctrl Pts',(47.0765238293988,-14.7669045822747,32.5068345296263));
#19336=CARTESIAN_POINT('Ctrl Pts',(47.0696355872449,-14.7669045823153,32.5079684116059));
#19337=CARTESIAN_POINT('Ctrl Pts',(47.0627410460591,-14.7669045823054,32.5090253551335));
#19338=CARTESIAN_POINT('Ctrl Pts',(47.0558439863807,-14.7669045823054,32.51000674472));
#19339=CARTESIAN_POINT('Ctrl Pts',(47.0558350832418,-14.7669045823054,32.5100080115567));
#19340=CARTESIAN_POINT('Ctrl Pts',(47.0558261800784,-14.7669045823054,32.5100092782722));
#19341=CARTESIAN_POINT('Ctrl Pts',(47.0558172768906,-14.7669045823054,32.5100105448667));
#19342=CARTESIAN_POINT('Ctrl Pts',(47.0334702770518,-14.7669045823054,32.5131896967335));
#19343=CARTESIAN_POINT('Ctrl Pts',(47.0109580530394,-14.7669045826373,32.5155957537189));
#19344=CARTESIAN_POINT('Ctrl Pts',(46.988364088111,-14.7669045772469,32.5172682730289));
#19345=CARTESIAN_POINT('Ctrl Pts',(46.9544731407184,-14.7669045691613,32.5197770519939));
#19346=CARTESIAN_POINT('Ctrl Pts',(46.9203982755575,-14.766904546284,32.5206353717701));
#19347=CARTESIAN_POINT('Ctrl Pts',(46.8864212383181,-14.7669045319054,32.5199766904459));
#19348=CARTESIAN_POINT('Ctrl Pts',(46.8524442010786,-14.7669045175269,32.5193180091216));
#19349=CARTESIAN_POINT('Ctrl Pts',(46.8185649917614,-14.7669045165844,32.5171423266874));
#19350=CARTESIAN_POINT('Ctrl Pts',(46.7850653560599,-14.7669045221653,32.5135831012478));
#19351=CARTESIAN_POINT('Ctrl Pts',(46.7521381651874,-14.7669045276508,32.510084696177));
#19352=CARTESIAN_POINT('Ctrl Pts',(46.7194212193199,-14.766904544103,32.505250427923));
#19353=CARTESIAN_POINT('Ctrl Pts',(46.6868943696421,-14.7669045570257,32.4991343892605));
#19354=CARTESIAN_POINT('Ctrl Pts',(46.6540025802383,-14.7669045700934,32.4929497308117));
#19355=CARTESIAN_POINT('Ctrl Pts',(46.6213042457889,-14.7669045784001,32.4854538238257));
#19356=CARTESIAN_POINT('Ctrl Pts',(46.5887987004027,-14.7669045808678,32.4766539405727));
#19357=CARTESIAN_POINT('Ctrl Pts',(46.566239175518,-14.7669045825804,32.4705466384841));
#19358=CARTESIAN_POINT('Ctrl Pts',(46.5437729059787,-14.7669045823054,32.4638102368474));
#19359=CARTESIAN_POINT('Ctrl Pts',(46.5214090713319,-14.7669045823054,32.4564357525968));
#19360=CARTESIAN_POINT('',(48.582477269951,-14.7669045823054,30.6288487842779));
#19361=CARTESIAN_POINT('Origin',(0.0835265683620477,-14.7669045823054,0.0824317919394229));
#19362=CARTESIAN_POINT('',(48.833526568362,-14.7669045823054,29.5557152835192));
#19363=CARTESIAN_POINT('Ctrl Pts',(48.833526568362,-14.7669045823054,29.5557152835192));
#19364=CARTESIAN_POINT('Ctrl Pts',(48.8335265671902,-14.7669045823054,29.6860166606407));
#19365=CARTESIAN_POINT('Ctrl Pts',(48.8252222740679,-14.7669045823192,29.8150666965999));
#19366=CARTESIAN_POINT('Ctrl Pts',(48.8072820544696,-14.7669045822898,29.9426399241485));
#19367=CARTESIAN_POINT('Ctrl Pts',(48.7995859656251,-14.7669045822772,29.9973669517645));
#19368=CARTESIAN_POINT('Ctrl Pts',(48.7901172263589,-14.7669045822536,30.0518222752217));
#19369=CARTESIAN_POINT('Ctrl Pts',(48.7787736637774,-14.7669045821918,30.1059884300764));
#19370=CARTESIAN_POINT('Ctrl Pts',(48.7786594332202,-14.7669045821911,30.1065338874674));
#19371=CARTESIAN_POINT('Ctrl Pts',(48.7785450210994,-14.7669045821905,30.1070793522221));
#19372=CARTESIAN_POINT('Ctrl Pts',(48.7784304268186,-14.7669045821899,30.1076248236673));
#19373=CARTESIAN_POINT('Ctrl Pts',(48.7628103615851,-14.7669045821038,30.1819766979346));
#19374=CARTESIAN_POINT('Ctrl Pts',(48.7438390541929,-14.7669045821474,30.2563336460274));
#19375=CARTESIAN_POINT('Ctrl Pts',(48.7199833467506,-14.7669045822053,30.3291843404247));
#19376=CARTESIAN_POINT('Ctrl Pts',(48.701498823388,-14.7669045822502,30.3856324824816));
#19377=CARTESIAN_POINT('Ctrl Pts',(48.6800822715329,-14.7669045822859,30.4411782859976));
#19378=CARTESIAN_POINT('Ctrl Pts',(48.6549907210206,-14.7669045822974,30.4951150676414));
#19379=CARTESIAN_POINT('Ctrl Pts',(48.6336414604553,-14.7669045823072,30.5410074251026));
#19380=CARTESIAN_POINT('Ctrl Pts',(48.609631649145,-14.7669045823054,30.5857353283516));
#19381=CARTESIAN_POINT('Ctrl Pts',(48.582477269951,-14.7669045823054,30.6288487842779));
#19382=CARTESIAN_POINT('',(48.8335265683622,-14.7669045823054,-29.39085169964));
#19383=CARTESIAN_POINT('',(48.8335265683622,-14.7669045823054,-30.3185344755987));
#19384=CARTESIAN_POINT('',(48.5824772699512,-14.7669045823054,-30.4639852003988));
#19385=CARTESIAN_POINT('Ctrl Pts',(48.5824772699512,-14.7669045823054,-30.4639852003988));
#19386=CARTESIAN_POINT('Ctrl Pts',(48.6324063391242,-14.7669045823054,-30.3847121561984));
#19387=CARTESIAN_POINT('Ctrl Pts',(48.6712567149129,-14.7669045823054,-30.2991109807002));
#19388=CARTESIAN_POINT('Ctrl Pts',(48.7346346019905,-14.7669045823054,-30.1242144446989));
#19389=CARTESIAN_POINT('Ctrl Pts',(48.7589711993479,-14.7669045823054,-30.0350331364586));
#19390=CARTESIAN_POINT('Ctrl Pts',(48.8162053854519,-14.7669045823054,-29.7637707034856));
#19391=CARTESIAN_POINT('Ctrl Pts',(48.8335265683622,-14.7669045823054,-29.5772266964482));
#19392=CARTESIAN_POINT('Ctrl Pts',(48.8335265683622,-14.7669045823054,-29.39085169964));
#19393=CARTESIAN_POINT('',(37.8461247099825,-14.7669045823054,-43.0362183703681));
#19394=CARTESIAN_POINT('Origin',(0.0835265683620477,-14.7669045823054,0.0824317919394229));
#19395=CARTESIAN_POINT('',(36.8109793750892,-14.7669045823054,-42.4433312829855));
#19396=CARTESIAN_POINT('Ctrl Pts',(37.8461247099825,-14.7669045823054,-43.0362183703681));
#19397=CARTESIAN_POINT('Ctrl Pts',(37.8298309202723,-14.7669045823054,-43.0504882009569));
#19398=CARTESIAN_POINT('Ctrl Pts',(37.812621196783,-14.7669045823054,-43.0635470401069));
#19399=CARTESIAN_POINT('Ctrl Pts',(37.7946352381859,-14.7669045823054,-43.0752957980133));
#19400=CARTESIAN_POINT('Ctrl Pts',(37.7769014109269,-14.7669045823054,-43.0868798591073));
#19401=CARTESIAN_POINT('Ctrl Pts',(37.7584118543307,-14.7669045823054,-43.0971912466976));
#19402=CARTESIAN_POINT('Ctrl Pts',(37.7392652539178,-14.7669045823054,-43.1061009232293));
#19403=CARTESIAN_POINT('Ctrl Pts',(37.7246902092306,-14.7669045823054,-43.1128832726176));
#19404=CARTESIAN_POINT('Ctrl Pts',(37.7097336127022,-14.7669045823054,-43.1188527973872));
#19405=CARTESIAN_POINT('Ctrl Pts',(37.6944306958395,-14.7669045823054,-43.123933952747));
#19406=CARTESIAN_POINT('Ctrl Pts',(37.6944288513635,-14.7669045823054,-43.1239345651839));
#19407=CARTESIAN_POINT('Ctrl Pts',(37.694427006883,-14.7669045823054,-43.1239351776075));
#19408=CARTESIAN_POINT('Ctrl Pts',(37.6944251623982,-14.7669045823054,-43.123935790018));
#19409=CARTESIAN_POINT('Ctrl Pts',(37.6386324644014,-14.7669045823054,-43.1424602224209));
#19410=CARTESIAN_POINT('Ctrl Pts',(37.5790647273354,-14.7669045823054,-43.1489383928368));
#19411=CARTESIAN_POINT('Ctrl Pts',(37.5205875226989,-14.7669045823054,-43.1443560209437));
#19412=CARTESIAN_POINT('Ctrl Pts',(37.5205836562294,-14.7669045823054,-43.1443557179606));
#19413=CARTESIAN_POINT('Ctrl Pts',(37.5205797897646,-14.7669045823054,-43.1443554149293));
#19414=CARTESIAN_POINT('Ctrl Pts',(37.5205759233047,-14.7669045823054,-43.1443551118495));
#19415=CARTESIAN_POINT('Ctrl Pts',(37.4036218025329,-14.7669045823054,-43.1351874428476));
#19416=CARTESIAN_POINT('Ctrl Pts',(37.2925576207558,-14.7669045823054,-43.0833778715053));
#19417=CARTESIAN_POINT('Ctrl Pts',(37.1988710917299,-14.7669045823054,-43.0132402586517));
#19418=CARTESIAN_POINT('Ctrl Pts',(37.1988648972462,-14.7669045823054,-43.0132356212048));
#19419=CARTESIAN_POINT('Ctrl Pts',(37.1988587028394,-14.7669045823054,-43.013230983672));
#19420=CARTESIAN_POINT('Ctrl Pts',(37.1988525085094,-14.7669045823054,-43.0132263460532));
#19421=CARTESIAN_POINT('Ctrl Pts',(37.1871477901788,-14.7669045823054,-43.0044631670982));
#19422=CARTESIAN_POINT('Ctrl Pts',(37.1756777312701,-14.7669045833006,-42.9954067949474));
#19423=CARTESIAN_POINT('Ctrl Pts',(37.1644411183454,-14.7669045783028,-42.9860779934194));
#19424=CARTESIAN_POINT('Ctrl Pts',(37.1375020351172,-14.7669045663207,-42.9637127698001));
#19425=CARTESIAN_POINT('Ctrl Pts',(37.1118996431171,-14.766904502036,-42.9397826144006));
#19426=CARTESIAN_POINT('Ctrl Pts',(37.0876273944267,-14.7669043153494,-42.9145720776327));
#19427=CARTESIAN_POINT('Ctrl Pts',(37.076446034899,-14.7669042293495,-42.902958482243));
#19428=CARTESIAN_POINT('Ctrl Pts',(37.0655462087051,-14.766904120834,-42.8910733513313));
#19429=CARTESIAN_POINT('Ctrl Pts',(37.0549236503131,-14.7669040086953,-42.8789450456804));
#19430=CARTESIAN_POINT('Ctrl Pts',(37.0380827633631,-14.7669038309118,-42.8597169636288));
#19431=CARTESIAN_POINT('Ctrl Pts',(37.0219431169162,-14.7669036396173,-42.8398770152339));
#19432=CARTESIAN_POINT('Ctrl Pts',(37.0064975538102,-14.7669035207875,-42.8195368438202));
#19433=CARTESIAN_POINT('Ctrl Pts',(36.9987747722572,-14.7669034613726,-42.8093667581133));
#19434=CARTESIAN_POINT('Ctrl Pts',(36.9912255115448,-14.7669034201738,-42.7990716166501));
#19435=CARTESIAN_POINT('Ctrl Pts',(36.9838488770277,-14.7669034045806,-42.7886653748589));
#19436=CARTESIAN_POINT('Ctrl Pts',(36.9764722425106,-14.7669033889875,-42.7782591330677));
#19437=CARTESIAN_POINT('Ctrl Pts',(36.9692682341903,-14.7669033991487,-42.7677417909482));
#19438=CARTESIAN_POINT('Ctrl Pts',(36.9622359573889,-14.7669034367692,-42.7571273039553));
#19439=CARTESIAN_POINT('Ctrl Pts',(36.9439833349958,-14.766903534415,-42.7295768777632));
#19440=CARTESIAN_POINT('Ctrl Pts',(36.9268780766106,-14.7669038199043,-42.7013696444846));
#19441=CARTESIAN_POINT('Ctrl Pts',(36.9108834785333,-14.7669040506412,-42.6725488010595));
#19442=CARTESIAN_POINT('Ctrl Pts',(36.8987074856777,-14.7669042262912,-42.6506087446767));
#19443=CARTESIAN_POINT('Ctrl Pts',(36.8871762981436,-14.7669043666507,-42.6283125394509));
#19444=CARTESIAN_POINT('Ctrl Pts',(36.8762936044956,-14.766904445574,-42.6056762745794));
#19445=CARTESIAN_POINT('Ctrl Pts',(36.8605909997264,-14.7669045594521,-42.5730144784999));
#19446=CARTESIAN_POINT('Ctrl Pts',(36.8462324067551,-14.7669045735796,-42.5396467674435));
#19447=CARTESIAN_POINT('Ctrl Pts',(36.8331795428374,-14.7669045795915,-42.5056252356918));
#19448=CARTESIAN_POINT('Ctrl Pts',(36.8253027509148,-14.7669045832193,-42.4850948349931));
#19449=CARTESIAN_POINT('Ctrl Pts',(36.8179024354812,-14.7669045823054,-42.4643261242436));
#19450=CARTESIAN_POINT('Ctrl Pts',(36.8109793750892,-14.7669045823054,-42.4433312829855));
#19451=CARTESIAN_POINT('',(20.56141397709,-14.7669045823054,6.83502636924522));
#19452=CARTESIAN_POINT('',(20.56141397709,-14.7669045823054,6.83502636924521));
#19453=CARTESIAN_POINT('',(9.92432302202933,-14.7669045823054,19.2683675629017));
#19454=CARTESIAN_POINT('Origin',(0.0835265683620477,-14.7669045823054,0.0824317919394229));
#19455=CARTESIAN_POINT('Origin',(10.2095634989472,-14.7669045823054,19.8244816432194));
#19456=CARTESIAN_POINT('',(14.5949188243533,-14.7669045823054,25.9268725828089));
#19457=CARTESIAN_POINT('',(29.703899630018,-14.7669045823054,-19.8925534551282));
#19458=CARTESIAN_POINT('',(46.9585265683621,-14.7669045823054,36.5987899438301));
#19459=CARTESIAN_POINT('',(-59.4004542373026,-14.7669045823054,1.52685782987659));
#19460=CARTESIAN_POINT('',(46.9585265683621,-14.7669045823054,38.3884670232579));
#19461=CARTESIAN_POINT('',(46.9585265683619,-14.7669045823054,0.0824317919392602));
#19462=CARTESIAN_POINT('',(48.8335265683621,-14.7669045823054,38.3884670232579));
#19463=CARTESIAN_POINT('',(0.0835265683620477,-14.7669045823054,38.3884670232579));
#19464=CARTESIAN_POINT('',(48.8335265683621,-14.7669045823054,37.6072170232579));
#19465=CARTESIAN_POINT('',(48.8335265683619,-14.7669045823054,0.0824317919392537));
#19466=CARTESIAN_POINT('',(0.0835265683620477,-14.7669045823054,37.6072170232579));
#19467=CARTESIAN_POINT('',(44.458526568362,-14.7669045823054,49.7699317919394));
#19468=CARTESIAN_POINT('Origin',(44.4585265683621,-14.7669045823054,44.4574317919394));
#19469=CARTESIAN_POINT('',(-44.2914734316384,-14.7669045823054,49.7699317919394));
#19470=CARTESIAN_POINT('',(-44.2914734316379,-14.7669045823054,49.7699317919394));
#19471=CARTESIAN_POINT('',(-49.603973431638,-14.7669045823054,44.4574317919389));
#19472=CARTESIAN_POINT('Origin',(-44.2914734316384,-14.7669045823054,44.457431791939));
#19473=CARTESIAN_POINT('',(-49.603973431638,-14.7669045823054,-44.2925682080605));
#19474=CARTESIAN_POINT('',(-49.603973431638,-14.7669045823054,-44.2925682080606));
#19475=CARTESIAN_POINT('',(-44.2914734316379,-14.7669045823054,-49.6050682080606));
#19476=CARTESIAN_POINT('Origin',(-44.291473431638,-14.7669045823054,-44.2925682080606));
#19477=CARTESIAN_POINT('',(44.4585265683622,-14.7669045823054,-49.6050682080606));
#19478=CARTESIAN_POINT('',(-44.291473431638,-14.7669045823054,-49.6050682080606));
#19479=CARTESIAN_POINT('Origin',(44.4585265683622,-14.7669045823054,-44.2925682080604));
#19480=CARTESIAN_POINT('',(30.6299435607004,-14.7669045823054,48.5813824935285));
#19481=CARTESIAN_POINT('',(43.2021767306697,-14.7669045823054,37.8450299335598));
#19482=CARTESIAN_POINT('Origin',(0.0835265683620477,-14.7669045823054,0.0824317919394229));
#19483=CARTESIAN_POINT('',(42.6092896432871,-14.7669045823054,36.8098845986664));
#19484=CARTESIAN_POINT('Ctrl Pts',(43.2021767306697,-14.7669045823054,37.8450299335598));
#19485=CARTESIAN_POINT('Ctrl Pts',(43.2164465612568,-14.7669045823054,37.8287361438515));
#19486=CARTESIAN_POINT('Ctrl Pts',(43.2295054004053,-14.7669045823054,37.8115264203645));
#19487=CARTESIAN_POINT('Ctrl Pts',(43.2412541583107,-14.7669045823054,37.7935404617698));
#19488=CARTESIAN_POINT('Ctrl Pts',(43.2528382194038,-14.7669045823054,37.7758066345126));
#19489=CARTESIAN_POINT('Ctrl Pts',(43.2631496069936,-14.7669045823054,37.7573170779186));
#19490=CARTESIAN_POINT('Ctrl Pts',(43.2720592835251,-14.7669045823054,37.7381704775078));
#19491=CARTESIAN_POINT('Ctrl Pts',(43.2788416329158,-14.7669045823054,37.7235954328166));
#19492=CARTESIAN_POINT('Ctrl Pts',(43.2848111576874,-14.7669045823054,37.708638836284));
#19493=CARTESIAN_POINT('Ctrl Pts',(43.2898923130487,-14.7669045823054,37.6933359194168));
#19494=CARTESIAN_POINT('Ctrl Pts',(43.2898929254855,-14.7669045823054,37.6933340749407));
#19495=CARTESIAN_POINT('Ctrl Pts',(43.2898935379092,-14.7669045823054,37.6933322304602));
#19496=CARTESIAN_POINT('Ctrl Pts',(43.2898941503197,-14.7669045823054,37.6933303859754));
#19497=CARTESIAN_POINT('Ctrl Pts',(43.3084185827225,-14.7669045823054,37.6375376879786));
#19498=CARTESIAN_POINT('Ctrl Pts',(43.3148967531382,-14.7669045823054,37.5779699509127));
#19499=CARTESIAN_POINT('Ctrl Pts',(43.3103143812451,-14.7669045823054,37.5194927462761));
#19500=CARTESIAN_POINT('Ctrl Pts',(43.3103140782621,-14.7669045823054,37.5194888798066));
#19501=CARTESIAN_POINT('Ctrl Pts',(43.3103137752307,-14.7669045823054,37.5194850133419));
#19502=CARTESIAN_POINT('Ctrl Pts',(43.310313472151,-14.7669045823054,37.5194811468819));
#19503=CARTESIAN_POINT('Ctrl Pts',(43.3011458031491,-14.7669045823054,37.4025270261101));
#19504=CARTESIAN_POINT('Ctrl Pts',(43.2493362318067,-14.7669045823054,37.2914628443332));
#19505=CARTESIAN_POINT('Ctrl Pts',(43.1791986189533,-14.7669045823054,37.1977763153071));
#19506=CARTESIAN_POINT('Ctrl Pts',(43.1791939815064,-14.7669045823054,37.1977701208234));
#19507=CARTESIAN_POINT('Ctrl Pts',(43.1791893439736,-14.7669045823054,37.1977639264166));
#19508=CARTESIAN_POINT('Ctrl Pts',(43.1791847063548,-14.7669045823054,37.1977577320866));
#19509=CARTESIAN_POINT('Ctrl Pts',(43.1704215273998,-14.7669045823054,37.186053013756));
#19510=CARTESIAN_POINT('Ctrl Pts',(43.1613651552491,-14.7669045833006,37.1745829548473));
#19511=CARTESIAN_POINT('Ctrl Pts',(43.152036353721,-14.7669045783028,37.1633463419226));
#19512=CARTESIAN_POINT('Ctrl Pts',(43.129671130102,-14.7669045663207,37.1364072586948));
#19513=CARTESIAN_POINT('Ctrl Pts',(43.1057409747029,-14.766904502036,37.110804866695));
#19514=CARTESIAN_POINT('Ctrl Pts',(43.0805304379353,-14.7669043153494,37.0865326180049));
#19515=CARTESIAN_POINT('Ctrl Pts',(43.0689168425453,-14.7669042293495,37.0753512584769));
#19516=CARTESIAN_POINT('Ctrl Pts',(43.0570317116333,-14.766904120834,37.0644514322827));
#19517=CARTESIAN_POINT('Ctrl Pts',(43.0449034059821,-14.7669040086953,37.0538288738903));
#19518=CARTESIAN_POINT('Ctrl Pts',(43.0256753239304,-14.7669038309118,37.0369879869403));
#19519=CARTESIAN_POINT('Ctrl Pts',(43.0058353755356,-14.7669036396173,37.0208483404934));
#19520=CARTESIAN_POINT('Ctrl Pts',(42.9854952041218,-14.7669035207875,37.0054027773874));
#19521=CARTESIAN_POINT('Ctrl Pts',(42.975325118415,-14.7669034613726,36.9976799958344));
#19522=CARTESIAN_POINT('Ctrl Pts',(42.9650299769516,-14.7669034201738,36.990130735122));
#19523=CARTESIAN_POINT('Ctrl Pts',(42.9546237351605,-14.7669034045806,36.982754100605));
#19524=CARTESIAN_POINT('Ctrl Pts',(42.9442174933693,-14.7669033889875,36.9753774660879));
#19525=CARTESIAN_POINT('Ctrl Pts',(42.9337001512499,-14.7669033991487,36.9681734577675));
#19526=CARTESIAN_POINT('Ctrl Pts',(42.9230856642569,-14.7669034367692,36.9611411809661));
#19527=CARTESIAN_POINT('Ctrl Pts',(42.8955352380647,-14.766903534415,36.9428885585729));
#19528=CARTESIAN_POINT('Ctrl Pts',(42.8673280047859,-14.7669038199043,36.9257833001877));
#19529=CARTESIAN_POINT('Ctrl Pts',(42.8385071613608,-14.7669040506412,36.9097887021103));
#19530=CARTESIAN_POINT('Ctrl Pts',(42.8165671049781,-14.7669042262912,36.8976127092548));
#19531=CARTESIAN_POINT('Ctrl Pts',(42.7942708997524,-14.7669043666507,36.8860815217207));
#19532=CARTESIAN_POINT('Ctrl Pts',(42.771634634881,-14.766904445574,36.8751988280728));
#19533=CARTESIAN_POINT('Ctrl Pts',(42.7389728388023,-14.7669045594521,36.859496223304));
#19534=CARTESIAN_POINT('Ctrl Pts',(42.7056051277468,-14.7669045735796,36.845137630333));
#19535=CARTESIAN_POINT('Ctrl Pts',(42.6715835959959,-14.7669045795915,36.8320847664156));
#19536=CARTESIAN_POINT('Ctrl Pts',(42.6510531952964,-14.7669045832193,36.8242079744926));
#19537=CARTESIAN_POINT('Ctrl Pts',(42.6302844845461,-14.7669045823054,36.8168076590587));
#19538=CARTESIAN_POINT('Ctrl Pts',(42.6092896432871,-14.7669045823054,36.8098845986664));
#19539=CARTESIAN_POINT('',(-6.66906800894368,-14.7669045823054,20.5603192006674));
#19540=CARTESIAN_POINT('',(-6.66906800894368,-14.7669045823054,20.5603192006674));
#19541=CARTESIAN_POINT('',(-19.1024092026003,-14.7669045823054,9.9232282456065));
#19542=CARTESIAN_POINT('Origin',(0.0835265683620477,-14.7669045823054,0.0824317919394229));
#19543=CARTESIAN_POINT('',(-20.2520852367942,-14.7669045823054,10.012741343472));
#19544=CARTESIAN_POINT('Origin',(-19.6585232829181,-14.7669045823054,10.2084687225244));
#19545=CARTESIAN_POINT('',(-32.2904773922958,-14.7669045823054,46.520314294909));
#19546=CARTESIAN_POINT('',(-6.45864799006472,-14.7669045823054,-31.8171733188375));
#19547=CARTESIAN_POINT('',(-32.0889297465829,-14.7669045823054,47.5183344911391));
#19548=CARTESIAN_POINT('Ctrl Pts',(-32.0889297465829,-14.7669045823054,
47.5183344911391));
#19549=CARTESIAN_POINT('Ctrl Pts',(-32.093681187517,-14.7669045823054,47.5151119108524));
#19550=CARTESIAN_POINT('Ctrl Pts',(-32.0983632619353,-14.7669045824339,
47.5118059696416));
#19551=CARTESIAN_POINT('Ctrl Pts',(-32.1029761681324,-14.7669045818319,
47.5084200277666));
#19552=CARTESIAN_POINT('Ctrl Pts',(-32.1205000379794,-14.7669045795448,
47.4955572462162));
#19553=CARTESIAN_POINT('Ctrl Pts',(-32.137038033317,-14.7669045609181,47.4815434440533));
#19554=CARTESIAN_POINT('Ctrl Pts',(-32.1525769871989,-14.7669044772679,
47.466556958451));
#19555=CARTESIAN_POINT('Ctrl Pts',(-32.1677160758741,-14.7669043957704,
47.4519561213427));
#19556=CARTESIAN_POINT('Ctrl Pts',(-32.1819074053697,-14.7669042476547,
47.4364326500176));
#19557=CARTESIAN_POINT('Ctrl Pts',(-32.1951848052397,-14.7669041441791,
47.4201637550177));
#19558=CARTESIAN_POINT('Ctrl Pts',(-32.2019111783887,-14.7669040917581,
47.4119218808885));
#19559=CARTESIAN_POINT('Ctrl Pts',(-32.208399998049,-14.7669040484303,47.4034879264671));
#19560=CARTESIAN_POINT('Ctrl Pts',(-32.2146526640799,-14.7669040210232,
47.3948841786726));
#19561=CARTESIAN_POINT('Ctrl Pts',(-32.2169974138415,-14.7669040107455,
47.3916577732497));
#19562=CARTESIAN_POINT('Ctrl Pts',(-32.2193089544991,-14.7669040026344,
47.3884074906338));
#19563=CARTESIAN_POINT('Ctrl Pts',(-32.2215873598741,-14.7669039967743,
47.3851345061127));
#19564=CARTESIAN_POINT('Ctrl Pts',(-32.2235809645773,-14.7669039916468,
47.3822706446566));
#19565=CARTESIAN_POINT('Ctrl Pts',(-32.2255492000797,-14.7669039882399,
47.3793894020543));
#19566=CARTESIAN_POINT('Ctrl Pts',(-32.2274921158364,-14.7669039865145,
47.3764915656568));
#19567=CARTESIAN_POINT('Ctrl Pts',(-32.2410925261333,-14.7669039744365,
47.3562067108741));
#19568=CARTESIAN_POINT('Ctrl Pts',(-32.2534522688591,-14.7669040526285,
47.3351087601222));
#19569=CARTESIAN_POINT('Ctrl Pts',(-32.264588307357,-14.7669041305354,47.3134677749313));
#19570=CARTESIAN_POINT('Ctrl Pts',(-32.2793095519727,-14.7669042335241,
47.2848595551612));
#19571=CARTESIAN_POINT('Ctrl Pts',(-32.2920011435596,-14.7669043748298,
47.2551678488351));
#19572=CARTESIAN_POINT('Ctrl Pts',(-32.3028240124684,-14.7669044578905,
47.2247591431293));
#19573=CARTESIAN_POINT('Ctrl Pts',(-32.3072094182012,-14.7669044915466,
47.2124375938757));
#19574=CARTESIAN_POINT('Ctrl Pts',(-32.311287379831,-14.7669045170158,47.1999982532253));
#19575=CARTESIAN_POINT('Ctrl Pts',(-32.3150662458798,-14.7669045346655,
47.187465480461));
#19576=CARTESIAN_POINT('Ctrl Pts',(-32.3261461585685,-14.7669045864155,
47.1507184705958));
#19577=CARTESIAN_POINT('Ctrl Pts',(-32.3346638269229,-14.7669045820527,
47.1131685352009));
#19578=CARTESIAN_POINT('Ctrl Pts',(-32.340876169326,-14.7669045822747,47.0754290529718));
#19579=CARTESIAN_POINT('Ctrl Pts',(-32.3420100513053,-14.7669045823153,
47.0685408108192));
#19580=CARTESIAN_POINT('Ctrl Pts',(-32.3430669948327,-14.7669045823054,
47.0616462696348));
#19581=CARTESIAN_POINT('Ctrl Pts',(-32.3440483844191,-14.7669045823054,
47.0547492099578));
#19582=CARTESIAN_POINT('Ctrl Pts',(-32.3440496512557,-14.7669045823054,
47.0547403068188));
#19583=CARTESIAN_POINT('Ctrl Pts',(-32.3440509179712,-14.7669045823054,
47.0547314036554));
#19584=CARTESIAN_POINT('Ctrl Pts',(-32.3440521845657,-14.7669045823054,
47.0547225004677));
#19585=CARTESIAN_POINT('Ctrl Pts',(-32.3472313364325,-14.7669045823054,
47.0323755006289));
#19586=CARTESIAN_POINT('Ctrl Pts',(-32.3496373934179,-14.7669045826373,
47.0098632766164));
#19587=CARTESIAN_POINT('Ctrl Pts',(-32.3513099127279,-14.7669045772469,
46.987269311688));
#19588=CARTESIAN_POINT('Ctrl Pts',(-32.353818691693,-14.7669045691613,46.9533783642954));
#19589=CARTESIAN_POINT('Ctrl Pts',(-32.3546770114691,-14.766904546284,46.9193034991345));
#19590=CARTESIAN_POINT('Ctrl Pts',(-32.3540183301449,-14.7669045319054,
46.8853264618951));
#19591=CARTESIAN_POINT('Ctrl Pts',(-32.3533596488207,-14.7669045175269,
46.8513494246557));
#19592=CARTESIAN_POINT('Ctrl Pts',(-32.3511839663865,-14.7669045165844,
46.8174702153385));
#19593=CARTESIAN_POINT('Ctrl Pts',(-32.3476247409469,-14.7669045221653,
46.783970579637));
#19594=CARTESIAN_POINT('Ctrl Pts',(-32.3441263358758,-14.7669045276508,
46.7510433887625));
#19595=CARTESIAN_POINT('Ctrl Pts',(-32.3392920676214,-14.766904544103,46.718326442893));
#19596=CARTESIAN_POINT('Ctrl Pts',(-32.3331760289583,-14.7669045570257,
46.6857995932133));
#19597=CARTESIAN_POINT('Ctrl Pts',(-32.3269913705088,-14.7669045700934,
46.6529078038072));
#19598=CARTESIAN_POINT('Ctrl Pts',(-32.319495463522,-14.7669045784001,46.6202094693554));
#19599=CARTESIAN_POINT('Ctrl Pts',(-32.310695580268,-14.7669045808678,46.5877039239669));
#19600=CARTESIAN_POINT('Ctrl Pts',(-32.3045882781803,-14.7669045825804,
46.5651443990865));
#19601=CARTESIAN_POINT('Ctrl Pts',(-32.2978518765448,-14.7669045823054,
46.5426781295515));
#19602=CARTESIAN_POINT('Ctrl Pts',(-32.2904773922958,-14.7669045823054,
46.520314294909));
#19603=CARTESIAN_POINT('',(-30.4628904239763,-14.7669045823054,48.5813824935285));
#19604=CARTESIAN_POINT('Origin',(0.0835265683620477,-14.7669045823054,0.0824317919394229));
#19605=CARTESIAN_POINT('',(-29.3897569232175,-14.7669045823054,48.8324317919394));
#19606=CARTESIAN_POINT('Ctrl Pts',(-29.3897569232175,-14.7669045823054,
48.8324317919394));
#19607=CARTESIAN_POINT('Ctrl Pts',(-29.5200807466481,-14.7669045823054,
48.8324317908));
#19608=CARTESIAN_POINT('Ctrl Pts',(-29.6491709400179,-14.7669045823184,
48.8241256340683));
#19609=CARTESIAN_POINT('Ctrl Pts',(-29.7768043956785,-14.7669045822907,
48.8061704983924));
#19610=CARTESIAN_POINT('Ctrl Pts',(-29.8315190134296,-14.7669045822788,
48.7984733912343));
#19611=CARTESIAN_POINT('Ctrl Pts',(-29.8859659940187,-14.7669045822566,
48.7890037111312));
#19612=CARTESIAN_POINT('Ctrl Pts',(-29.9401280908703,-14.7669045821984,
48.7776586172617));
#19613=CARTESIAN_POINT('Ctrl Pts',(-29.9406641464146,-14.7669045821978,
48.7775463320877));
#19614=CARTESIAN_POINT('Ctrl Pts',(-29.9412002084696,-14.7669045821972,
48.7774338713268));
#19615=CARTESIAN_POINT('Ctrl Pts',(-29.9417362763945,-14.7669045821967,
48.7773212344192));
#19616=CARTESIAN_POINT('Ctrl Pts',(-30.0123701479919,-14.7669045821198,
48.7624798673106));
#19617=CARTESIAN_POINT('Ctrl Pts',(-30.0829795903623,-14.7669045821514,
48.7446144797856));
#19618=CARTESIAN_POINT('Ctrl Pts',(-30.1522892880597,-14.766904582203,48.7224220884003));
#19619=CARTESIAN_POINT('Ctrl Pts',(-30.2064608535874,-14.7669045822433,
48.7050768016066));
#19620=CARTESIAN_POINT('Ctrl Pts',(-30.2598402837736,-14.7669045822799,
48.6850886651948));
#19621=CARTESIAN_POINT('Ctrl Pts',(-30.3118149289063,-14.7669045822938,
48.6618061992418));
#19622=CARTESIAN_POINT('Ctrl Pts',(-30.360916740954,-14.7669045823069,48.639810642287));
#19623=CARTESIAN_POINT('Ctrl Pts',(-30.408765698194,-14.7669045823054,48.6148755124272));
#19624=CARTESIAN_POINT('Ctrl Pts',(-30.4548245533698,-14.7669045823054,
48.5864144376838));
#19625=CARTESIAN_POINT('Ctrl Pts',(-30.4575193501094,-14.7669045823054,
48.5847492462428));
#19626=CARTESIAN_POINT('Ctrl Pts',(-30.4602080106262,-14.7669045823054,
48.5830719723037));
#19627=CARTESIAN_POINT('Ctrl Pts',(-30.4628904239763,-14.7669045823054,
48.5813824935285));
#19628=CARTESIAN_POINT('',(29.5568100599416,-14.7669045823054,48.8324317919394));
#19629=CARTESIAN_POINT('',(30.4844928359003,-14.7669045823054,48.8324317919394));
#19630=CARTESIAN_POINT('Ctrl Pts',(30.6299435607004,-14.7669045823054,48.5813824935285));
#19631=CARTESIAN_POINT('Ctrl Pts',(30.5506705165001,-14.7669045823054,48.6313115627014));
#19632=CARTESIAN_POINT('Ctrl Pts',(30.4650693410018,-14.7669045823054,48.6701619384902));
#19633=CARTESIAN_POINT('Ctrl Pts',(30.2901728050006,-14.7669045823054,48.7335398255678));
#19634=CARTESIAN_POINT('Ctrl Pts',(30.2009914967602,-14.7669045823054,48.7578764229251));
#19635=CARTESIAN_POINT('Ctrl Pts',(29.9297290637873,-14.7669045823054,48.8151106090292));
#19636=CARTESIAN_POINT('Ctrl Pts',(29.7431850567499,-14.7669045823054,48.8324317919394));
#19637=CARTESIAN_POINT('Ctrl Pts',(29.5568100599416,-14.7669045823054,48.8324317919394));
#19638=CARTESIAN_POINT('',(-30.4628904239763,-14.7669045823054,-48.4165189096496));
#19639=CARTESIAN_POINT('',(-43.0351235939456,-14.7669045823054,-37.6801663496809));
#19640=CARTESIAN_POINT('Origin',(0.0835265683620477,-14.7669045823054,0.0824317919394229));
#19641=CARTESIAN_POINT('',(-42.442236506563,-14.7669045823054,-36.6450210147876));
#19642=CARTESIAN_POINT('Ctrl Pts',(-43.0351235939456,-14.7669045823054,
-37.6801663496809));
#19643=CARTESIAN_POINT('Ctrl Pts',(-43.0493934245332,-14.7669045823054,
-37.663872559972));
#19644=CARTESIAN_POINT('Ctrl Pts',(-43.0624522636822,-14.7669045823054,
-37.6466628364843));
#19645=CARTESIAN_POINT('Ctrl Pts',(-43.0742010215879,-14.7669045823054,
-37.6286768778889));
#19646=CARTESIAN_POINT('Ctrl Pts',(-43.085785082681,-14.7669045823054,-37.6109430506316));
#19647=CARTESIAN_POINT('Ctrl Pts',(-43.0960964702708,-14.7669045823054,
-37.5924534940372));
#19648=CARTESIAN_POINT('Ctrl Pts',(-43.1050061468023,-14.7669045823054,
-37.5733068936262));
#19649=CARTESIAN_POINT('Ctrl Pts',(-43.1117884961925,-14.7669045823054,
-37.5587318489358));
#19650=CARTESIAN_POINT('Ctrl Pts',(-43.1177580209636,-14.7669045823054,
-37.5437752524041));
#19651=CARTESIAN_POINT('Ctrl Pts',(-43.1228391763247,-14.7669045823054,
-37.5284723355379));
#19652=CARTESIAN_POINT('Ctrl Pts',(-43.1228397887615,-14.7669045823054,
-37.5284704910619));
#19653=CARTESIAN_POINT('Ctrl Pts',(-43.1228404011851,-14.7669045823054,
-37.5284686465814));
#19654=CARTESIAN_POINT('Ctrl Pts',(-43.1228410135956,-14.7669045823054,
-37.5284668020966));
#19655=CARTESIAN_POINT('Ctrl Pts',(-43.1413654459984,-14.7669045823054,
-37.4726741040998));
#19656=CARTESIAN_POINT('Ctrl Pts',(-43.1478436164141,-14.7669045823054,
-37.4131063670338));
#19657=CARTESIAN_POINT('Ctrl Pts',(-43.1432612445211,-14.7669045823054,
-37.3546291623973));
#19658=CARTESIAN_POINT('Ctrl Pts',(-43.143260941538,-14.7669045823054,-37.3546252959278));
#19659=CARTESIAN_POINT('Ctrl Pts',(-43.1432606385066,-14.7669045823054,
-37.354621429463));
#19660=CARTESIAN_POINT('Ctrl Pts',(-43.1432603354269,-14.7669045823054,
-37.354617563003));
#19661=CARTESIAN_POINT('Ctrl Pts',(-43.134092666425,-14.7669045823054,-37.2376634422313));
#19662=CARTESIAN_POINT('Ctrl Pts',(-43.0822830950826,-14.7669045823054,
-37.1265992604543));
#19663=CARTESIAN_POINT('Ctrl Pts',(-43.0121454822292,-14.7669045823054,
-37.0329127314283));
#19664=CARTESIAN_POINT('Ctrl Pts',(-43.0121408447823,-14.7669045823054,
-37.0329065369446));
#19665=CARTESIAN_POINT('Ctrl Pts',(-43.0121362072495,-14.7669045823054,
-37.0329003425378));
#19666=CARTESIAN_POINT('Ctrl Pts',(-43.0121315696307,-14.7669045823054,
-37.0328941482078));
#19667=CARTESIAN_POINT('Ctrl Pts',(-43.0033683906757,-14.7669045823054,
-37.0211894298772));
#19668=CARTESIAN_POINT('Ctrl Pts',(-42.994312018525,-14.7669045833006,-37.0097193709685));
#19669=CARTESIAN_POINT('Ctrl Pts',(-42.9849832169969,-14.7669045783028,
-36.9984827580438));
#19670=CARTESIAN_POINT('Ctrl Pts',(-42.9626179933785,-14.7669045663207,
-36.9715436748167));
#19671=CARTESIAN_POINT('Ctrl Pts',(-42.9386878379802,-14.766904502036,-36.9459412828177));
#19672=CARTESIAN_POINT('Ctrl Pts',(-42.9134773012134,-14.7669043153494,
-36.9216690341282));
#19673=CARTESIAN_POINT('Ctrl Pts',(-42.9018637058227,-14.7669042293495,
-36.9104876745995));
#19674=CARTESIAN_POINT('Ctrl Pts',(-42.8899785749099,-14.766904120834,-36.8995878484045));
#19675=CARTESIAN_POINT('Ctrl Pts',(-42.877850269258,-14.7669040086953,-36.8889652900115));
#19676=CARTESIAN_POINT('Ctrl Pts',(-42.8586221872063,-14.7669038309118,
-36.8721244030615));
#19677=CARTESIAN_POINT('Ctrl Pts',(-42.8387822388114,-14.7669036396173,
-36.8559847566146));
#19678=CARTESIAN_POINT('Ctrl Pts',(-42.8184420673977,-14.7669035207875,
-36.8405391935086));
#19679=CARTESIAN_POINT('Ctrl Pts',(-42.8082719816908,-14.7669034613726,
-36.8328164119555));
#19680=CARTESIAN_POINT('Ctrl Pts',(-42.7979768402275,-14.7669034201738,
-36.8252671512432));
#19681=CARTESIAN_POINT('Ctrl Pts',(-42.7875705984364,-14.7669034045806,
-36.8178905167261));
#19682=CARTESIAN_POINT('Ctrl Pts',(-42.7771643566452,-14.7669033889875,
-36.810513882209));
#19683=CARTESIAN_POINT('Ctrl Pts',(-42.7666470145257,-14.7669033991487,
-36.8033098738887));
#19684=CARTESIAN_POINT('Ctrl Pts',(-42.7560325275328,-14.7669034367692,
-36.7962775970873));
#19685=CARTESIAN_POINT('Ctrl Pts',(-42.7284821013409,-14.766903534415,-36.7780249746943));
#19686=CARTESIAN_POINT('Ctrl Pts',(-42.7002748680626,-14.7669038199043,
-36.7609197163093));
#19687=CARTESIAN_POINT('Ctrl Pts',(-42.6714540246378,-14.7669040506412,
-36.7449251182321));
#19688=CARTESIAN_POINT('Ctrl Pts',(-42.6495139682548,-14.7669042262912,
-36.7327491253764));
#19689=CARTESIAN_POINT('Ctrl Pts',(-42.6272177630288,-14.7669043666507,
-36.7212179378421));
#19690=CARTESIAN_POINT('Ctrl Pts',(-42.6045814981569,-14.766904445574,-36.7103352441939));
#19691=CARTESIAN_POINT('Ctrl Pts',(-42.5719197020778,-14.7669045594521,
-36.694632639425));
#19692=CARTESIAN_POINT('Ctrl Pts',(-42.5385519910219,-14.7669045735796,
-36.6802740464539));
#19693=CARTESIAN_POINT('Ctrl Pts',(-42.5045304592707,-14.7669045795915,
-36.6672211825363));
#19694=CARTESIAN_POINT('Ctrl Pts',(-42.4840000585715,-14.7669045832193,
-36.6593443906135));
#19695=CARTESIAN_POINT('Ctrl Pts',(-42.4632313478216,-14.7669045823054,
-36.6519440751797));
#19696=CARTESIAN_POINT('Ctrl Pts',(-42.442236506563,-14.7669045823054,-36.6450210147876));
#19697=CARTESIAN_POINT('',(6.83612114566778,-14.7669045823054,-20.3954556167886));
#19698=CARTESIAN_POINT('',(6.83612114566778,-14.7669045823054,-20.3954556167886));
#19699=CARTESIAN_POINT('Origin',(0.0835265683620477,-14.7669045823054,0.0824317919394229));
#19700=CARTESIAN_POINT('',(32.4575305290195,-14.7669045823054,-46.3554507110303));
#19701=CARTESIAN_POINT('',(24.3171104787687,-14.7669045823054,-21.6688501250819));
#19702=CARTESIAN_POINT('',(32.2559828833067,-14.7669045823054,-47.3534709072605));
#19703=CARTESIAN_POINT('Ctrl Pts',(32.2559828833067,-14.7669045823054,-47.3534709072605));
#19704=CARTESIAN_POINT('Ctrl Pts',(32.2607343242407,-14.7669045823054,-47.3502483269737));
#19705=CARTESIAN_POINT('Ctrl Pts',(32.2654163986591,-14.7669045824339,-47.3469423857629));
#19706=CARTESIAN_POINT('Ctrl Pts',(32.2700293048561,-14.7669045818318,-47.343556443888));
#19707=CARTESIAN_POINT('Ctrl Pts',(32.2875531747034,-14.7669045795448,-47.3306936623373));
#19708=CARTESIAN_POINT('Ctrl Pts',(32.3040911700412,-14.766904560918,-47.3166798601742));
#19709=CARTESIAN_POINT('Ctrl Pts',(32.3196301239233,-14.7669044772679,-47.3016933745717));
#19710=CARTESIAN_POINT('Ctrl Pts',(32.3347692125982,-14.7669043957704,-47.2870925374637));
#19711=CARTESIAN_POINT('Ctrl Pts',(32.3489605420936,-14.7669042476547,-47.2715690661388));
#19712=CARTESIAN_POINT('Ctrl Pts',(32.3622379419634,-14.7669041441791,-47.255300171139));
#19713=CARTESIAN_POINT('Ctrl Pts',(32.3689643151124,-14.7669040917581,-47.2470582970099));
#19714=CARTESIAN_POINT('Ctrl Pts',(32.3754531347727,-14.7669040484303,-47.2386243425884));
#19715=CARTESIAN_POINT('Ctrl Pts',(32.3817058008036,-14.7669040210232,-47.2300205947939));
#19716=CARTESIAN_POINT('Ctrl Pts',(32.3840505505652,-14.7669040107455,-47.226794189371));
#19717=CARTESIAN_POINT('Ctrl Pts',(32.3863620912228,-14.7669040026344,-47.2235439067552));
#19718=CARTESIAN_POINT('Ctrl Pts',(32.3886404965979,-14.7669039967743,-47.220270922234));
#19719=CARTESIAN_POINT('Ctrl Pts',(32.390634101301,-14.7669039916468,-47.217407060778));
#19720=CARTESIAN_POINT('Ctrl Pts',(32.3926023368035,-14.7669039882399,-47.2145258181757));
#19721=CARTESIAN_POINT('Ctrl Pts',(32.3945452525602,-14.7669039865145,-47.2116279817781));
#19722=CARTESIAN_POINT('Ctrl Pts',(32.4081456628571,-14.7669039744365,-47.1913431269954));
#19723=CARTESIAN_POINT('Ctrl Pts',(32.4205054055829,-14.7669040526285,-47.1702451762436));
#19724=CARTESIAN_POINT('Ctrl Pts',(32.4316414440808,-14.7669041305354,-47.1486041910527));
#19725=CARTESIAN_POINT('Ctrl Pts',(32.4463626886987,-14.7669042335241,-47.1199959712781));
#19726=CARTESIAN_POINT('Ctrl Pts',(32.4590542802873,-14.7669043748298,-47.0903042649473));
#19727=CARTESIAN_POINT('Ctrl Pts',(32.4698771491973,-14.7669044578905,-47.0598955592365));
#19728=CARTESIAN_POINT('Ctrl Pts',(32.4742625549281,-14.7669044915466,-47.0475740099875));
#19729=CARTESIAN_POINT('Ctrl Pts',(32.4783405165562,-14.7669045170158,-47.0351346693419));
#19730=CARTESIAN_POINT('Ctrl Pts',(32.4821193826036,-14.7669045346655,-47.0226018965824));
#19731=CARTESIAN_POINT('Ctrl Pts',(32.4931992952929,-14.7669045864155,-46.9858548867149));
#19732=CARTESIAN_POINT('Ctrl Pts',(32.5017169636477,-14.7669045820527,-46.9483049513178));
#19733=CARTESIAN_POINT('Ctrl Pts',(32.5079293060509,-14.7669045822747,-46.9105654690864));
#19734=CARTESIAN_POINT('Ctrl Pts',(32.5090631880298,-14.7669045823153,-46.9036772269361));
#19735=CARTESIAN_POINT('Ctrl Pts',(32.5101201315568,-14.7669045823054,-46.8967826857539));
#19736=CARTESIAN_POINT('Ctrl Pts',(32.5111015211428,-14.7669045823054,-46.8898856260792));
#19737=CARTESIAN_POINT('Ctrl Pts',(32.5111027879795,-14.7669045823054,-46.8898767229402));
#19738=CARTESIAN_POINT('Ctrl Pts',(32.511104054695,-14.7669045823054,-46.8898678197768));
#19739=CARTESIAN_POINT('Ctrl Pts',(32.5111053212894,-14.7669045823054,-46.889858916589));
#19740=CARTESIAN_POINT('Ctrl Pts',(32.5142844731562,-14.7669045823054,-46.8675119167502));
#19741=CARTESIAN_POINT('Ctrl Pts',(32.5166905301417,-14.7669045826373,-46.8449996927378));
#19742=CARTESIAN_POINT('Ctrl Pts',(32.5183630494517,-14.7669045772469,-46.8224057278094));
#19743=CARTESIAN_POINT('Ctrl Pts',(32.5208718284167,-14.7669045691613,-46.7885147804168));
#19744=CARTESIAN_POINT('Ctrl Pts',(32.5217301481929,-14.766904546284,-46.7544399152559));
#19745=CARTESIAN_POINT('Ctrl Pts',(32.5210714668687,-14.7669045319054,-46.7204628780165));
#19746=CARTESIAN_POINT('Ctrl Pts',(32.5204127855445,-14.7669045175269,-46.6864858407771));
#19747=CARTESIAN_POINT('Ctrl Pts',(32.5182371031102,-14.7669045165844,-46.6526066314599));
#19748=CARTESIAN_POINT('Ctrl Pts',(32.5146778776706,-14.7669045221653,-46.6191069957584));
#19749=CARTESIAN_POINT('Ctrl Pts',(32.5111794725999,-14.7669045276508,-46.5861798048872));
#19750=CARTESIAN_POINT('Ctrl Pts',(32.5063452043462,-14.766904544103,-46.553462859021));
#19751=CARTESIAN_POINT('Ctrl Pts',(32.5002291656841,-14.7669045570257,-46.5209360093445));
#19752=CARTESIAN_POINT('Ctrl Pts',(32.4940445072357,-14.7669045700934,-46.4880442199424));
#19753=CARTESIAN_POINT('Ctrl Pts',(32.4865486002504,-14.7669045784001,-46.4553458854947));
#19754=CARTESIAN_POINT('Ctrl Pts',(32.4777487169981,-14.7669045808678,-46.4228403401102));
#19755=CARTESIAN_POINT('Ctrl Pts',(32.4716414149088,-14.7669045825804,-46.4002808152224));
#19756=CARTESIAN_POINT('Ctrl Pts',(32.4649050132712,-14.7669045823054,-46.3778145456801));
#19757=CARTESIAN_POINT('Ctrl Pts',(32.4575305290195,-14.7669045823054,-46.3554507110304));
#19758=CARTESIAN_POINT('',(30.6299435607004,-14.7669045823054,-48.4165189096496));
#19759=CARTESIAN_POINT('Origin',(0.0835265683620477,-14.7669045823054,0.0824317919394229));
#19760=CARTESIAN_POINT('',(29.5568100599416,-14.7669045823054,-48.6675682080606));
#19761=CARTESIAN_POINT('Ctrl Pts',(29.5568100599416,-14.7669045823054,-48.6675682080606));
#19762=CARTESIAN_POINT('Ctrl Pts',(29.687226059415,-14.7669045823054,-48.6675682069665));
#19763=CARTESIAN_POINT('Ctrl Pts',(29.8164312767719,-14.7669045823175,-48.6592516832571));
#19764=CARTESIAN_POINT('Ctrl Pts',(29.9442057515289,-14.7669045822917,-48.6412585834828));
#19765=CARTESIAN_POINT('Ctrl Pts',(29.9988450488462,-14.7669045822807,-48.6335643211499));
#19766=CARTESIAN_POINT('Ctrl Pts',(30.0532227864462,-14.7669045822601,-48.6241012172608));
#19767=CARTESIAN_POINT('Ctrl Pts',(30.1073220850124,-14.7669045822063,-48.6127658445173));
#19768=CARTESIAN_POINT('Ctrl Pts',(30.1078450912829,-14.7669045822058,-48.6126562595285));
#19769=CARTESIAN_POINT('Ctrl Pts',(30.1083681026981,-14.7669045822053,-48.6125465072483));
#19770=CARTESIAN_POINT('Ctrl Pts',(30.1088911186622,-14.7669045822047,-48.6124365871634));
#19771=CARTESIAN_POINT('Ctrl Pts',(30.1758594224764,-14.7669045821373,-48.5983621379247));
#19772=CARTESIAN_POINT('Ctrl Pts',(30.2427679718073,-14.7669045821586,-48.5815717818007));
#19773=CARTESIAN_POINT('Ctrl Pts',(30.3085555596271,-14.7669045822031,-48.5609664254967));
#19774=CARTESIAN_POINT('Ctrl Pts',(30.3646336248817,-14.7669045822411,-48.5434021925814));
#19775=CARTESIAN_POINT('Ctrl Pts',(30.4198994743272,-14.766904582279,-48.5230669892512));
#19776=CARTESIAN_POINT('Ctrl Pts',(30.473690093401,-14.7669045822933,-48.4992416030476));
#19777=CARTESIAN_POINT('Ctrl Pts',(30.5206443189021,-14.7669045823058,-48.4784442488673));
#19778=CARTESIAN_POINT('Ctrl Pts',(30.5664751505883,-14.7669045823054,-48.454987627778));
#19779=CARTESIAN_POINT('Ctrl Pts',(30.6107202044109,-14.7669045823054,-48.4283554531363));
#19780=CARTESIAN_POINT('Ctrl Pts',(30.6171621507609,-14.7669045823054,-48.4244778888573));
#19781=CARTESIAN_POINT('Ctrl Pts',(30.6235704304707,-14.7669045823054,-48.4205329323747));
#19782=CARTESIAN_POINT('Ctrl Pts',(30.6299435607004,-14.7669045823054,-48.4165189096496));
#19783=CARTESIAN_POINT('',(-29.3897569232175,-14.7669045823054,-48.6675682080606));
#19784=CARTESIAN_POINT('',(-30.3174396991762,-14.7669045823054,-48.6675682080606));
#19785=CARTESIAN_POINT('Ctrl Pts',(-30.4628904239763,-14.7669045823054,
-48.4165189096496));
#19786=CARTESIAN_POINT('Ctrl Pts',(-30.383617379776,-14.7669045823054,-48.4664479788226));
#19787=CARTESIAN_POINT('Ctrl Pts',(-30.2980162042778,-14.7669045823054,
-48.5052983546113));
#19788=CARTESIAN_POINT('Ctrl Pts',(-30.1231196682765,-14.7669045823054,
-48.568676241689));
#19789=CARTESIAN_POINT('Ctrl Pts',(-30.0339383600361,-14.7669045823054,
-48.5930128390463));
#19790=CARTESIAN_POINT('Ctrl Pts',(-29.7626759270632,-14.7669045823054,
-48.6502470251504));
#19791=CARTESIAN_POINT('Ctrl Pts',(-29.5761319200258,-14.7669045823054,
-48.6675682080606));
#19792=CARTESIAN_POINT('Ctrl Pts',(-29.3897569232175,-14.7669045823054,
-48.6675682080606));
#19793=CARTESIAN_POINT('',(-20.394360840366,-14.7669045823054,-6.6701627853663));
#19794=CARTESIAN_POINT('',(-9.75726988530523,-14.7669045823054,-19.1035039790228));
#19795=CARTESIAN_POINT('Origin',(0.0835265683620477,-14.7669045823054,0.0824317919394229));
#19796=CARTESIAN_POINT('',(-9.84678298317079,-14.7669045823054,-20.2531800132168));
#19797=CARTESIAN_POINT('Origin',(-10.0425103622231,-14.7669045823054,-19.6596180593406));
#19798=CARTESIAN_POINT('',(-46.3543559346078,-14.7669045823054,-32.2915721687179));
#19799=CARTESIAN_POINT('',(-48.0630165107499,-14.7669045823054,-32.8550039285778));
#19800=CARTESIAN_POINT('',(-47.352376130838,-14.7669045823054,-32.090024523005));
#19801=CARTESIAN_POINT('Ctrl Pts',(-47.352376130838,-14.7669045823054,-32.090024523005));
#19802=CARTESIAN_POINT('Ctrl Pts',(-47.3491535505513,-14.7669045823054,
-32.0947759639391));
#19803=CARTESIAN_POINT('Ctrl Pts',(-47.3458476093404,-14.7669045824339,
-32.0994580383575));
#19804=CARTESIAN_POINT('Ctrl Pts',(-47.3424616674655,-14.7669045818319,
-32.1040709445545));
#19805=CARTESIAN_POINT('Ctrl Pts',(-47.3295988859157,-14.7669045795448,
-32.1215948144007));
#19806=CARTESIAN_POINT('Ctrl Pts',(-47.3155850837535,-14.766904560918,-32.1381328097375));
#19807=CARTESIAN_POINT('Ctrl Pts',(-47.300598598152,-14.7669044772679,-32.1536717636188));
#19808=CARTESIAN_POINT('Ctrl Pts',(-47.2859977610431,-14.7669043957704,
-32.1688108522948));
#19809=CARTESIAN_POINT('Ctrl Pts',(-47.2704742897173,-14.7669042476547,
-32.1830021817911));
#19810=CARTESIAN_POINT('Ctrl Pts',(-47.2542053947165,-14.7669041441791,
-32.1962795816618));
#19811=CARTESIAN_POINT('Ctrl Pts',(-47.2459635205874,-14.7669040917581,
-32.2030059548108));
#19812=CARTESIAN_POINT('Ctrl Pts',(-47.2375295661659,-14.7669040484303,
-32.2094947744711));
#19813=CARTESIAN_POINT('Ctrl Pts',(-47.2289258183714,-14.7669040210232,
-32.215747440502));
#19814=CARTESIAN_POINT('Ctrl Pts',(-47.2256994129485,-14.7669040107455,
-32.2180921902636));
#19815=CARTESIAN_POINT('Ctrl Pts',(-47.2224491303327,-14.7669040026344,
-32.2204037309212));
#19816=CARTESIAN_POINT('Ctrl Pts',(-47.2191761458115,-14.7669039967743,
-32.2226821362962));
#19817=CARTESIAN_POINT('Ctrl Pts',(-47.2163122843555,-14.7669039916467,
-32.2246757409994));
#19818=CARTESIAN_POINT('Ctrl Pts',(-47.2134310417532,-14.7669039882399,
-32.2266439765019));
#19819=CARTESIAN_POINT('Ctrl Pts',(-47.2105332053557,-14.7669039865145,
-32.2285868922586));
#19820=CARTESIAN_POINT('Ctrl Pts',(-47.190248350573,-14.7669039744365,-32.2421873025555));
#19821=CARTESIAN_POINT('Ctrl Pts',(-47.1691503998211,-14.7669040526285,
-32.2545470452812));
#19822=CARTESIAN_POINT('Ctrl Pts',(-47.1475094146302,-14.7669041305354,
-32.2656830837792));
#19823=CARTESIAN_POINT('Ctrl Pts',(-47.1189011948645,-14.7669042335241,
-32.2804043283925));
#19824=CARTESIAN_POINT('Ctrl Pts',(-47.0892094885433,-14.7669043748298,
-32.2930959199778));
#19825=CARTESIAN_POINT('Ctrl Pts',(-47.0588007828424,-14.7669044578905,
-32.3039187888855));
#19826=CARTESIAN_POINT('Ctrl Pts',(-47.0464792335841,-14.7669044915466,
-32.3083041946202));
#19827=CARTESIAN_POINT('Ctrl Pts',(-47.034039892929,-14.7669045170158,-32.3123821562517));
#19828=CARTESIAN_POINT('Ctrl Pts',(-47.0215071201599,-14.7669045346655,
-32.3161610223019));
#19829=CARTESIAN_POINT('Ctrl Pts',(-46.984760110287,-14.7669045864155,-32.3272409349929));
#19830=CARTESIAN_POINT('Ctrl Pts',(-46.9472101748842,-14.7669045820527,
-32.3357586033484));
#19831=CARTESIAN_POINT('Ctrl Pts',(-46.9094706926473,-14.7669045822747,
-32.3419709457519));
#19832=CARTESIAN_POINT('Ctrl Pts',(-46.9025824505025,-14.7669045823153,
-32.3431048277297));
#19833=CARTESIAN_POINT('Ctrl Pts',(-46.8956879093258,-14.7669045823054,
-32.3441617712558));
#19834=CARTESIAN_POINT('Ctrl Pts',(-46.8887908496566,-14.7669045823054,
-32.3451431608411));
#19835=CARTESIAN_POINT('Ctrl Pts',(-46.8887819465176,-14.7669045823054,
-32.3451444276778));
#19836=CARTESIAN_POINT('Ctrl Pts',(-46.8887730433543,-14.7669045823054,
-32.3451456943933));
#19837=CARTESIAN_POINT('Ctrl Pts',(-46.8887641401665,-14.7669045823054,
-32.3451469609878));
#19838=CARTESIAN_POINT('Ctrl Pts',(-46.8664171403277,-14.7669045823054,
-32.3483261128546));
#19839=CARTESIAN_POINT('Ctrl Pts',(-46.8439049163153,-14.7669045826373,
-32.3507321698401));
#19840=CARTESIAN_POINT('Ctrl Pts',(-46.8213109513869,-14.7669045772469,
-32.3524046891501));
#19841=CARTESIAN_POINT('Ctrl Pts',(-46.7874200039943,-14.7669045691613,
-32.3549134681151));
#19842=CARTESIAN_POINT('Ctrl Pts',(-46.7533451388334,-14.766904546284,-32.3557717878912));
#19843=CARTESIAN_POINT('Ctrl Pts',(-46.719368101594,-14.7669045319054,-32.355113106567));
#19844=CARTESIAN_POINT('Ctrl Pts',(-46.6853910643546,-14.7669045175269,
-32.3544544252428));
#19845=CARTESIAN_POINT('Ctrl Pts',(-46.6515118550373,-14.7669045165844,
-32.3522787428086));
#19846=CARTESIAN_POINT('Ctrl Pts',(-46.6180122193358,-14.7669045221653,
-32.348719517369));
#19847=CARTESIAN_POINT('Ctrl Pts',(-46.585085028464,-14.7669045276508,-32.3452211122982));
#19848=CARTESIAN_POINT('Ctrl Pts',(-46.5523680825972,-14.766904544103,-32.3403868440443));
#19849=CARTESIAN_POINT('Ctrl Pts',(-46.5198412329201,-14.7669045570257,
-32.334270805382));
#19850=CARTESIAN_POINT('Ctrl Pts',(-46.4869494435169,-14.7669045700934,
-32.3280861469334));
#19851=CARTESIAN_POINT('Ctrl Pts',(-46.4542511090682,-14.7669045784001,
-32.3205902399477));
#19852=CARTESIAN_POINT('Ctrl Pts',(-46.4217455636826,-14.7669045808678,
-32.311790356695));
#19853=CARTESIAN_POINT('Ctrl Pts',(-46.3991860387965,-14.7669045825804,
-32.305683054606));
#19854=CARTESIAN_POINT('Ctrl Pts',(-46.3767197692559,-14.7669045823054,
-32.298946652969));
#19855=CARTESIAN_POINT('Ctrl Pts',(-46.3543559346078,-14.7669045823054,
-32.2915721687179));
#19856=CARTESIAN_POINT('',(-48.415424133227,-14.7669045823054,-30.4639852003989));
#19857=CARTESIAN_POINT('Origin',(0.0835265683620477,-14.7669045823054,0.0824317919394229));
#19858=CARTESIAN_POINT('',(-48.6664734316379,-14.7669045823054,-29.3908516996402));
#19859=CARTESIAN_POINT('Ctrl Pts',(-48.6664734316379,-14.7669045823054,
-29.3908516996402));
#19860=CARTESIAN_POINT('Ctrl Pts',(-48.6664734305346,-14.7669045823054,
-29.5212452714537));
#19861=CARTESIAN_POINT('Ctrl Pts',(-48.658159503563,-14.7669045823177,-29.6504238593144));
#19862=CARTESIAN_POINT('Ctrl Pts',(-48.6401750099693,-14.7669045822915,
-29.778166914327));
#19863=CARTESIAN_POINT('Ctrl Pts',(-48.6324798641135,-14.7669045822804,
-29.8328251917631));
#19864=CARTESIAN_POINT('Ctrl Pts',(-48.6230148766798,-14.7669045822595,
-29.8872207222031));
#19865=CARTESIAN_POINT('Ctrl Pts',(-48.6116767039643,-14.7669045822049,
-29.9413365514922));
#19866=CARTESIAN_POINT('Ctrl Pts',(-48.6115666059104,-14.7669045822044,
-29.9418620371803));
#19867=CARTESIAN_POINT('Ctrl Pts',(-48.6114563389905,-14.7669045822038,
-29.9423875282861));
#19868=CARTESIAN_POINT('Ctrl Pts',(-48.6113459026832,-14.7669045822033,
-29.9429130242052));
#19869=CARTESIAN_POINT('Ctrl Pts',(-48.5971465642682,-14.7669045821343,
-30.0104786153631));
#19870=CARTESIAN_POINT('Ctrl Pts',(-48.5801820330883,-14.7669045821572,
-30.0779908271464));
#19871=CARTESIAN_POINT('Ctrl Pts',(-48.559321523009,-14.7669045822029,-30.1443546643599));
#19872=CARTESIAN_POINT('Ctrl Pts',(-48.5417918489716,-14.7669045822413,
-30.2001220655312));
#19873=CARTESIAN_POINT('Ctrl Pts',(-48.5215119330852,-14.7669045822791,
-30.2550807409539));
#19874=CARTESIAN_POINT('Ctrl Pts',(-48.4977739691264,-14.7669045822934,
-30.3085755625293));
#19875=CARTESIAN_POINT('Ctrl Pts',(-48.4767816374474,-14.766904582306,-30.3558829491095));
#19876=CARTESIAN_POINT('Ctrl Pts',(-48.4530851649729,-14.7669045823054,
-30.4020462550889));
#19877=CARTESIAN_POINT('Ctrl Pts',(-48.4261572648105,-14.7669045823054,
-30.4465911244048));
#19878=CARTESIAN_POINT('Ctrl Pts',(-48.4226353067432,-14.7669045823054,
-30.4524172438162));
#19879=CARTESIAN_POINT('Ctrl Pts',(-48.4190580087251,-14.7669045823054,
-30.4582156362162));
#19880=CARTESIAN_POINT('Ctrl Pts',(-48.415424133227,-14.7669045823054,-30.4639852003989));
#19881=CARTESIAN_POINT('',(-48.6664734316379,-14.7669045823054,29.555715283519));
#19882=CARTESIAN_POINT('',(-48.6664734316379,-14.7669045823054,30.4833980594772));
#19883=CARTESIAN_POINT('',(-48.415424133227,-14.7669045823054,30.6288487842778));
#19884=CARTESIAN_POINT('Ctrl Pts',(-48.415424133227,-14.7669045823054,30.6288487842778));
#19885=CARTESIAN_POINT('Ctrl Pts',(-48.4653532024,-14.7669045823054,30.5495757400775));
#19886=CARTESIAN_POINT('Ctrl Pts',(-48.5042035781887,-14.7669045823054,
30.4639745645792));
#19887=CARTESIAN_POINT('Ctrl Pts',(-48.5675814652663,-14.7669045823054,
30.2890780285779));
#19888=CARTESIAN_POINT('Ctrl Pts',(-48.5919180626237,-14.7669045823054,
30.1998967203376));
#19889=CARTESIAN_POINT('Ctrl Pts',(-48.6491522487277,-14.7669045823054,
29.9286342873647));
#19890=CARTESIAN_POINT('Ctrl Pts',(-48.666473431638,-14.7669045823054,29.7420902803272));
#19891=CARTESIAN_POINT('Ctrl Pts',(-48.6664734316379,-14.7669045823054,
29.555715283519));
#19892=CARTESIAN_POINT('',(-37.6790715732587,-14.7669045823054,43.2010819542467));
#19893=CARTESIAN_POINT('Origin',(0.0835265683620477,-14.7669045823054,0.0824317919394229));
#19894=CARTESIAN_POINT('',(-36.6439262383654,-14.7669045823054,42.6081948668641));
#19895=CARTESIAN_POINT('Ctrl Pts',(-37.6790715732587,-14.7669045823054,
43.2010819542467));
#19896=CARTESIAN_POINT('Ctrl Pts',(-37.6627777835487,-14.7669045823054,
43.2153517848353));
#19897=CARTESIAN_POINT('Ctrl Pts',(-37.6455680600597,-14.7669045823054,
43.2284106239852));
#19898=CARTESIAN_POINT('Ctrl Pts',(-37.6275821014629,-14.7669045823054,
43.2401593818916));
#19899=CARTESIAN_POINT('Ctrl Pts',(-37.6098482742043,-14.7669045823054,
43.2517434429853));
#19900=CARTESIAN_POINT('Ctrl Pts',(-37.5913587176086,-14.7669045823054,
43.2620548305755));
#19901=CARTESIAN_POINT('Ctrl Pts',(-37.5722121171962,-14.7669045823054,
43.2709645071072));
#19902=CARTESIAN_POINT('Ctrl Pts',(-37.5576370725083,-14.7669045823054,
43.2777468564959));
#19903=CARTESIAN_POINT('Ctrl Pts',(-37.5426804759792,-14.7669045823054,
43.2837163812658));
#19904=CARTESIAN_POINT('Ctrl Pts',(-37.5273775591158,-14.7669045823054,
43.2887975366259));
#19905=CARTESIAN_POINT('Ctrl Pts',(-37.5273757146397,-14.7669045823054,
43.2887981490627));
#19906=CARTESIAN_POINT('Ctrl Pts',(-37.5273738701592,-14.7669045823054,
43.2887987614863));
#19907=CARTESIAN_POINT('Ctrl Pts',(-37.5273720256744,-14.7669045823054,
43.2887993738968));
#19908=CARTESIAN_POINT('Ctrl Pts',(-37.4715793276776,-14.7669045823054,
43.3073238062995));
#19909=CARTESIAN_POINT('Ctrl Pts',(-37.4120115906116,-14.7669045823054,
43.313801976715));
#19910=CARTESIAN_POINT('Ctrl Pts',(-37.3535343859751,-14.7669045823054,
43.309219604822));
#19911=CARTESIAN_POINT('Ctrl Pts',(-37.3535305195056,-14.7669045823054,
43.309219301839));
#19912=CARTESIAN_POINT('Ctrl Pts',(-37.3535266530408,-14.7669045823054,
43.3092189988076));
#19913=CARTESIAN_POINT('Ctrl Pts',(-37.3535227865809,-14.7669045823054,
43.3092186957278));
#19914=CARTESIAN_POINT('Ctrl Pts',(-37.2365686658092,-14.7669045823054,
43.3000510267261));
#19915=CARTESIAN_POINT('Ctrl Pts',(-37.1255044840321,-14.7669045823054,
43.2482414553837));
#19916=CARTESIAN_POINT('Ctrl Pts',(-37.0318179550061,-14.7669045823054,
43.1781038425302));
#19917=CARTESIAN_POINT('Ctrl Pts',(-37.0318117605224,-14.7669045823054,
43.1780992050834));
#19918=CARTESIAN_POINT('Ctrl Pts',(-37.0318055661156,-14.7669045823054,
43.1780945675506));
#19919=CARTESIAN_POINT('Ctrl Pts',(-37.0317993717856,-14.7669045823054,
43.1780899299318));
#19920=CARTESIAN_POINT('Ctrl Pts',(-37.020094653455,-14.7669045823054,43.1693267509767));
#19921=CARTESIAN_POINT('Ctrl Pts',(-37.0086245945463,-14.7669045833006,
43.160270378826));
#19922=CARTESIAN_POINT('Ctrl Pts',(-36.9973879816216,-14.7669045783028,
43.1509415772979));
#19923=CARTESIAN_POINT('Ctrl Pts',(-36.9704488983943,-14.7669045663207,
43.1285763536794));
#19924=CARTESIAN_POINT('Ctrl Pts',(-36.9448465063951,-14.766904502036,43.1046461982809));
#19925=CARTESIAN_POINT('Ctrl Pts',(-36.9205742577055,-14.7669043153494,
43.0794356615139));
#19926=CARTESIAN_POINT('Ctrl Pts',(-36.9093928981769,-14.7669042293495,
43.0678220661234));
#19927=CARTESIAN_POINT('Ctrl Pts',(-36.8984930719822,-14.766904120834,43.0559369352108));
#19928=CARTESIAN_POINT('Ctrl Pts',(-36.8878705135893,-14.7669040086953,
43.043808629559));
#19929=CARTESIAN_POINT('Ctrl Pts',(-36.8710296266393,-14.7669038309118,
43.0245805475074));
#19930=CARTESIAN_POINT('Ctrl Pts',(-36.8548899801924,-14.7669036396173,
43.0047405991125));
#19931=CARTESIAN_POINT('Ctrl Pts',(-36.8394444170864,-14.7669035207875,
42.9844004276988));
#19932=CARTESIAN_POINT('Ctrl Pts',(-36.8317216355334,-14.7669034613726,
42.9742303419919));
#19933=CARTESIAN_POINT('Ctrl Pts',(-36.824172374821,-14.7669034201738,42.9639352005286));
#19934=CARTESIAN_POINT('Ctrl Pts',(-36.8167957403039,-14.7669034045806,
42.9535289587375));
#19935=CARTESIAN_POINT('Ctrl Pts',(-36.8094191057869,-14.7669033889875,
42.9431227169463));
#19936=CARTESIAN_POINT('Ctrl Pts',(-36.8022150974665,-14.7669033991487,
42.9326053748268));
#19937=CARTESIAN_POINT('Ctrl Pts',(-36.7951828206651,-14.7669034367692,
42.9219908878338));
#19938=CARTESIAN_POINT('Ctrl Pts',(-36.7769301982716,-14.766903534415,42.8944404616412));
#19939=CARTESIAN_POINT('Ctrl Pts',(-36.7598249398862,-14.7669038199043,
42.8662332283621));
#19940=CARTESIAN_POINT('Ctrl Pts',(-36.7438303418086,-14.7669040506412,
42.8374123849365));
#19941=CARTESIAN_POINT('Ctrl Pts',(-36.7316543489533,-14.7669042262912,
42.8154723285542));
#19942=CARTESIAN_POINT('Ctrl Pts',(-36.7201231614195,-14.7669043666507,
42.793176123329));
#19943=CARTESIAN_POINT('Ctrl Pts',(-36.7092404677718,-14.766904445574,42.770539858458));
#19944=CARTESIAN_POINT('Ctrl Pts',(-36.6935378630025,-14.7669045594521,
42.7378780623783));
#19945=CARTESIAN_POINT('Ctrl Pts',(-36.6791792700311,-14.7669045735796,
42.7045103513217));
#19946=CARTESIAN_POINT('Ctrl Pts',(-36.6661264061134,-14.7669045795915,
42.6704888195698));
#19947=CARTESIAN_POINT('Ctrl Pts',(-36.6582496141909,-14.7669045832193,
42.6499584188713));
#19948=CARTESIAN_POINT('Ctrl Pts',(-36.6508492987573,-14.7669045823054,
42.629189708122));
#19949=CARTESIAN_POINT('Ctrl Pts',(-36.6439262383654,-14.7669045823054,
42.6081948668641));
#19950=CARTESIAN_POINT('',(-20.3943608403659,-14.7669045823054,-6.67016278536651));
#19951=CARTESIAN_POINT('Origin',(-44.291473431638,16.4830954176946,-44.2925682080606));
#19952=CARTESIAN_POINT('Origin',(-44.291473431638,13.4386401876617,-44.2925682080606));
#19953=CARTESIAN_POINT('Origin',(-44.291473431638,16.1705954176946,-44.2925682080606));
#19954=CARTESIAN_POINT('Origin',(0.0835265683620477,16.4830954176946,0.0824317919394229));
#19955=CARTESIAN_POINT('',(-48.2416470424902,16.3915662868154,-22.5111558702776));
#19956=CARTESIAN_POINT('',(-48.2616069551277,11.5746245485739,-4.13831849464094));
#19957=CARTESIAN_POINT('Ctrl Pts',(-48.2416470424886,16.3915662868154,-22.5111558702765));
#19958=CARTESIAN_POINT('Ctrl Pts',(-48.2463095265271,15.1541680928392,-19.5795487103057));
#19959=CARTESIAN_POINT('Ctrl Pts',(-48.2506569957559,14.0894359483377,-16.5909382447155));
#19960=CARTESIAN_POINT('Ctrl Pts',(-48.2559385859013,12.8480220597894,-11.9905975010272));
#19961=CARTESIAN_POINT('Ctrl Pts',(-48.2574906537671,12.4934998941785,-10.4347915160951));
#19962=CARTESIAN_POINT('Ctrl Pts',(-48.2600106799664,11.9258476364963,-7.30351014927071));
#19963=CARTESIAN_POINT('Ctrl Pts',(-48.2609809492583,11.7120008366799,-5.72500374474883));
#19964=CARTESIAN_POINT('Ctrl Pts',(-48.2616069550931,11.5746245485739,-4.13831849503741));
#19965=CARTESIAN_POINT('',(-4.13722371775065,11.5746245485364,-48.2627017315536));
#19966=CARTESIAN_POINT('Origin',(0.0835265683620477,11.5746245485738,0.0824317919394229));
#19967=CARTESIAN_POINT('',(-22.5100610938543,16.3915662868156,-48.2427418189112));
#19968=CARTESIAN_POINT('Ctrl Pts',(-4.13722371861476,11.5746245485739,-48.2627017315157));
#19969=CARTESIAN_POINT('Ctrl Pts',(-5.72250617307994,11.7118793817134,-48.2620762791354));
#19970=CARTESIAN_POINT('Ctrl Pts',(-7.29569335888353,11.9249456441311,-48.2611095568614));
#19971=CARTESIAN_POINT('Ctrl Pts',(-10.419797403947,12.4906656417943,-48.2585979169746));
#19972=CARTESIAN_POINT('Ctrl Pts',(-11.9729836285199,12.843980457976,-48.2570508371642));
#19973=CARTESIAN_POINT('Ctrl Pts',(-16.5789073885739,14.0856585112706,-48.2517672875344));
#19974=CARTESIAN_POINT('Ctrl Pts',(-19.5792793614228,15.1545164964592,-48.247402990174));
#19975=CARTESIAN_POINT('Ctrl Pts',(-22.5100610938539,16.3915662868154,-48.2427418189112));
#19976=CARTESIAN_POINT('Origin',(0.0835265683620477,16.3915662868154,0.0824317919394229));
#19977=CARTESIAN_POINT('Origin',(0.083526568362047,-85.4775827009602,-48.3550682080606));
#19978=CARTESIAN_POINT('',(4.28505819640515,11.7955954176946,-48.3550682080606));
#19979=CARTESIAN_POINT('',(0.0835265683620996,11.6131136241746,-48.3550682080606));
#19980=CARTESIAN_POINT('Origin',(0.0819794847533267,84.3502669982689,-48.3550682080606));
#19981=CARTESIAN_POINT('',(21.5192635553992,16.1706033824536,-48.3550682079476));
#19982=CARTESIAN_POINT('Ctrl Pts',(4.28505819640516,11.7955954176946,-48.3550682080605));
#19983=CARTESIAN_POINT('Ctrl Pts',(5.50013823173107,11.9012754508552,-48.3550682080566));
#19984=CARTESIAN_POINT('Ctrl Pts',(6.70990241723394,12.0520583728992,-48.3550682079193));
#19985=CARTESIAN_POINT('Ctrl Pts',(7.91463518434723,12.2455340352926,-48.3550682079632));
#19986=CARTESIAN_POINT('Ctrl Pts',(8.17547622965408,12.2874241501776,-48.3550682079727));
#19987=CARTESIAN_POINT('Ctrl Pts',(8.43608138895782,12.3313158147402,-48.3550682079893));
#19988=CARTESIAN_POINT('Ctrl Pts',(8.69645351250441,12.3771848834522,-48.3550682080079));
#19989=CARTESIAN_POINT('Ctrl Pts',(8.7750191265218,12.3910255799857,-48.3550682080135));
#19990=CARTESIAN_POINT('Ctrl Pts',(8.85355914623864,12.4050450140608,-48.3550682080107));
#19991=CARTESIAN_POINT('Ctrl Pts',(8.93207474413674,12.4192427232394,-48.3550682079984));
#19992=CARTESIAN_POINT('Ctrl Pts',(9.48447684182607,12.5191317203639,-48.3550682079116));
#19993=CARTESIAN_POINT('Ctrl Pts',(10.0363845144415,12.6280707956085,-48.3550682070548));
#19994=CARTESIAN_POINT('Ctrl Pts',(10.5869585665338,12.7454889373936,-48.3550682017512));
#19995=CARTESIAN_POINT('Ctrl Pts',(11.1518287905254,12.8659559514106,-48.35506819631));
#19996=CARTESIAN_POINT('Ctrl Pts',(11.7152965319533,12.9953485173926,-48.3550681859822));
#19997=CARTESIAN_POINT('Ctrl Pts',(12.2764461842882,13.1331031832615,-48.355068184015));
#19998=CARTESIAN_POINT('Ctrl Pts',(12.5381803751669,13.1973553945227,-48.3550681830974));
#19999=CARTESIAN_POINT('Ctrl Pts',(12.7994100068431,13.2634275010368,-48.3550681842804));
#20000=CARTESIAN_POINT('Ctrl Pts',(13.0600402582532,13.3312657045531,-48.3550681878717));
#20001=CARTESIAN_POINT('Ctrl Pts',(13.2556797364647,13.3821877700729,-48.3550681905676));
#20002=CARTESIAN_POINT('Ctrl Pts',(13.4510063934693,13.434106757518,-48.3550681928176));
#20003=CARTESIAN_POINT('Ctrl Pts',(13.645959769717,13.4869947668889,-48.3550681947288));
#20004=CARTESIAN_POINT('Ctrl Pts',(14.4497762714823,13.7050584675342,-48.3550682026087));
#20005=CARTESIAN_POINT('Ctrl Pts',(15.2484412867238,13.9395350034004,-48.3550682050813));
#20006=CARTESIAN_POINT('Ctrl Pts',(16.0422501539207,14.189298282416,-48.3550682064483));
#20007=CARTESIAN_POINT('Ctrl Pts',(16.8503556614315,14.4435598429592,-48.3550682078398));
#20008=CARTESIAN_POINT('Ctrl Pts',(17.6534285697549,14.7136635664416,-48.3550682079255));
#20009=CARTESIAN_POINT('Ctrl Pts',(18.4518008809203,14.9983707526325,-48.3550682080074));
#20010=CARTESIAN_POINT('Ctrl Pts',(19.2740592777951,15.2915959449672,-48.3550682080917));
#20011=CARTESIAN_POINT('Ctrl Pts',(20.0913316502591,15.600311376789,-48.3550682080606));
#20012=CARTESIAN_POINT('Ctrl Pts',(20.9040014843348,15.9231126709103,-48.3550682080606));
#20013=CARTESIAN_POINT('Ctrl Pts',(21.1093767204212,16.0046899476952,-48.3550682080606));
#20014=CARTESIAN_POINT('Ctrl Pts',(21.3144581104562,16.0871665859146,-48.3550682080606));
#20015=CARTESIAN_POINT('Ctrl Pts',(21.5192520383888,16.1705194395555,-48.3550682080606));
#20016=CARTESIAN_POINT('',(-21.3522103060312,16.1706033612892,-48.3550682079475));
#20017=CARTESIAN_POINT('',(0.083526568362047,16.1705954176946,-48.3550682080606));
#20018=CARTESIAN_POINT('',(-4.11800505968095,11.7955954176946,-48.3550682080606));
#20019=CARTESIAN_POINT('Ctrl Pts',(-21.3521988196773,16.1705196413539,-48.3550682080606));
#20020=CARTESIAN_POINT('Ctrl Pts',(-20.5487763954986,15.8435202228695,-48.3550682080606));
#20021=CARTESIAN_POINT('Ctrl Pts',(-19.7409251344067,15.5300086687594,-48.3550682080737));
#20022=CARTESIAN_POINT('Ctrl Pts',(-18.9282733738634,15.231367963779,-48.3550682080473));
#20023=CARTESIAN_POINT('Ctrl Pts',(-18.1328568981362,14.939061038971,-48.3550682080215));
#20024=CARTESIAN_POINT('Ctrl Pts',(-17.3328413075813,14.6610010609439,-48.3550682080443));
#20025=CARTESIAN_POINT('Ctrl Pts',(-16.5278966912028,14.3984390234986,-48.3550682072886));
#20026=CARTESIAN_POINT('Ctrl Pts',(-15.7437545768866,14.1426624806255,-48.3550682065524));
#20027=CARTESIAN_POINT('Ctrl Pts',(-14.9549348814219,13.9015932988569,-48.3550682052102));
#20028=CARTESIAN_POINT('Ctrl Pts',(-14.1611512443295,13.6763418789407,-48.3550682001227));
#20029=CARTESIAN_POINT('Ctrl Pts',(-13.9342291332018,13.6119483523507,-48.3550681986684));
#20030=CARTESIAN_POINT('Ctrl Pts',(-13.7069014694831,13.5488472154603,-48.3550681968855));
#20031=CARTESIAN_POINT('Ctrl Pts',(-13.4791618560963,13.4870636734958,-48.3550681946374));
#20032=CARTESIAN_POINT('Ctrl Pts',(-13.284209997429,13.4341751304712,-48.355068192713));
#20033=CARTESIAN_POINT('Ctrl Pts',(-13.0888824669268,13.3822549873819,-48.3550681904474));
#20034=CARTESIAN_POINT('Ctrl Pts',(-12.8932400676278,13.3313312754885,-48.3550681877328));
#20035=CARTESIAN_POINT('Ctrl Pts',(-12.3335737655675,13.1856558716668,-48.3550681799675));
#20036=CARTESIAN_POINT('Ctrl Pts',(-11.7711216017144,13.0481153497989,-48.3550681851995));
#20037=CARTESIAN_POINT('Ctrl Pts',(-11.2068238023173,12.9192577967038,-48.3550681923975));
#20038=CARTESIAN_POINT('Ctrl Pts',(-10.6541153068945,12.7930466642643,-48.3550681994477));
#20039=CARTESIAN_POINT('Ctrl Pts',(-10.0996349288977,12.6751650327118,-48.3550682055201));
#20040=CARTESIAN_POINT('Ctrl Pts',(-9.54424878778532,12.5661734818932,-48.3550682070987));
#20041=CARTESIAN_POINT('Ctrl Pts',(-9.28473868838682,12.5152460170309,-48.3550682078364));
#20042=CARTESIAN_POINT('Ctrl Pts',(-9.02503069905943,12.4662602454808,-48.355068207957));
#20043=CARTESIAN_POINT('Ctrl Pts',(-8.76521301459484,12.4192773203262,-48.3550682079981));
#20044=CARTESIAN_POINT('Ctrl Pts',(-8.68668667654382,12.405077374426,-48.3550682080105));
#20045=CARTESIAN_POINT('Ctrl Pts',(-8.6081361458596,12.3910557938695,-48.3550682080133));
#20046=CARTESIAN_POINT('Ctrl Pts',(-8.52956025973485,12.3772130393319,-48.3550682080077));
#20047=CARTESIAN_POINT('Ctrl Pts',(-7.3298348698903,12.1658567963019,-48.3550682079214));
#20048=CARTESIAN_POINT('Ctrl Pts',(-6.12517728947009,11.9964818480142,-48.3550682079949));
#20049=CARTESIAN_POINT('Ctrl Pts',(-4.91530765780725,11.8714667031496,-48.3550682080425));
#20050=CARTESIAN_POINT('Ctrl Pts',(-4.64979216840663,11.8440311377774,-48.355068208053));
#20051=CARTESIAN_POINT('Ctrl Pts',(-4.38402563457531,11.8187322172129,-48.3550682080596));
#20052=CARTESIAN_POINT('Ctrl Pts',(-4.11800505968097,11.7955954176945,-48.3550682080605));
#20053=CARTESIAN_POINT('Origin',(0.0850736592996893,84.3502670004067,-48.3550682139743));
#20054=CARTESIAN_POINT('Origin',(-48.3539734316379,-85.4775827009602,-44.2925682080605));
#20055=CARTESIAN_POINT('',(-48.3539734316379,-6.32940458230554,4.28396341998237));
#20056=CARTESIAN_POINT('',(-48.3539734316379,-6.14692278878557,0.0824317919393188));
#20057=CARTESIAN_POINT('Origin',(-48.3539734376932,-78.8840761710573,0.0808847054354922));
#20058=CARTESIAN_POINT('',(-48.3539734316292,-14.4544067125518,29.5557245537287));
#20059=CARTESIAN_POINT('Ctrl Pts',(-48.3539734316348,-6.32940458230555,
4.28396341998237));
#20060=CARTESIAN_POINT('Ctrl Pts',(-48.3539734314083,-6.60009088520904,
7.39624028683883));
#20061=CARTESIAN_POINT('Ctrl Pts',(-48.3539734245018,-7.165487581754,10.4492205117651));
#20062=CARTESIAN_POINT('Ctrl Pts',(-48.3539734271436,-7.96970388346465,
13.454151014626));
#20063=CARTESIAN_POINT('Ctrl Pts',(-48.3539734282648,-8.31099932795918,
14.729391381512));
#20064=CARTESIAN_POINT('Ctrl Pts',(-48.3539734303379,-8.695305697332,15.9959779893149));
#20065=CARTESIAN_POINT('Ctrl Pts',(-48.3539734312518,-9.11834864237836,
17.2547710529606));
#20066=CARTESIAN_POINT('Ctrl Pts',(-48.3539734313703,-9.17316448001786,
17.4178793071142));
#20067=CARTESIAN_POINT('Ctrl Pts',(-48.353973431397,-9.22862227451118,17.5808367859632));
#20068=CARTESIAN_POINT('Ctrl Pts',(-48.3539734313916,-9.28471651645581,
17.74365610972));
#20069=CARTESIAN_POINT('Ctrl Pts',(-48.3539734313723,-9.48472234839191,
18.3241936689119));
#20070=CARTESIAN_POINT('Ctrl Pts',(-48.3539734305475,-9.69311870415955,
18.9037446387506));
#20071=CARTESIAN_POINT('Ctrl Pts',(-48.353973430177,-9.90895820813048,19.4810918986109));
#20072=CARTESIAN_POINT('Ctrl Pts',(-48.3539734299785,-10.0245908848806,
19.7903967656244));
#20073=CARTESIAN_POINT('Ctrl Pts',(-48.3539734301286,-10.1423607380477,
20.0990689006501));
#20074=CARTESIAN_POINT('Ctrl Pts',(-48.3539734306861,-10.2621272193483,
20.4069177749615));
#20075=CARTESIAN_POINT('Ctrl Pts',(-48.353973431074,-10.3454600297986,20.6211172038148));
#20076=CARTESIAN_POINT('Ctrl Pts',(-48.3539734312712,-10.4297627624244,
20.8349374125696));
#20077=CARTESIAN_POINT('Ctrl Pts',(-48.3539734313944,-10.5149781806565,
21.0482886973521));
#20078=CARTESIAN_POINT('Ctrl Pts',(-48.3539734318711,-10.8449565878889,
21.8744457308332));
#20079=CARTESIAN_POINT('Ctrl Pts',(-48.3539734316591,-11.188740579391,22.6942362972106));
#20080=CARTESIAN_POINT('Ctrl Pts',(-48.3539734316028,-11.5450903892488,
23.5084157089998));
#20081=CARTESIAN_POINT('Ctrl Pts',(-48.353973431585,-11.6579509129727,23.7662766991778));
#20082=CARTESIAN_POINT('Ctrl Pts',(-48.3539734315666,-11.7720687209441,
24.0235665829017));
#20083=CARTESIAN_POINT('Ctrl Pts',(-48.3539734315544,-11.8874012527356,
24.280305717357));
#20084=CARTESIAN_POINT('Ctrl Pts',(-48.353973431512,-12.2879313738287,25.1719167399829));
#20085=CARTESIAN_POINT('Ctrl Pts',(-48.3539734315605,-12.7030439005446,
26.0569236215327));
#20086=CARTESIAN_POINT('Ctrl Pts',(-48.3539734315972,-13.1313454185141,
26.9359487176993));
#20087=CARTESIAN_POINT('Ctrl Pts',(-48.3539734316338,-13.5596469364837,
27.8149738138659));
#20088=CARTESIAN_POINT('Ctrl Pts',(-48.3539734316379,-14.001137100463,28.6880173360691));
#20089=CARTESIAN_POINT('Ctrl Pts',(-48.3539734316379,-14.4543739218735,
29.5557312928386));
#20090=CARTESIAN_POINT('',(-48.3539734316379,-14.4544045823054,-29.3908631559322));
#20091=CARTESIAN_POINT('',(-48.3539734316379,-14.4544045823054,-30.3185344755988));
#20092=CARTESIAN_POINT('',(-48.3539734316379,-6.32940458230556,-4.11909983610373));
#20093=CARTESIAN_POINT('Ctrl Pts',(-48.3539734316379,-14.4543736123986,
-29.3908678705539));
#20094=CARTESIAN_POINT('Ctrl Pts',(-48.3539734316379,-14.0009603589249,
-28.5228172256933));
#20095=CARTESIAN_POINT('Ctrl Pts',(-48.3539734316337,-13.5592886344727,
-27.6494060064744));
#20096=CARTESIAN_POINT('Ctrl Pts',(-48.3539734315961,-13.1308037218344,
-26.7699764159717));
#20097=CARTESIAN_POINT('Ctrl Pts',(-48.3539734315586,-12.7023188091961,
-25.890546825469));
#20098=CARTESIAN_POINT('Ctrl Pts',(-48.3539734315088,-12.2870210611745,
-25.0050986454736));
#20099=CARTESIAN_POINT('Ctrl Pts',(-48.3539734315522,-11.8863062114336,
-24.1130046264528));
#20100=CARTESIAN_POINT('Ctrl Pts',(-48.3539734315648,-11.7707122689893,
-23.8556628664549));
#20101=CARTESIAN_POINT('Ctrl Pts',(-48.3539734315836,-11.6563375248576,
-23.5977648578349));
#20102=CARTESIAN_POINT('Ctrl Pts',(-48.3539734316019,-11.5432249100059,
-23.3392899164854));
#20103=CARTESIAN_POINT('Ctrl Pts',(-48.3539734316532,-11.2263851142924,
-22.6152756434389));
#20104=CARTESIAN_POINT('Ctrl Pts',(-48.3539734317118,-10.9195690676833,
-21.8870351496141));
#20105=CARTESIAN_POINT('Ctrl Pts',(-48.3539734315538,-10.6234156307627,
-21.1534577234119));
#20106=CARTESIAN_POINT('Ctrl Pts',(-48.3539734315341,-10.5864935786647,
-21.0620011317553));
#20107=CARTESIAN_POINT('Ctrl Pts',(-48.3539734315083,-10.5497373137513,
-20.9704615520097));
#20108=CARTESIAN_POINT('Ctrl Pts',(-48.3539734314726,-10.5131481250882,
-20.8788368000147));
#20109=CARTESIAN_POINT('Ctrl Pts',(-48.353973431389,-10.4276256561533,-20.6646758608825));
#20110=CARTESIAN_POINT('Ctrl Pts',(-48.3539734312548,-10.3430386875929,
-20.4500850053422));
#20111=CARTESIAN_POINT('Ctrl Pts',(-48.3539734309901,-10.2594333452065,
-20.235123917639));
#20112=CARTESIAN_POINT('Ctrl Pts',(-48.3539734303323,-10.051669996851,-19.7009351436613));
#20113=CARTESIAN_POINT('Ctrl Pts',(-48.3539734307198,-9.85012639371284,
-19.1648181410921));
#20114=CARTESIAN_POINT('Ctrl Pts',(-48.3539734310814,-9.65537647176604,
-18.627378781688));
#20115=CARTESIAN_POINT('Ctrl Pts',(-48.3539734313171,-9.52849547986369,
-18.2772331265478));
#20116=CARTESIAN_POINT('Ctrl Pts',(-48.3539734314598,-9.40449887251127,
-17.9265254096188));
#20117=CARTESIAN_POINT('Ctrl Pts',(-48.3539734314675,-9.28355639505876,
-17.5754184692672));
#20118=CARTESIAN_POINT('Ctrl Pts',(-48.3539734314711,-9.22712679184453,
-17.4115982321832));
#20119=CARTESIAN_POINT('Ctrl Pts',(-48.3539734314525,-9.17133865071588,
-17.247630070549));
#20120=CARTESIAN_POINT('Ctrl Pts',(-48.3539734313696,-9.11619658428807,
-17.0834969853208));
#20121=CARTESIAN_POINT('Ctrl Pts',(-48.3539734305581,-8.57607118782138,
-15.4757870557661));
#20122=CARTESIAN_POINT('Ctrl Pts',(-48.353973428403,-8.09914441522936,-13.8554310180361));
#20123=CARTESIAN_POINT('Ctrl Pts',(-48.3539734276855,-7.69433779295044,
-12.2206426330261));
#20124=CARTESIAN_POINT('Ctrl Pts',(-48.3539734269937,-7.30405740045158,
-10.6445175959344));
#20125=CARTESIAN_POINT('Ctrl Pts',(-48.3539734277293,-6.98081414568337,
-9.05497754756053));
#20126=CARTESIAN_POINT('Ctrl Pts',(-48.3539734292173,-6.73255660928855,
-7.45043168080743));
#20127=CARTESIAN_POINT('Ctrl Pts',(-48.3539734302404,-6.56187116055321,
-6.3472521549798));
#20128=CARTESIAN_POINT('Ctrl Pts',(-48.3539734315641,-6.42663073464616,
-5.23697946849498));
#20129=CARTESIAN_POINT('Ctrl Pts',(-48.3539734316352,-6.32940458230556,
-4.11909983610374));
#20130=CARTESIAN_POINT('Origin',(-48.3539734376649,-78.8840761544994,0.0839788705204157));
#20131=CARTESIAN_POINT('Origin',(-39.6912298733813,16.4855954176946,-41.0181498645286));
#20132=CARTESIAN_POINT('',(-37.8722959448873,-8.24885981233827,-39.1992159360346));
#20133=CARTESIAN_POINT('Ctrl Pts',(-34.5978496132723,-3.61941807409669,
-35.9247696044197));
#20134=CARTESIAN_POINT('Ctrl Pts',(-35.144360826703,-4.3920600802535,-36.4712808178504));
#20135=CARTESIAN_POINT('Ctrl Pts',(-35.6908680880204,-5.16470767732064,
-37.0177880791678));
#20136=CARTESIAN_POINT('Ctrl Pts',(-36.7823498735465,-6.70785538323104,
-38.1092698646939));
#20137=CARTESIAN_POINT('Ctrl Pts',(-37.3273244157758,-7.4783554666459,-38.6542444069232));
#20138=CARTESIAN_POINT('Ctrl Pts',(-37.8722959448873,-8.24885981233827,
-39.1992159360346));
#20139=CARTESIAN_POINT('',(-39.0283172660189,-8.24885981233827,-40.3552372571663));
#20140=CARTESIAN_POINT('',(-35.219899890096,12.8136401876617,-36.5468198812434));
#20141=CARTESIAN_POINT('',(-35.1331064857663,12.8136401876617,-36.4600264769137));
#20142=CARTESIAN_POINT('',(-35.219899890096,12.8136401876617,-36.5468198812434));
#20143=CARTESIAN_POINT('Origin',(-41.017055088106,16.4855954176946,-39.6923246498039));
#20144=CARTESIAN_POINT('',(-39.198121159612,-8.24885981233827,-37.8733907213099));
#20145=CARTESIAN_POINT('',(-39.1110035352202,-8.24885981233827,-37.7862730969181));
#20146=CARTESIAN_POINT('',(-35.9236748279971,-3.61941807409669,-34.5989443896949));
#20147=CARTESIAN_POINT('Ctrl Pts',(-39.198121159612,-8.24885981233827,-37.8733907213099));
#20148=CARTESIAN_POINT('Ctrl Pts',(-38.6531496305005,-7.47835546664588,
-37.3284191921984));
#20149=CARTESIAN_POINT('Ctrl Pts',(-38.1081750882713,-6.70785538323099,
-36.7834446499691));
#20150=CARTESIAN_POINT('Ctrl Pts',(-37.0166933027451,-5.1647076773206,-35.6919628644429));
#20151=CARTESIAN_POINT('Ctrl Pts',(-36.4701860414278,-4.39206008025347,
-35.1454556031256));
#20152=CARTESIAN_POINT('Ctrl Pts',(-35.9236748279971,-3.61941807409669,
-34.5989443896949));
#20153=CARTESIAN_POINT('',(-35.9236748279974,11.9341984494207,-34.5989443896953));
#20154=CARTESIAN_POINT('',(-35.9236748279971,12.0636401876617,-34.5989443896949));
#20155=CARTESIAN_POINT('',(-36.5457251048207,12.8136401876617,-35.2209946665186));
#20156=CARTESIAN_POINT('',(-35.9236748279971,11.9341984494202,-34.5989443896949));
#20157=CARTESIAN_POINT('',(-40.3541424807436,12.8136401876617,-39.0294120424415));
#20158=CARTESIAN_POINT('Origin',(0.0835265683620477,-11.0169045823054,0.0824317919394229));
#20159=CARTESIAN_POINT('',(-9.89989012376418,-11.3294045823054,-19.3815610191817));
#20160=CARTESIAN_POINT('',(-9.89989012376418,-14.4544045823054,-19.3815610191817));
#20161=CARTESIAN_POINT('',(-9.89989012376418,-11.0169045823054,-19.3815610191817));
#20162=CARTESIAN_POINT('',(-20.6911418173041,-14.4544045823054,-6.76802647489247));
#20163=CARTESIAN_POINT('Origin',(0.0835265683620477,-14.4544045823054,0.0824317919394229));
#20164=CARTESIAN_POINT('',(-20.6911418173041,-11.3294045823054,-6.76802647489247));
#20165=CARTESIAN_POINT('',(-20.6911418173041,-11.0169045823054,-6.76802647489247));
#20166=CARTESIAN_POINT('Origin',(0.0835265683620477,-11.3294045823054,0.0824317919394229));
#20167=CARTESIAN_POINT('Origin',(0.0835265683620477,-13.2044045823054,0.0824317919394229));
#20168=CARTESIAN_POINT('',(-34.1929414312581,-13.2044045823054,-34.5829146143929));
#20169=CARTESIAN_POINT('',(-41.2766849510695,-13.2044045823054,-36.9187829158523));
#20170=CARTESIAN_POINT('',(-41.5387861275671,-13.2044045823054,-37.0052109222086));
#20171=CARTESIAN_POINT('',(-40.1126065460396,-13.2044045823054,-38.1801853354021));
#20172=CARTESIAN_POINT('Origin',(0.0835265683620477,-13.2044045823054,0.0824317919394229));
#20173=CARTESIAN_POINT('',(-32.9108164063353,-13.2044045823054,-35.8053910964449));
#20174=CARTESIAN_POINT('',(7.52116697235096,-13.2044045823054,-22.4729224553552));
#20175=CARTESIAN_POINT('Origin',(0.0835265683620477,-13.2044045823054,0.0824317919394229));
#20176=CARTESIAN_POINT('Origin',(7.61903066187713,16.4855954176946,-22.7697034322933));
#20177=CARTESIAN_POINT('',(-32.8129527168091,-12.8919045823054,-36.102172073383));
#20178=CARTESIAN_POINT('',(-39.0675209577957,-12.8919045823054,-38.1646193729747));
#20179=CARTESIAN_POINT('',(7.61903066187713,-12.8919045823054,-22.7697034322933));
#20180=CARTESIAN_POINT('',(-32.8129496113305,-7.07886051013308,-36.1021710493883));
#20181=CARTESIAN_POINT('Ctrl Pts',(-39.0675209577957,-12.8919045823054,
-38.1646193729747));
#20182=CARTESIAN_POINT('Ctrl Pts',(-37.4159861250462,-11.333902336486,-37.6200248582543));
#20183=CARTESIAN_POINT('Ctrl Pts',(-35.7569364419389,-9.78474033506735,
-37.0729523175167));
#20184=CARTESIAN_POINT('Ctrl Pts',(-34.0875946907817,-8.24794400051366,
-36.5224859617085));
#20185=CARTESIAN_POINT('Ctrl Pts',(-33.6633986356396,-7.85742903123153,
-36.3826070804306));
#20186=CARTESIAN_POINT('Ctrl Pts',(-33.2385378437358,-7.46771271973443,
-36.2425090018419));
#20187=CARTESIAN_POINT('Ctrl Pts',(-32.8129663798493,-7.07885337126046,
-36.102176578778));
#20188=CARTESIAN_POINT('',(-32.8129527168091,16.4855954176946,-36.102172073383));
#20189=CARTESIAN_POINT('Origin',(0.0835265683620477,-13.2044045823054,0.0824317919394229));
#20190=CARTESIAN_POINT('',(-39.8705894675228,-13.2044045823054,-27.8501855539351));
#20191=CARTESIAN_POINT('',(-46.5229781270741,-13.2044045823054,-30.0438143542121));
#20192=CARTESIAN_POINT('',(-46.726369315508,-13.2044045823054,-30.1108827098817));
#20193=CARTESIAN_POINT('',(-45.6231018412815,-13.2044045823054,-31.3923375671359));
#20194=CARTESIAN_POINT('Origin',(0.0835265683620477,-13.2044045823054,0.0824317919394229));
#20195=CARTESIAN_POINT('',(-38.9085015017574,-13.2044045823054,-29.1781944313494));
#20196=CARTESIAN_POINT('',(4.96196078618764,-13.2044045823054,-14.7118854886011));
#20197=CARTESIAN_POINT('Origin',(0.0835265683620477,-13.2044045823054,0.0824317919394229));
#20198=CARTESIAN_POINT('Origin',(4.37477864903062,16.4855954176946,-12.9311996269726));
#20199=CARTESIAN_POINT('',(-39.968453157049,-12.8919045823054,-27.553404576997));
#20200=CARTESIAN_POINT('',(-39.9684532734914,-6.59535001054288,-27.5534046153939));
#20201=CARTESIAN_POINT('',(-39.968453157049,-6.01690458230549,-27.553404576997));
#20202=CARTESIAN_POINT('',(-46.1602402810308,-12.8919045823054,-29.5951497689063));
#20203=CARTESIAN_POINT('Ctrl Pts',(-39.968453721219,-6.59534981969064,-27.5534047630323));
#20204=CARTESIAN_POINT('Ctrl Pts',(-42.0370533398943,-8.68909917212592,
-28.2355266191048));
#20205=CARTESIAN_POINT('Ctrl Pts',(-44.1004290564877,-10.788569829982,-28.9159258906075));
#20206=CARTESIAN_POINT('Ctrl Pts',(-46.1602402810309,-12.8919045823054,
-29.5951497689063));
#20207=CARTESIAN_POINT('',(-39.74712214338,-12.8919045823054,-27.4804205541405));
#20208=CARTESIAN_POINT('Origin',(0.0835265683620477,15.5455954176946,0.0824317919394229));
#20209=CARTESIAN_POINT('',(-28.9637578711591,16.1705954176946,-46.6214788225857));
#20210=CARTESIAN_POINT('Origin',(0.0835265683620477,16.1705954176946,0.0824317919394229));
#20211=CARTESIAN_POINT('',(-28.9637578711591,15.8580954176946,-46.6214788225857));
#20212=CARTESIAN_POINT('',(-28.9637578711591,15.5455954176946,-46.6214788225857));
#20213=CARTESIAN_POINT('Origin',(0.0835265683620477,15.8580954176946,0.0824317919394229));
#20214=CARTESIAN_POINT('Origin',(-48.3539734316379,15.5455954176946,-42.6687705759647));
#20215=CARTESIAN_POINT('',(-48.3539734316379,15.8580954176946,-39.9964034940395));
#20216=CARTESIAN_POINT('',(-48.3539734316379,16.1705954176946,-39.9964034940395));
#20217=CARTESIAN_POINT('',(-48.3539734316379,16.4830954176946,-39.9964034940395));
#20218=CARTESIAN_POINT('',(-48.3539734316379,16.1705954176946,-29.4599768141645));
#20219=CARTESIAN_POINT('',(-48.3539734316379,15.8580954176946,-42.6687705759647));
#20220=CARTESIAN_POINT('Origin',(-25.9704288655064,15.5455954176946,-48.3550682080606));
#20221=CARTESIAN_POINT('',(-29.4588820377419,15.8580954176946,-48.3550682080606));
#20222=CARTESIAN_POINT('',(-29.4588820377419,16.1705954176946,-48.3550682080606));
#20223=CARTESIAN_POINT('',(-29.4588820377419,16.4830954176946,-48.3550682080606));
#20224=CARTESIAN_POINT('',(-39.9953087176169,16.1705954176946,-48.3550682080606));
#20225=CARTESIAN_POINT('',(-39.9953087176169,16.1705954176946,-48.3550682080606));
#20226=CARTESIAN_POINT('',(-39.9953087176169,15.8580954176946,-48.3550682080606));
#20227=CARTESIAN_POINT('',(-39.9953087176169,15.5455954176946,-48.3550682080606));
#20228=CARTESIAN_POINT('',(-25.9704288655064,15.8580954176946,-48.3550682080606));
#20229=CARTESIAN_POINT('Origin',(0.0835265683620477,15.5455954176946,0.0824317919394229));
#20230=CARTESIAN_POINT('',(-48.0414734316379,15.5455954176946,-39.9964034940395));
#20231=CARTESIAN_POINT('Origin',(-47.4164734316379,15.5455954176946,-39.9964034940395));
#20232=CARTESIAN_POINT('',(-48.0414734316379,15.5455954176946,0.0824317919394229));
#20233=CARTESIAN_POINT('',(-29.1287992600201,15.5455954176946,-46.8868419510773));
#20234=CARTESIAN_POINT('Origin',(0.0835265683620477,15.5455954176946,0.0824317919394229));
#20235=CARTESIAN_POINT('',(-29.4588820377419,15.5455954176946,-48.0425682080606));
#20236=CARTESIAN_POINT('Origin',(-29.4588820377419,15.5455954176946,-47.4175682080606));
#20237=CARTESIAN_POINT('',(-39.9953087176169,15.5455954176946,-48.0425682080606));
#20238=CARTESIAN_POINT('',(0.0835265683620977,15.5455954176946,-48.0425682080605));
#20239=CARTESIAN_POINT('Origin',(-39.9953087176169,15.5455954176946,-47.4175682080606));
#20240=CARTESIAN_POINT('Origin',(-29.4588820377419,15.5455954176946,-47.4175682080606));
#20241=CARTESIAN_POINT('Origin',(-29.4588820377419,15.8580954176946,-47.4175682080606));
#20242=CARTESIAN_POINT('Origin',(-29.4588820377419,16.1705954176946,-47.4175682080606));
#20243=CARTESIAN_POINT('Origin',(-47.4164734316379,15.5455954176946,-39.9964034940395));
#20244=CARTESIAN_POINT('Origin',(-47.4164734316379,15.8580954176946,-39.9964034940395));
#20245=CARTESIAN_POINT('Origin',(-47.4164734316379,16.1705954176946,-39.9964034940395));
#20246=CARTESIAN_POINT('Origin',(-39.9953087176169,15.5455954176946,-47.4175682080606));
#20247=CARTESIAN_POINT('Origin',(-39.9953087176169,15.8580954176946,-47.4175682080606));
#20248=CARTESIAN_POINT('Origin',(-39.9953087176169,16.1705954176946,-47.4175682080606));
#20249=CARTESIAN_POINT('Origin',(0.0835265683620477,-6.01690458230549,0.0824317919394229));
#20250=CARTESIAN_POINT('',(31.6836214013763,-13.2959337131846,-45.8061901631445));
#20251=CARTESIAN_POINT('',(30.3297286714006,-13.2959337131846,-46.7096495545262));
#20252=CARTESIAN_POINT('Origin',(0.0835265683620477,-13.2959337131846,0.0824317919394229));
#20253=CARTESIAN_POINT('',(29.5826474545624,-12.6709337131846,-46.4458225157374));
#20254=CARTESIAN_POINT('Ctrl Pts',(30.3297286714006,-13.2959337131846,-46.7096495545262));
#20255=CARTESIAN_POINT('Ctrl Pts',(30.2953116335171,-13.2959337131846,-46.7318965812379));
#20256=CARTESIAN_POINT('Ctrl Pts',(30.2590829799862,-13.2919430659199,-46.7505039986476));
#20257=CARTESIAN_POINT('Ctrl Pts',(30.2221538011279,-13.2842290832321,-46.7650885650838));
#20258=CARTESIAN_POINT('Ctrl Pts',(30.1851131667048,-13.2764918190547,-46.779717149046));
#20259=CARTESIAN_POINT('Ctrl Pts',(30.1473660521867,-13.2650083398801,-46.7902992078703));
#20260=CARTESIAN_POINT('Ctrl Pts',(30.1100232324367,-13.2500137812862,-46.7964131006815));
#20261=CARTESIAN_POINT('Ctrl Pts',(30.0963576295144,-13.2445265233579,-46.7986504794341));
#20262=CARTESIAN_POINT('Ctrl Pts',(30.0827461978655,-13.2385687578801,-46.800289099107));
#20263=CARTESIAN_POINT('Ctrl Pts',(30.0692437277915,-13.232151003965,-46.8013068668765));
#20264=CARTESIAN_POINT('Ctrl Pts',(30.06896789394,-13.2320198995248,-46.801327658243));
#20265=CARTESIAN_POINT('Ctrl Pts',(30.0686921064576,-13.2318886036913,-46.801348190617));
#20266=CARTESIAN_POINT('Ctrl Pts',(30.0684163658334,-13.2317571165657,-46.80136846381));
#20267=CARTESIAN_POINT('Ctrl Pts',(30.0213645219584,-13.2093204091551,-46.8048278420269));
#20268=CARTESIAN_POINT('Ctrl Pts',(29.9767272365876,-13.1821368365904,-46.8010574025015));
#20269=CARTESIAN_POINT('Ctrl Pts',(29.9353668651223,-13.1520894283177,-46.7917741093876));
#20270=CARTESIAN_POINT('Ctrl Pts',(29.9003561104518,-13.126654878234,-46.7839159812753));
#20271=CARTESIAN_POINT('Ctrl Pts',(29.8676937058866,-13.0991694705196,-46.7721089114476));
#20272=CARTESIAN_POINT('Ctrl Pts',(29.8379008490097,-13.0707895719798,-46.7574125642514));
#20273=CARTESIAN_POINT('Ctrl Pts',(29.8376173879301,-13.0705195543472,-46.7572727373641));
#20274=CARTESIAN_POINT('Ctrl Pts',(29.8373341809497,-13.0702494422352,-46.7571326365248));
#20275=CARTESIAN_POINT('Ctrl Pts',(29.8370512286687,-13.0699792368,-46.7569922627404));
#20276=CARTESIAN_POINT('Ctrl Pts',(29.8166813000282,-13.0505269623214,-46.7468866577897));
#20277=CARTESIAN_POINT('Ctrl Pts',(29.7974702652244,-13.0305367697043,-46.7354061965312));
#20278=CARTESIAN_POINT('Ctrl Pts',(29.779419955612,-13.0101903794891,-46.722765565803));
#20279=CARTESIAN_POINT('Ctrl Pts',(29.7688872570839,-12.9983178743149,-46.7153895176619));
#20280=CARTESIAN_POINT('Ctrl Pts',(29.758748871208,-12.9863240855331,-46.7076190123881));
#20281=CARTESIAN_POINT('Ctrl Pts',(29.748998012555,-12.9742444051773,-46.6995004081416));
#20282=CARTESIAN_POINT('Ctrl Pts',(29.7356513039303,-12.9577100691025,-46.6883878847044));
#20283=CARTESIAN_POINT('Ctrl Pts',(29.7230341631078,-12.9410147689399,-46.6766208987538));
#20284=CARTESIAN_POINT('Ctrl Pts',(29.7111382215491,-12.9242496162066,-46.6643130148113));
#20285=CARTESIAN_POINT('Ctrl Pts',(29.7051902507697,-12.9158670398399,-46.6581590728401));
#20286=CARTESIAN_POINT('Ctrl Pts',(29.6994225797523,-12.9074670004228,-46.6518699062888));
#20287=CARTESIAN_POINT('Ctrl Pts',(29.6938341619597,-12.8990608878296,-46.6454597098703));
#20288=CARTESIAN_POINT('Ctrl Pts',(29.6882457441671,-12.8906547752363,-46.6390495134518));
#20289=CARTESIAN_POINT('Ctrl Pts',(29.6828365795893,-12.8822425894822,-46.6325182871528));
#20290=CARTESIAN_POINT('Ctrl Pts',(29.6776056213999,-12.8738357211132,-46.6258802250576));
#20291=CARTESIAN_POINT('Ctrl Pts',(29.661151233601,-12.8473912596384,-46.604999681954));
#20292=CARTESIAN_POINT('Ctrl Pts',(29.6462987841921,-12.820747274008,-46.5828657680258));
#20293=CARTESIAN_POINT('Ctrl Pts',(29.6330144113446,-12.7940681980236,-46.5596959484487));
#20294=CARTESIAN_POINT('Ctrl Pts',(29.6294060259108,-12.7868214585446,-46.5534024154062));
#20295=CARTESIAN_POINT('Ctrl Pts',(29.6259136021541,-12.7795722581719,-46.5470324354036));
#20296=CARTESIAN_POINT('Ctrl Pts',(29.6225370413182,-12.7723242153339,-46.5405903840077));
#20297=CARTESIAN_POINT('Ctrl Pts',(29.6102672896986,-12.7459862668495,-46.5171812483842));
#20298=CARTESIAN_POINT('Ctrl Pts',(29.5995238745078,-12.7196622748057,-46.4928211348268));
#20299=CARTESIAN_POINT('Ctrl Pts',(29.5902746512498,-12.693508739059,-46.4677171585527));
#20300=CARTESIAN_POINT('Ctrl Pts',(29.5876078409674,-12.6859679417289,-46.4604789786333));
#20301=CARTESIAN_POINT('Ctrl Pts',(29.5850654985989,-12.6784415052658,-46.4531790258387));
#20302=CARTESIAN_POINT('Ctrl Pts',(29.5826474545624,-12.6709337131846,-46.4458225157374));
#20303=CARTESIAN_POINT('',(27.4605785366061,-6.10843371318477,-39.9870540284925));
#20304=CARTESIAN_POINT('Origin',(79.5093886191839,-177.510309510992,-197.332122666226));
#20305=CARTESIAN_POINT('',(4.30427685474491,-6.1084337131847,-48.2627017315676));
#20306=CARTESIAN_POINT('Origin',(0.0835265683620477,-6.10843371318469,0.0824317919394229));
#20307=CARTESIAN_POINT('',(30.5121796307595,-14.6753754514266,-48.2295435588552));
#20308=CARTESIAN_POINT('Ctrl Pts',(4.30427685533897,-6.10843371318471,-48.2627017315157));
#20309=CARTESIAN_POINT('Ctrl Pts',(8.94175590178151,-6.50994980321315,-48.2608720750402));
#20310=CARTESIAN_POINT('Ctrl Pts',(13.4240603542055,-7.55645913600449,-48.2561124331622));
#20311=CARTESIAN_POINT('Ctrl Pts',(19.9841318245208,-9.80534906153842,-48.2470092000062));
#20312=CARTESIAN_POINT('Ctrl Pts',(22.1452414843856,-10.6692546575742,-48.2436494975834));
#20313=CARTESIAN_POINT('Ctrl Pts',(26.3834535137794,-12.5596572871779,-48.2367077593843));
#20314=CARTESIAN_POINT('Ctrl Pts',(28.4629814284201,-13.58630787804,-48.2331238453003));
#20315=CARTESIAN_POINT('Ctrl Pts',(30.5121796307589,-14.6753754514262,-48.2295435588551));
#20316=CARTESIAN_POINT('',(32.131950172941,-14.6753754514262,-47.17059386726));
#20317=CARTESIAN_POINT('Origin',(0.0835265683620477,-14.6753754514262,0.0824317919394229));
#20318=CARTESIAN_POINT('Origin',(-321.603193845972,-1402.95413117761,1241.62885743152));
#20319=CARTESIAN_POINT('Origin',(15.1746248258407,-11.0169045823054,5.05872969929124));
#20320=CARTESIAN_POINT('',(20.1223573965802,-11.3294045823054,-9.94574144911951));
#20321=CARTESIAN_POINT('',(20.1223573965802,-11.0169045823054,-9.94574144911951));
#20322=CARTESIAN_POINT('',(29.4342239561067,-11.3294045823054,-38.184865357424));
#20323=CARTESIAN_POINT('',(15.1746248258407,-11.3294045823054,5.05872969929124));
#20324=CARTESIAN_POINT('',(29.4342239561067,-12.8919045823054,-38.184865357424));
#20325=CARTESIAN_POINT('',(29.4342239561067,-11.0169045823054,-38.184865357424));
#20326=CARTESIAN_POINT('',(29.6409337685891,-13.5169045823054,-38.8117325886538));
#20327=CARTESIAN_POINT('Ctrl Pts',(29.6409337685891,-13.5169045823054,-38.8117325886538));
#20328=CARTESIAN_POINT('Ctrl Pts',(29.6292942393977,-13.516904574972,-38.7764346057018));
#20329=CARTESIAN_POINT('Ctrl Pts',(29.617680555433,-13.5137764691088,-38.7412150008653));
#20330=CARTESIAN_POINT('Ctrl Pts',(29.6062374009932,-13.5077394335824,-38.7065125430914));
#20331=CARTESIAN_POINT('Ctrl Pts',(29.5939633721145,-13.5012640557673,-38.6692903792972));
#20332=CARTESIAN_POINT('Ctrl Pts',(29.5818851650686,-13.4914421681939,-38.6326620639058));
#20333=CARTESIAN_POINT('Ctrl Pts',(29.5701745905273,-13.4784883891808,-38.5971486291694));
#20334=CARTESIAN_POINT('Ctrl Pts',(29.5582820089413,-13.4653332811016,-38.5610832407026));
#20335=CARTESIAN_POINT('Ctrl Pts',(29.5467680680181,-13.4489478321172,-38.5261661161798));
#20336=CARTESIAN_POINT('Ctrl Pts',(29.5358129510534,-13.4295031815268,-38.4929436786193));
#20337=CARTESIAN_POINT('Ctrl Pts',(29.5252137549884,-13.4106902683751,-38.4608006051502));
#20338=CARTESIAN_POINT('Ctrl Pts',(29.5151372397151,-13.3890130654928,-38.4302426110392));
#20339=CARTESIAN_POINT('Ctrl Pts',(29.505753620787,-13.3645846069503,-38.4017858911997));
#20340=CARTESIAN_POINT('Ctrl Pts',(29.502706973872,-13.3566532439626,-38.3925466437009));
#20341=CARTESIAN_POINT('Ctrl Pts',(29.499733451499,-13.348431556951,-38.3835291533526));
#20342=CARTESIAN_POINT('Ctrl Pts',(29.4968391572844,-13.3399225829037,-38.3747519299551));
#20343=CARTESIAN_POINT('Ctrl Pts',(29.4968079493295,-13.339830834222,-38.3746572888538));
#20344=CARTESIAN_POINT('Ctrl Pts',(29.4967767506818,-13.3397390509053,-38.3745626759776));
#20345=CARTESIAN_POINT('Ctrl Pts',(29.4967455613462,-13.3396472329756,-38.3744680913411));
#20346=CARTESIAN_POINT('Ctrl Pts',(29.485255261427,-13.3058210700066,-38.3396226603605));
#20347=CARTESIAN_POINT('Ctrl Pts',(29.475076277546,-13.267440322379,-38.3087539204414));
#20348=CARTESIAN_POINT('Ctrl Pts',(29.4664377760755,-13.2257618865122,-38.2825568404197));
#20349=CARTESIAN_POINT('Ctrl Pts',(29.4618903252278,-13.2038216646858,-38.2687662617925));
#20350=CARTESIAN_POINT('Ctrl Pts',(29.4577699082708,-13.1809667715091,-38.2562707041878));
#20351=CARTESIAN_POINT('Ctrl Pts',(29.4541112021333,-13.1573764603984,-38.245175328701));
#20352=CARTESIAN_POINT('Ctrl Pts',(29.4482111530888,-13.1193345987958,-38.2272828669731));
#20353=CARTESIAN_POINT('Ctrl Pts',(29.4435099348019,-13.0793753611095,-38.2130259739134));
#20354=CARTESIAN_POINT('Ctrl Pts',(29.4401602474623,-13.0382175959794,-38.2028677274188));
#20355=CARTESIAN_POINT('Ctrl Pts',(29.4368767709741,-12.9978733666794,-38.192910271649));
#20356=CARTESIAN_POINT('Ctrl Pts',(29.4348920783845,-12.9563778844129,-38.1868915019856));
#20357=CARTESIAN_POINT('Ctrl Pts',(29.4343654883888,-12.9144212112981,-38.1852945675748));
#20358=CARTESIAN_POINT('Ctrl Pts',(29.4342714552248,-12.9069290090975,-38.185009403032));
#20359=CARTESIAN_POINT('Ctrl Pts',(29.4342239572584,-12.8994221374127,-38.1848653609166));
#20360=CARTESIAN_POINT('Ctrl Pts',(29.4342239561067,-12.8919045823054,-38.184865357424));
#20361=CARTESIAN_POINT('',(31.8550769043756,-13.5169045823054,-45.5263329281778));
#20362=CARTESIAN_POINT('',(15.1746248258407,-13.5169045823054,5.05872969929124));
#20363=CARTESIAN_POINT('',(32.1607495565261,-14.4544045724555,-46.4533144140353));
#20364=CARTESIAN_POINT('Origin',(-385.578293801187,-1402.30169514568,1220.38019629327));
#20365=CARTESIAN_POINT('',(15.1746248258407,-14.4544045823054,5.05872969929124));
#20366=CARTESIAN_POINT('Origin',(20.8581949540281,-11.0169045823054,6.93289005877139));
#20367=CARTESIAN_POINT('',(20.8581949540281,-11.3294045823054,6.93289005877139));
#20368=CARTESIAN_POINT('',(20.8581949540281,-11.3294045823054,6.93289005877131));
#20369=CARTESIAN_POINT('',(20.8581949540281,-14.4544045823054,6.93289005877139));
#20370=CARTESIAN_POINT('',(20.8581949540281,-11.0169045823054,6.93289005877139));
#20371=CARTESIAN_POINT('',(37.1077603633878,-14.4544045474399,-42.3454676279164));
#20372=CARTESIAN_POINT('',(37.4052635491749,-14.4544045823054,-43.2476744274668));
#20373=CARTESIAN_POINT('',(36.7879602992159,-13.5169045823054,-41.3756434170181));
#20374=CARTESIAN_POINT('Origin',(-151.647538790397,-669.972713648666,530.072988729517));
#20375=CARTESIAN_POINT('',(34.4520919977564,-13.5169045823054,-34.2918998972067));
#20376=CARTESIAN_POINT('',(34.3920744991467,-13.5169045823054,-34.1098911056212));
#20377=CARTESIAN_POINT('Ctrl Pts',(34.2319046026008,-12.8919045823054,-33.6241606104486));
#20378=CARTESIAN_POINT('Ctrl Pts',(34.2319046026008,-12.9240089539757,-33.6241606104486));
#20379=CARTESIAN_POINT('Ctrl Pts',(34.2327660676948,-12.955801183813,-33.6267730855496));
#20380=CARTESIAN_POINT('Ctrl Pts',(34.2344596877549,-12.9870390822744,-33.6319091499924));
#20381=CARTESIAN_POINT('Ctrl Pts',(34.2361941274839,-13.0190298772671,-33.6371690039758));
#20382=CARTESIAN_POINT('Ctrl Pts',(34.2388012607647,-13.0504387215055,-33.6450753844307));
#20383=CARTESIAN_POINT('Ctrl Pts',(34.2422325669316,-13.0810143824795,-33.655481147807));
#20384=CARTESIAN_POINT('Ctrl Pts',(34.2446351437452,-13.1024232485338,-33.6627671912553));
#20385=CARTESIAN_POINT('Ctrl Pts',(34.2474414246086,-13.1234238076974,-33.6712775057571));
#20386=CARTESIAN_POINT('Ctrl Pts',(34.2506302568241,-13.1439346499851,-33.6809479437379));
#20387=CARTESIAN_POINT('Ctrl Pts',(34.25064462592,-13.1440270732421,-33.6809915193923));
#20388=CARTESIAN_POINT('Ctrl Pts',(34.2506590017993,-13.1441194808469,-33.6810351156181));
#20389=CARTESIAN_POINT('Ctrl Pts',(34.2506733844596,-13.1442118727969,-33.681078732408));
#20390=CARTESIAN_POINT('Ctrl Pts',(34.262088806318,-13.2175427492195,-33.7156970884852));
#20391=CARTESIAN_POINT('Ctrl Pts',(34.2778470820053,-13.2814833078763,-33.7634855632141));
#20392=CARTESIAN_POINT('Ctrl Pts',(34.297083605806,-13.3355724238096,-33.8218221572446));
#20393=CARTESIAN_POINT('Ctrl Pts',(34.2984164892935,-13.3393202157823,-33.8258642536082));
#20394=CARTESIAN_POINT('Ctrl Pts',(34.2997660765859,-13.3430206976121,-33.8299570058538));
#20395=CARTESIAN_POINT('Ctrl Pts',(34.3011320820256,-13.3466737099125,-33.8340995476976));
#20396=CARTESIAN_POINT('Ctrl Pts',(34.3011486427789,-13.3467179971708,-33.8341497697625));
#20397=CARTESIAN_POINT('Ctrl Pts',(34.30116520512,-13.3467622754629,-33.8341999966422));
#20398=CARTESIAN_POINT('Ctrl Pts',(34.3011817690487,-13.3468065447896,-33.8342502283365));
#20399=CARTESIAN_POINT('Ctrl Pts',(34.3222770796446,-13.4031865990188,-33.8982237706922));
#20400=CARTESIAN_POINT('Ctrl Pts',(34.3459380694435,-13.4450083105498,-33.9699779800617));
#20401=CARTESIAN_POINT('Ctrl Pts',(34.3718849768693,-13.4738659092279,-34.0486644527659));
#20402=CARTESIAN_POINT('Ctrl Pts',(34.3978462731079,-13.5027395108376,-34.127394560918));
#20403=CARTESIAN_POINT('Ctrl Pts',(34.4246047850287,-13.5169045582356,-34.2085423016968));
#20404=CARTESIAN_POINT('Ctrl Pts',(34.4520919977564,-13.5169045823054,-34.2918998972067));
#20405=CARTESIAN_POINT('Origin',(0.0835265683620477,-6.01690458230549,0.0824317919394229));
#20406=CARTESIAN_POINT('',(48.4286602621091,-6.10843422628167,-4.13831834965265));
#20407=CARTESIAN_POINT('',(36.459401449836,-6.10843371299757,-32.0401832164143));
#20408=CARTESIAN_POINT('Origin',(0.0835265683620477,-6.10843371318468,0.0824317919394229));
#20409=CARTESIAN_POINT('',(38.7825797314222,-12.6709337131846,-39.1280242913702));
#20410=CARTESIAN_POINT('Ctrl Pts',(36.4594014504071,-6.10843371318764,-32.0401832160548));
#20411=CARTESIAN_POINT('Ctrl Pts',(36.6177503688256,-6.54712953979038,-32.5236246202131));
#20412=CARTESIAN_POINT('Ctrl Pts',(36.7757172835296,-6.98698298252111,-33.0061517892532));
#20413=CARTESIAN_POINT('Ctrl Pts',(36.9334136781008,-7.42790908716257,-33.4877815134637));
#20414=CARTESIAN_POINT('Ctrl Pts',(37.0904935659948,-7.8671114118254,-33.967528328799));
#20415=CARTESIAN_POINT('Ctrl Pts',(37.2473051036632,-8.30737802775023,-34.4463847898388));
#20416=CARTESIAN_POINT('Ctrl Pts',(37.4039138029555,-8.74862497320324,-34.9243934293266));
#20417=CARTESIAN_POINT('Ctrl Pts',(37.5602173246846,-9.18901207710122,-35.4014705911098));
#20418=CARTESIAN_POINT('Ctrl Pts',(37.7163188570147,-9.63037569358639,-35.8777032990578));
#20419=CARTESIAN_POINT('Ctrl Pts',(37.8722380448622,-10.0726323508084,-36.3531585902921));
#20420=CARTESIAN_POINT('Ctrl Pts',(38.0277161383152,-10.5136378667497,-36.8272688215204));
#20421=CARTESIAN_POINT('Ctrl Pts',(38.1830129581763,-10.955531377762,-37.3006060886532));
#20422=CARTESIAN_POINT('Ctrl Pts',(38.3381019771589,-11.3982301184165,-37.7732605459248));
#20423=CARTESIAN_POINT('Ctrl Pts',(38.4864727775814,-11.8217518282566,-38.2254403366584));
#20424=CARTESIAN_POINT('Ctrl Pts',(38.63465313382,-12.2460105161165,-38.6769953773671));
#20425=CARTESIAN_POINT('Ctrl Pts',(38.7825797314222,-12.6709337131846,-39.1280242913702));
#20426=CARTESIAN_POINT('',(38.4984968574033,-13.2959337131846,-40.2737533112661));
#20427=CARTESIAN_POINT('Ctrl Pts',(38.4984968574034,-13.2959337131846,-40.273753311266));
#20428=CARTESIAN_POINT('Ctrl Pts',(38.5331904713011,-13.2959336603243,-40.2407284579781));
#20429=CARTESIAN_POINT('Ctrl Pts',(38.5644068713101,-13.291660512867,-40.2050259534244));
#20430=CARTESIAN_POINT('Ctrl Pts',(38.5925219243482,-13.2840750781511,-40.1676284350549));
#20431=CARTESIAN_POINT('Ctrl Pts',(38.6250024648541,-13.2753118359401,-40.1244241199653));
#20432=CARTESIAN_POINT('Ctrl Pts',(38.6533440434163,-13.2621273075647,-40.0789565662769));
#20433=CARTESIAN_POINT('Ctrl Pts',(38.6780885048562,-13.2459526169403,-40.032706281476));
#20434=CARTESIAN_POINT('Ctrl Pts',(38.6853255888349,-13.2412219585397,-40.0191793273347));
#20435=CARTESIAN_POINT('Ctrl Pts',(38.692254746233,-13.2362352705224,-40.005585284207));
#20436=CARTESIAN_POINT('Ctrl Pts',(38.6988890084814,-13.2310278528738,-39.9919609828319));
#20437=CARTESIAN_POINT('Ctrl Pts',(38.6989109743279,-13.2310106112676,-39.9919158731721));
#20438=CARTESIAN_POINT('Ctrl Pts',(38.6989329369403,-13.230993367242,-39.9918707631823));
#20439=CARTESIAN_POINT('Ctrl Pts',(38.6989548963189,-13.2309761207981,-39.9918256528639));
#20440=CARTESIAN_POINT('Ctrl Pts',(38.7427007443125,-13.1966190324461,-39.9019602168528));
#20441=CARTESIAN_POINT('Ctrl Pts',(38.7735109344404,-13.1525556490531,-39.810753760552));
#20442=CARTESIAN_POINT('Ctrl Pts',(38.7942479882117,-13.1028429791957,-39.7212397410345));
#20443=CARTESIAN_POINT('Ctrl Pts',(38.796698753037,-13.0969677924886,-39.7106607160278));
#20444=CARTESIAN_POINT('Ctrl Pts',(38.799008865195,-13.0910137402717,-39.7001053460992));
#20445=CARTESIAN_POINT('Ctrl Pts',(38.8011830809703,-13.0849875486837,-39.6895786502124));
#20446=CARTESIAN_POINT('Ctrl Pts',(38.8012082331003,-13.0849178354768,-39.6894568735118));
#20447=CARTESIAN_POINT('Ctrl Pts',(38.8012333665422,-13.0848481114876,-39.6893350995626));
#20448=CARTESIAN_POINT('Ctrl Pts',(38.8012584813034,-13.0847783767298,-39.6892133283766));
#20449=CARTESIAN_POINT('Ctrl Pts',(38.8063708461711,-13.0705831581647,-39.6644255660912));
#20450=CARTESIAN_POINT('Ctrl Pts',(38.8107403271801,-13.0558793142743,-39.6396345669642));
#20451=CARTESIAN_POINT('Ctrl Pts',(38.8143720370972,-13.0407301262923,-39.6149263152304));
#20452=CARTESIAN_POINT('Ctrl Pts',(38.8198463634219,-13.0178947125452,-39.5776818667505));
#20453=CARTESIAN_POINT('Ctrl Pts',(38.823645519602,-12.9940463246918,-39.5406227563601));
#20454=CARTESIAN_POINT('Ctrl Pts',(38.8257918572288,-12.9693962501975,-39.5040316466717));
#20455=CARTESIAN_POINT('Ctrl Pts',(38.8279381948557,-12.9447461757032,-39.4674405369834));
#20456=CARTESIAN_POINT('Ctrl Pts',(38.8284317229906,-12.9192944015675,-39.4313174373128));
#20457=CARTESIAN_POINT('Ctrl Pts',(38.8272948694351,-12.8932521061511,-39.3959450880251));
#20458=CARTESIAN_POINT('Ctrl Pts',(38.826328746216,-12.8711207892723,-39.3658848856384));
#20459=CARTESIAN_POINT('Ctrl Pts',(38.8242284614393,-12.8485482515867,-39.3363038677842));
#20460=CARTESIAN_POINT('Ctrl Pts',(38.8209322963513,-12.8255048445995,-39.3072258776694));
#20461=CARTESIAN_POINT('Ctrl Pts',(38.819056923723,-12.8123941618594,-39.2906817831558));
#20462=CARTESIAN_POINT('Ctrl Pts',(38.8167936529581,-12.799130872597,-39.2743010308738));
#20463=CARTESIAN_POINT('Ctrl Pts',(38.81412530896,-12.7857088195892,-39.2580927786456));
#20464=CARTESIAN_POINT('Ctrl Pts',(38.8093643068945,-12.7617604747961,-39.2291731481964));
#20465=CARTESIAN_POINT('Ctrl Pts',(38.8033163192104,-12.7373067239541,-39.2008001973807));
#20466=CARTESIAN_POINT('Ctrl Pts',(38.7959160408695,-12.7123167139302,-39.1730000886664));
#20467=CARTESIAN_POINT('Ctrl Pts',(38.7918790162404,-12.6986840799535,-39.1578344802393));
#20468=CARTESIAN_POINT('Ctrl Pts',(38.7874388547392,-12.6848916910894,-39.1428398006197));
#20469=CARTESIAN_POINT('Ctrl Pts',(38.7825797314222,-12.6709337131846,-39.1280242913702));
#20470=CARTESIAN_POINT('',(37.2320718162657,-13.2959337131846,-41.4424668154812));
#20471=CARTESIAN_POINT('Origin',(0.0835265683620477,-13.2959337131846,0.0824317919394229));
#20472=CARTESIAN_POINT('',(37.7005406317231,-14.6753754514262,-42.8699853978345));
#20473=CARTESIAN_POINT('Origin',(-133.456925507265,-671.736420006179,537.350524279956));
#20474=CARTESIAN_POINT('',(48.3955020421714,-14.675375306047,-30.3462213479384));
#20475=CARTESIAN_POINT('Origin',(0.0835265683620477,-14.6753754514262,0.0824317919394229));
#20476=CARTESIAN_POINT('Ctrl Pts',(48.395502411215,-14.6753748699083,-30.3462215803797));
#20477=CARTESIAN_POINT('Ctrl Pts',(48.3970165064124,-14.2165313286484,-29.4828741133762));
#20478=CARTESIAN_POINT('Ctrl Pts',(48.3985257931811,-13.7688961383428,-28.614397690063));
#20479=CARTESIAN_POINT('Ctrl Pts',(48.4000249035474,-13.3339028935805,-27.7401315814044));
#20480=CARTESIAN_POINT('Ctrl Pts',(48.4014813424394,-12.9112915277744,-26.8907510480124));
#20481=CARTESIAN_POINT('Ctrl Pts',(48.4029281735502,-12.5006127529904,-26.0359056762573));
#20482=CARTESIAN_POINT('Ctrl Pts',(48.4043602774117,-12.103139198672,-25.1750154147393));
#20483=CARTESIAN_POINT('Ctrl Pts',(48.4048913764569,-11.9557352073326,-24.855752260564));
#20484=CARTESIAN_POINT('Ctrl Pts',(48.4054204482461,-11.8101469177382,-24.5356580098551));
#20485=CARTESIAN_POINT('Ctrl Pts',(48.4059472256945,-11.6664376689278,-24.2147040460321));
#20486=CARTESIAN_POINT('Ctrl Pts',(48.4060000541633,-11.6520256252871,-24.1825168168067));
#20487=CARTESIAN_POINT('Ctrl Pts',(48.4060528586946,-11.6376325718392,-24.1503208891208));
#20488=CARTESIAN_POINT('Ctrl Pts',(48.4061056388366,-11.6232585917442,-24.118116222714));
#20489=CARTESIAN_POINT('Ctrl Pts',(48.4073722199955,-11.2783218091964,-23.3452910246814));
#20490=CARTESIAN_POINT('Ctrl Pts',(48.4086232798676,-10.9443666880957,-22.567421367977));
#20491=CARTESIAN_POINT('Ctrl Pts',(48.4098496480416,-10.6225428079207,-21.784018721879));
#20492=CARTESIAN_POINT('Ctrl Pts',(48.4102724995876,-10.5115779866166,-21.5139016174983));
#20493=CARTESIAN_POINT('Ctrl Pts',(48.4106924186025,-10.4020550274973,-21.2431269446329));
#20494=CARTESIAN_POINT('Ctrl Pts',(48.4111090387546,-10.2940198074426,-20.971675429716));
#20495=CARTESIAN_POINT('Ctrl Pts',(48.4111340145,-10.2875432600576,-20.9554023236105));
#20496=CARTESIAN_POINT('Ctrl Pts',(48.4111589786261,-10.2810720136184,-20.9391265270569));
#20497=CARTESIAN_POINT('Ctrl Pts',(48.4111839309784,-10.2746060938735,-20.922848081286));
#20498=CARTESIAN_POINT('Ctrl Pts',(48.4118827329214,-10.0935250792971,-20.4669628256337));
#20499=CARTESIAN_POINT('Ctrl Pts',(48.4125729062024,-9.91663263835351,-20.0090368445298));
#20500=CARTESIAN_POINT('Ctrl Pts',(48.4132521719491,-9.74425107303465,-19.5493017432801));
#20501=CARTESIAN_POINT('Ctrl Pts',(48.4139027926854,-9.57913893319766,-19.1089539242711));
#20502=CARTESIAN_POINT('Ctrl Pts',(48.4145434106902,-9.41816464515814,-18.6669448938639));
#20503=CARTESIAN_POINT('Ctrl Pts',(48.4151719180711,-9.26165511783415,-18.2234627935507));
#20504=CARTESIAN_POINT('Ctrl Pts',(48.415435037911,-9.19613359329876,-18.0378023816033));
#20505=CARTESIAN_POINT('Ctrl Pts',(48.4156960335652,-9.13139516041176,-17.851883727953));
#20506=CARTESIAN_POINT('Ctrl Pts',(48.4159547419103,-9.06746659619111,-17.6657206784883));
#20507=CARTESIAN_POINT('Ctrl Pts',(48.4159597463539,-9.06622996466504,-17.6621195480896));
#20508=CARTESIAN_POINT('Ctrl Pts',(48.4159647498858,-9.06499364665102,-17.6585183566049));
#20509=CARTESIAN_POINT('Ctrl Pts',(48.4159697525046,-9.06375764243243,-17.654917104426));
#20510=CARTESIAN_POINT('Ctrl Pts',(48.4171758193888,-8.76577296157743,-16.7867016363302));
#20511=CARTESIAN_POINT('Ctrl Pts',(48.418330759243,-8.48534970203332,-15.9132437322746));
#20512=CARTESIAN_POINT('Ctrl Pts',(48.4194226489004,-8.22405492478902,-15.0341112036849));
#20513=CARTESIAN_POINT('Ctrl Pts',(48.4197035105318,-8.15684330051223,-14.8079760860058));
#20514=CARTESIAN_POINT('Ctrl Pts',(48.4199801982767,-8.09089757124237,-14.5814654555463));
#20515=CARTESIAN_POINT('Ctrl Pts',(48.4202525046535,-8.02624496071548,-14.3545718466408));
#20516=CARTESIAN_POINT('Ctrl Pts',(48.4208747192833,-7.87851503755607,-13.8361244841013));
#20517=CARTESIAN_POINT('Ctrl Pts',(48.4214742831675,-7.73745329660274,-13.315369950669));
#20518=CARTESIAN_POINT('Ctrl Pts',(48.4220479333675,-7.60353311382448,-12.7927342626265));
#20519=CARTESIAN_POINT('Ctrl Pts',(48.4225989655767,-7.47489316188464,-12.2907051554594));
#20520=CARTESIAN_POINT('Ctrl Pts',(48.4231260855195,-7.35284273129863,-11.7869403092735));
#20521=CARTESIAN_POINT('Ctrl Pts',(48.4236265540814,-7.23775611982599,-11.2818266328076));
#20522=CARTESIAN_POINT('Ctrl Pts',(48.4238051253453,-7.19669227839415,-11.1015979541626));
#20523=CARTESIAN_POINT('Ctrl Pts',(48.4239803068534,-7.15651419440814,-10.9211957470908));
#20524=CARTESIAN_POINT('Ctrl Pts',(48.4241519678033,-7.11724012295319,-10.7406508058928));
#20525=CARTESIAN_POINT('Ctrl Pts',(48.4251874613739,-6.88033098026176,-9.65156720309959));
#20526=CARTESIAN_POINT('Ctrl Pts',(48.4260950282616,-6.67627260244589,-8.55708589982596));
#20527=CARTESIAN_POINT('Ctrl Pts',(48.426853401255,-6.50737682457182,-7.45682324763825));
#20528=CARTESIAN_POINT('Ctrl Pts',(48.4276117742484,-6.33848104669775,-6.35656059545055));
#20529=CARTESIAN_POINT('Ctrl Pts',(48.4282209516793,-6.20474805616907,-5.25051655743529));
#20530=CARTESIAN_POINT('Ctrl Pts',(48.4286600676394,-6.10843510301224,-4.13831837467277));
#20531=CARTESIAN_POINT('Origin',(0.0835265683620477,11.4830954176946,0.0824317919394229));
#20532=CARTESIAN_POINT('',(36.0852727571828,-3.61941807409668,-34.1625959873708));
#20533=CARTESIAN_POINT('',(36.0852727571828,11.9341984494201,-34.1625959873708));
#20534=CARTESIAN_POINT('',(36.0852727571828,11.4830954176946,-34.1625959873708));
#20535=CARTESIAN_POINT('',(36.0852727571827,11.9341984494201,34.3274595712498));
#20536=CARTESIAN_POINT('Origin',(0.0835265683620477,11.9341984494201,0.0824317919394229));
#20537=CARTESIAN_POINT('',(36.0852727571827,-3.61941807409668,34.3274595712498));
#20538=CARTESIAN_POINT('',(36.0852727571827,11.4830954176946,34.3274595712498));
#20539=CARTESIAN_POINT('Origin',(0.0835265683620477,-3.61941807409668,0.0824317919394229));
#20540=CARTESIAN_POINT('Origin',(0.0835265683620477,12.0636401876617,0.0824317919394229));
#20541=CARTESIAN_POINT('',(36.7737075413345,13.0346110567824,35.0125232743287));
#20542=CARTESIAN_POINT('',(36.1515914195991,12.155169318541,34.3905421902096));
#20543=CARTESIAN_POINT('',(36.7737075413348,13.0346110567825,35.0125232743285));
#20544=CARTESIAN_POINT('',(36.151591419599,12.1551693185413,-34.2256786063311));
#20545=CARTESIAN_POINT('Origin',(0.0835265683620477,12.1551693185409,0.0824317919394229));
#20546=CARTESIAN_POINT('',(36.7737075413349,13.0346110567825,-34.8476596904496));
#20547=CARTESIAN_POINT('',(36.1515914195989,12.1551693185409,-34.2256786063308));
#20548=CARTESIAN_POINT('',(49.9887116253026,13.0346110567825,-8.62119821111519));
#20549=CARTESIAN_POINT('Origin',(0.0835265683620477,13.0346110567825,0.0824317919394229));
#20550=CARTESIAN_POINT('',(49.9887116253026,13.0346110567825,8.78606179499438));
#20551=CARTESIAN_POINT('Ctrl Pts',(49.9887116253026,13.0346110567825,-8.62119821111519));
#20552=CARTESIAN_POINT('Ctrl Pts',(49.9893478560974,12.8871967548494,-7.75954228903555));
#20553=CARTESIAN_POINT('Ctrl Pts',(49.9899000357746,12.7606786217836,-6.89565773289813));
#20554=CARTESIAN_POINT('Ctrl Pts',(49.9903598055825,12.6558408130361,-6.02947623345575));
#20555=CARTESIAN_POINT('Ctrl Pts',(49.990665808201,12.5860653657491,-5.45298381838726));
#20556=CARTESIAN_POINT('Ctrl Pts',(49.990930885539,12.5258925150002,-4.8754741482685));
#20557=CARTESIAN_POINT('Ctrl Pts',(49.99115267096,12.4755408811194,-4.29692965082524));
#20558=CARTESIAN_POINT('Ctrl Pts',(49.9911538902138,12.4752640756467,-4.29374913272224));
#20559=CARTESIAN_POINT('Ctrl Pts',(49.9911551081487,12.4749875690303,-4.29056855464817));
#20560=CARTESIAN_POINT('Ctrl Pts',(49.9911563247646,12.4747113612848,-4.28738791693494));
#20561=CARTESIAN_POINT('Ctrl Pts',(49.9913179387918,12.4380202039338,-3.86487522247577));
#20562=CARTESIAN_POINT('Ctrl Pts',(49.9914565488923,12.4066244501982,-3.44160145281131));
#20563=CARTESIAN_POINT('Ctrl Pts',(49.9915720324612,12.3805167222718,-3.01783128710948));
#20564=CARTESIAN_POINT('Ctrl Pts',(49.991688629906,12.3541571769569,-2.5899737225819));
#20565=CARTESIAN_POINT('Ctrl Pts',(49.991781653618,12.3331879704902,-2.16160894685783));
#20566=CARTESIAN_POINT('Ctrl Pts',(49.9918507579081,12.3176520559872,-1.73299266868656));
#20567=CARTESIAN_POINT('Ctrl Pts',(49.9919186373041,12.3023915201941,-1.31197374165334));
#20568=CARTESIAN_POINT('Ctrl Pts',(49.9919634378385,12.292373396783,-0.890710996911061));
#20569=CARTESIAN_POINT('Ctrl Pts',(49.9919846138091,12.2876877721247,-0.469448250446118));
#20570=CARTESIAN_POINT('Ctrl Pts',(49.9919938577277,12.2856423625376,-0.285554976195753));
#20571=CARTESIAN_POINT('Ctrl Pts',(49.991998596967,12.2846137392985,-0.101661822245885));
#20572=CARTESIAN_POINT('Ctrl Pts',(49.9919987726311,12.2846124143566,0.0822099968334337));
#20573=CARTESIAN_POINT('Ctrl Pts',(49.9919987763777,12.2846123860983,0.0861316130377299));
#20574=CARTESIAN_POINT('Ctrl Pts',(49.9919987780095,12.2846128251731,0.0900531737555135));
#20575=CARTESIAN_POINT('Ctrl Pts',(49.991998777526,12.2846137316597,0.0939746783873438));
#20576=CARTESIAN_POINT('Ctrl Pts',(49.9919986349354,12.2848811103967,1.25066806982682));
#20577=CARTESIAN_POINT('Ctrl Pts',(49.9918145061858,12.3254286613201,2.40515107505473));
#20578=CARTESIAN_POINT('Ctrl Pts',(49.9914604149175,12.4051717607756,3.55744718045229));
#20579=CARTESIAN_POINT('Ctrl Pts',(49.9913692018685,12.4257133891542,3.85427585328813));
#20580=CARTESIAN_POINT('Ctrl Pts',(49.9912667127974,12.448855628615,4.15095943259262));
#20581=CARTESIAN_POINT('Ctrl Pts',(49.9911531925445,12.4745793828316,4.44749836453926));
#20582=CARTESIAN_POINT('Ctrl Pts',(49.9909438913061,12.522007163138,4.99423750681911));
#20583=CARTESIAN_POINT('Ctrl Pts',(49.990696665258,12.5782201197775,5.54055086955121));
#20584=CARTESIAN_POINT('Ctrl Pts',(49.9904129303823,12.6430432691593,6.08604846635906));
#20585=CARTESIAN_POINT('Ctrl Pts',(49.9901251899494,12.7087815433771,6.6392469910537));
#20586=CARTESIAN_POINT('Ctrl Pts',(49.9897999034691,12.7833747881785,7.19160655594086));
#20587=CARTESIAN_POINT('Ctrl Pts',(49.9894387770557,12.866586934251,7.74272639699184));
#20588=CARTESIAN_POINT('Ctrl Pts',(49.9892105457498,12.9191768752446,8.0910332402735));
#20589=CARTESIAN_POINT('Ctrl Pts',(49.9889680037392,12.9752083234145,8.43884503024982));
#20590=CARTESIAN_POINT('Ctrl Pts',(49.9887116253026,13.0346110567825,8.78606179499438));
#20591=CARTESIAN_POINT('Origin',(0.0835265683620477,13.0346110567825,0.0824317919394229));
#20592=CARTESIAN_POINT('Origin',(0.0835265683622866,-8.56135981233827,-68.3550682080606));
#20593=CARTESIAN_POINT('',(49.7710265683621,-8.56135981233827,-22.6228153633312));
#20594=CARTESIAN_POINT('',(49.7710265683622,-8.56135981233827,-44.2925682080604));
#20595=CARTESIAN_POINT('',(49.7710265683623,-8.56135981233827,-68.3550682080604));
#20596=CARTESIAN_POINT('',(44.4585265683622,-8.56135981233827,-49.6050682080606));
#20597=CARTESIAN_POINT('Origin',(44.4585265683622,-8.56135981233827,-44.2925682080604));
#20598=CARTESIAN_POINT('',(22.7887737236329,-8.56135981233827,-49.6050682080606));
#20599=CARTESIAN_POINT('',(0.0835265683622903,-8.56135981233827,-49.6050682080606));
#20600=CARTESIAN_POINT('',(37.8183782124907,-8.56135981233827,-39.4201868051553));
#20601=CARTESIAN_POINT('Origin',(0.0835265683620477,-8.56135981233827,0.0824317919394229));
#20602=CARTESIAN_POINT('',(38.9743995336223,-8.56135981233827,-40.5762081262869));
#20603=CARTESIAN_POINT('',(39.586145165457,-8.56135981233827,-37.6524198521889));
#20604=CARTESIAN_POINT('',(39.4990275410653,-8.56135981233827,-37.5653022277972));
#20605=CARTESIAN_POINT('Origin',(0.0835265683620477,-8.56135981233827,0.0824317919394229));
#20606=CARTESIAN_POINT('Origin',(0.0835265683622249,13.1261401876617,-50.6675682080606));
#20607=CARTESIAN_POINT('',(11.0320394968432,13.1261401876617,-49.6050682080606));
#20608=CARTESIAN_POINT('',(44.4585265683622,13.1261401876617,-49.6050682080606));
#20609=CARTESIAN_POINT('',(0.0835265683622251,13.1261401876617,-49.6050682080606));
#20610=CARTESIAN_POINT('',(49.7710265683622,13.1261401876617,-44.2925682080604));
#20611=CARTESIAN_POINT('Origin',(44.4585265683622,13.1261401876617,-44.2925682080604));
#20612=CARTESIAN_POINT('',(49.7710265683621,13.1261401876617,-10.8660811365416));
#20613=CARTESIAN_POINT('',(49.7710265683622,13.1261401876617,-50.6675682080604));
#20614=CARTESIAN_POINT('',(36.9337491106658,13.1261401876617,-35.0000237973977));
#20615=CARTESIAN_POINT('Origin',(0.0835265683620477,13.1261401876617,0.0824317919394229));
#20616=CARTESIAN_POINT('',(40.7421664865887,13.1261401876617,-38.8084411733206));
#20617=CARTESIAN_POINT('',(40.7421664865887,13.1261401876617,-38.8084411733205));
#20618=CARTESIAN_POINT('',(38.9743995336223,13.1261401876617,-40.5762081262869));
#20619=CARTESIAN_POINT('Origin',(39.8582830101055,13.1261401876617,-39.6923246498037));
#20620=CARTESIAN_POINT('',(35.1659821576994,13.1261401876617,-36.7677907503641));
#20621=CARTESIAN_POINT('',(35.0791887533698,13.1261401876617,-36.6809973460344));
#20622=CARTESIAN_POINT('Origin',(0.0835265683620477,13.1261401876617,0.0824317919394229));
#20623=CARTESIAN_POINT('Origin',(50.0835265683621,16.4830954176946,0.0824317919395974));
#20624=CARTESIAN_POINT('',(50.083526568362,-8.87385981233827,22.7876789472104));
#20625=CARTESIAN_POINT('',(50.0835265683619,-8.87385981233827,36.6697170232579));
#20626=CARTESIAN_POINT('',(50.0835265683621,-8.87385981233827,0.0824317919395974));
#20627=CARTESIAN_POINT('',(50.0835265683619,-14.4544045823054,36.6697170232579));
#20628=CARTESIAN_POINT('',(50.0835265683619,16.4830954176946,36.6697170232579));
#20629=CARTESIAN_POINT('',(50.0835265683622,-14.4544045823054,-44.2925682080604));
#20630=CARTESIAN_POINT('',(50.0835265683621,-14.4544045823054,0.0824317919395974));
#20631=CARTESIAN_POINT('',(50.0835265683622,-8.87385981233827,-44.2925682080604));
#20632=CARTESIAN_POINT('',(50.0835265683622,16.4830954176946,-44.2925682080604));
#20633=CARTESIAN_POINT('',(50.0835265683621,-8.87385981233827,-22.6228153633312));
#20634=CARTESIAN_POINT('',(50.0835265683621,-8.87385981233827,0.0824317919395974));
#20635=CARTESIAN_POINT('',(50.0835265683621,-8.69080155057986,-21.5378711661598));
#20636=CARTESIAN_POINT('Ctrl Pts',(50.0835265683621,-8.69080155057987,-21.5378711661598));
#20637=CARTESIAN_POINT('Ctrl Pts',(50.0835265683621,-8.73475654613112,-21.6480367600604));
#20638=CARTESIAN_POINT('Ctrl Pts',(50.0835265683621,-8.76821292000551,-21.7616061533008));
#20639=CARTESIAN_POINT('Ctrl Pts',(50.0835265683621,-8.79411643469755,-21.8764708457468));
#20640=CARTESIAN_POINT('Ctrl Pts',(50.0835265683621,-8.80879390138821,-21.9415555540326));
#20641=CARTESIAN_POINT('Ctrl Pts',(50.0835265683621,-8.8210476068989,-22.0070558185655));
#20642=CARTESIAN_POINT('Ctrl Pts',(50.083526568362,-8.83141832822413,-22.0725884285981));
#20643=CARTESIAN_POINT('Ctrl Pts',(50.0835265683619,-8.83143478595685,-22.072692425046));
#20644=CARTESIAN_POINT('Ctrl Pts',(50.0835265683619,-8.83145123875071,-22.0727964220728));
#20645=CARTESIAN_POINT('Ctrl Pts',(50.0835265683619,-8.83146768660594,-22.0729004196781));
#20646=CARTESIAN_POINT('Ctrl Pts',(50.0835265683616,-8.86014040550798,-22.2541942152644));
#20647=CARTESIAN_POINT('Ctrl Pts',(50.0835265683621,-8.87385980853305,-22.4375560999868));
#20648=CARTESIAN_POINT('Ctrl Pts',(50.0835265683621,-8.87385981233827,-22.6228153633312));
#20649=CARTESIAN_POINT('',(50.083526568362,-8.69080155057986,21.702734750039));
#20650=CARTESIAN_POINT('Ctrl Pts',(50.0835265683621,-8.69080155057986,-21.5378711661598));
#20651=CARTESIAN_POINT('Ctrl Pts',(50.0835265683621,-8.34768669240312,-20.6779139118167));
#20652=CARTESIAN_POINT('Ctrl Pts',(50.0835265683621,-8.01980178776899,-19.8131224223239));
#20653=CARTESIAN_POINT('Ctrl Pts',(50.083526568362,-7.7086638179161,-18.9430124229936));
#20654=CARTESIAN_POINT('Ctrl Pts',(50.0835265683619,-7.39752584806321,-18.0729024236633));
#20655=CARTESIAN_POINT('Ctrl Pts',(50.0835265683619,-7.10313511035522,-17.1974737894229));
#20656=CARTESIAN_POINT('Ctrl Pts',(50.083526568362,-6.8269564419545,-16.316264163741));
#20657=CARTESIAN_POINT('Ctrl Pts',(50.083526568362,-6.82354225770081,-16.3053704475622));
#20658=CARTESIAN_POINT('Ctrl Pts',(50.083526568362,-6.82013086172525,-16.294475845857));
#20659=CARTESIAN_POINT('Ctrl Pts',(50.083526568362,-6.81672225716413,-16.2835803575982));
#20660=CARTESIAN_POINT('Ctrl Pts',(50.0835265683622,-6.58377695494992,-15.5389786416461));
#20661=CARTESIAN_POINT('Ctrl Pts',(50.0835265683636,-6.36386066861884,-14.7901976392119));
#20662=CARTESIAN_POINT('Ctrl Pts',(50.0835265683606,-6.15798672711213,-14.0370234161259));
#20663=CARTESIAN_POINT('Ctrl Pts',(50.0835265683601,-6.12185688864097,-13.9048451383818));
#20664=CARTESIAN_POINT('Ctrl Pts',(50.0835265683594,-6.08615941337703,-13.7725316059818));
#20665=CARTESIAN_POINT('Ctrl Pts',(50.0835265683582,-6.05089962282675,-13.6400817274103));
#20666=CARTESIAN_POINT('Ctrl Pts',(50.0835265683581,-6.04778978459125,-13.6283999309435));
#20667=CARTESIAN_POINT('Ctrl Pts',(50.083526568358,-6.0446832728305,-13.6167166878872));
#20668=CARTESIAN_POINT('Ctrl Pts',(50.0835265683579,-6.04158009539427,-13.6050320163313));
#20669=CARTESIAN_POINT('Ctrl Pts',(50.0835265683529,-5.90116651460509,-13.0763202016747));
#20670=CARTESIAN_POINT('Ctrl Pts',(50.0835265683567,-5.76761845986938,-12.5448358405602));
#20671=CARTESIAN_POINT('Ctrl Pts',(50.083526568357,-5.64153128315162,-12.0117275204805));
#20672=CARTESIAN_POINT('Ctrl Pts',(50.0835265683572,-5.55530241465321,-11.647143837792));
#20673=CARTESIAN_POINT('Ctrl Pts',(50.0835265683583,-5.4725636069766,-11.2817995154151));
#20674=CARTESIAN_POINT('Ctrl Pts',(50.0835265683438,-5.39351662111518,-10.916053821918));
#20675=CARTESIAN_POINT('Ctrl Pts',(50.0835265683434,-5.39159586118404,-10.9071665801668));
#20676=CARTESIAN_POINT('Ctrl Pts',(50.0835265683431,-5.38967730441898,-10.898279165744));
#20677=CARTESIAN_POINT('Ctrl Pts',(50.0835265683427,-5.38776095106819,-10.8893915765148));
#20678=CARTESIAN_POINT('Ctrl Pts',(50.0835265681882,-4.60335148320456,-7.25148777604795));
#20679=CARTESIAN_POINT('Ctrl Pts',(50.0835265682258,-4.18752460344888,-3.58097782223435));
#20680=CARTESIAN_POINT('Ctrl Pts',(50.0835265683469,-4.19081815795072,0.126611260712779));
#20681=CARTESIAN_POINT('Ctrl Pts',(50.0835265683471,-4.1908242862358,0.133509935943779));
#20682=CARTESIAN_POINT('Ctrl Pts',(50.0835265683474,-4.19083186535593,0.140408739492022));
#20683=CARTESIAN_POINT('Ctrl Pts',(50.0835265683476,-4.1908408956384,0.147307671387013));
#20684=CARTESIAN_POINT('Ctrl Pts',(50.0835265683765,-4.19204516267736,1.06734049527786));
#20685=CARTESIAN_POINT('Ctrl Pts',(50.0835265683618,-4.21882226363321,1.98963515495041));
#20686=CARTESIAN_POINT('Ctrl Pts',(50.083526568362,-4.27143022964226,2.91421541345035));
#20687=CARTESIAN_POINT('Ctrl Pts',(50.083526568362,-4.27205281679694,2.92515732654982));
#20688=CARTESIAN_POINT('Ctrl Pts',(50.083526568362,-4.27267902824778,2.93609967822935));
#20689=CARTESIAN_POINT('Ctrl Pts',(50.083526568362,-4.27330886465573,2.94704246860311));
#20690=CARTESIAN_POINT('Ctrl Pts',(50.0835265683621,-4.32629862648307,3.86768765251147));
#20691=CARTESIAN_POINT('Ctrl Pts',(50.0835265683618,-4.40442769523305,4.78252778718964));
#20692=CARTESIAN_POINT('Ctrl Pts',(50.0835265683619,-4.50641515619369,5.69168642424652));
#20693=CARTESIAN_POINT('Ctrl Pts',(50.0835265683619,-4.50797212337508,5.70556587714443));
#20694=CARTESIAN_POINT('Ctrl Pts',(50.0835265683619,-4.50953465011834,5.71944400116706));
#20695=CARTESIAN_POINT('Ctrl Pts',(50.0835265683619,-4.51110273180188,5.73332079645939));
#20696=CARTESIAN_POINT('Ctrl Pts',(50.083526568362,-4.63310585043406,6.81299178557852));
#20697=CARTESIAN_POINT('Ctrl Pts',(50.083526568362,-4.78875206538555,7.88473847945899));
#20698=CARTESIAN_POINT('Ctrl Pts',(50.0835265683619,-4.97573014435409,8.94910172276016));
#20699=CARTESIAN_POINT('Ctrl Pts',(50.0835265683619,-5.104928022985,9.68455410244992));
#20700=CARTESIAN_POINT('Ctrl Pts',(50.0835265683619,-5.24908423887366,10.4164815427171));
#20701=CARTESIAN_POINT('Ctrl Pts',(50.0835265683619,-5.40742232363258,11.1450662553477));
#20702=CARTESIAN_POINT('Ctrl Pts',(50.0835265683619,-5.4105998810796,11.159687625708));
#20703=CARTESIAN_POINT('Ctrl Pts',(50.0835265683619,-5.41378314936642,11.1743076488218));
#20704=CARTESIAN_POINT('Ctrl Pts',(50.0835265683619,-5.41697212217387,11.1889263261959));
#20705=CARTESIAN_POINT('Ctrl Pts',(50.083526568362,-5.65900900139522,12.2984557150021));
#20706=CARTESIAN_POINT('Ctrl Pts',(50.083526568362,-5.9337967445744,13.4002686430632));
#20707=CARTESIAN_POINT('Ctrl Pts',(50.083526568362,-6.23869144824832,14.4949862172741));
#20708=CARTESIAN_POINT('Ctrl Pts',(50.083526568362,-6.54852480772613,15.6074359240422));
#20709=CARTESIAN_POINT('Ctrl Pts',(50.083526568362,-6.88944821129976,16.7125585971452));
#20710=CARTESIAN_POINT('Ctrl Pts',(50.083526568362,-7.25863482935653,17.8110201816428));
#20711=CARTESIAN_POINT('Ctrl Pts',(50.083526568362,-7.63718691654914,18.9373473700475));
#20712=CARTESIAN_POINT('Ctrl Pts',(50.083526568362,-8.04545424387804,20.056671259519));
#20713=CARTESIAN_POINT('Ctrl Pts',(50.083526568362,-8.48033670889165,21.1697240178476));
#20714=CARTESIAN_POINT('Ctrl Pts',(50.083526568362,-8.54981664757972,21.3475533019114));
#20715=CARTESIAN_POINT('Ctrl Pts',(50.083526568362,-8.61997584800288,21.5252225401305));
#20716=CARTESIAN_POINT('Ctrl Pts',(50.083526568362,-8.69080155057986,21.7027347500389));
#20717=CARTESIAN_POINT('Ctrl Pts',(50.083526568362,-8.87385981233827,22.7876789472104));
#20718=CARTESIAN_POINT('Ctrl Pts',(50.083526568362,-8.87385981188611,22.717742516166));
#20719=CARTESIAN_POINT('Ctrl Pts',(50.083526568362,-8.87185808464315,22.6477745033947));
#20720=CARTESIAN_POINT('Ctrl Pts',(50.0835265683619,-8.86782837150229,22.5779796471447));
#20721=CARTESIAN_POINT('Ctrl Pts',(50.0835265683618,-8.86373626040434,22.507104054799));
#20722=CARTESIAN_POINT('Ctrl Pts',(50.0835265683618,-8.85755327620425,22.4364053802177));
#20723=CARTESIAN_POINT('Ctrl Pts',(50.0835265683588,-8.84920383564881,22.3660776681213));
#20724=CARTESIAN_POINT('Ctrl Pts',(50.0835265683569,-8.84406583764724,22.3228000806222));
#20725=CARTESIAN_POINT('Ctrl Pts',(50.0835265683538,-8.83810648050989,22.2796626723357));
#20726=CARTESIAN_POINT('Ctrl Pts',(50.0835265683476,-8.83129827231312,22.2367110515669));
#20727=CARTESIAN_POINT('Ctrl Pts',(50.0835265683475,-8.83124617212743,22.2363823619392));
#20728=CARTESIAN_POINT('Ctrl Pts',(50.0835265683475,-8.83119402657744,22.2360536803506));
#20729=CARTESIAN_POINT('Ctrl Pts',(50.0835265683474,-8.83114183558509,22.235725006798));
#20730=CARTESIAN_POINT('Ctrl Pts',(50.0835265683309,-8.81326914157238,22.1231714497214));
#20731=CARTESIAN_POINT('Ctrl Pts',(50.0835265683519,-8.79011900704274,22.011837783367));
#20732=CARTESIAN_POINT('Ctrl Pts',(50.0835265683584,-8.75874571255292,21.9024044661432));
#20733=CARTESIAN_POINT('Ctrl Pts',(50.0835265683624,-8.73944301755183,21.8350746565177));
#20734=CARTESIAN_POINT('Ctrl Pts',(50.083526568362,-8.71702701275813,21.7684643500544));
#20735=CARTESIAN_POINT('Ctrl Pts',(50.083526568362,-8.69080155058071,21.7027347500411));
#20736=CARTESIAN_POINT('Origin',(44.4585265683622,16.4830954176946,-44.2925682080604));
#20737=CARTESIAN_POINT('Origin',(44.4585265683622,-8.87385981233827,-44.2925682080604));
#20738=CARTESIAN_POINT('Origin',(44.4585265683622,-14.4544045823054,-44.2925682080604));
#20739=CARTESIAN_POINT('Origin',(50.0835265683621,16.4830954176946,0.0824317919395974));
#20740=CARTESIAN_POINT('',(50.0835265683622,16.1705954176946,-44.2925682080604));
#20741=CARTESIAN_POINT('',(50.0835265683619,16.1705954176946,36.6697170232579));
#20742=CARTESIAN_POINT('',(50.0835265683619,16.1705954176946,44.4574317919394));
#20743=CARTESIAN_POINT('',(50.0835265683619,13.4386401876617,36.6697170232579));
#20744=CARTESIAN_POINT('',(50.0835265683619,16.4830954176946,36.6697170232579));
#20745=CARTESIAN_POINT('',(50.083526568362,13.4386401876617,11.0309447204208));
#20746=CARTESIAN_POINT('',(50.0835265683621,13.4386401876617,0.0824317919395974));
#20747=CARTESIAN_POINT('',(50.083526568362,13.2555819259033,8.74809679815803));
#20748=CARTESIAN_POINT('Ctrl Pts',(50.083526568362,13.2555819259033,8.74809679815823));
#20749=CARTESIAN_POINT('Ctrl Pts',(50.083526568362,13.2969611279801,8.98893971344353));
#20750=CARTESIAN_POINT('Ctrl Pts',(50.083526568362,13.3294628820991,9.23096941458519));
#20751=CARTESIAN_POINT('Ctrl Pts',(50.083526568362,13.3553162053205,9.47374987915283));
#20752=CARTESIAN_POINT('Ctrl Pts',(50.083526568362,13.3699153107393,9.61084550765334));
#20753=CARTESIAN_POINT('Ctrl Pts',(50.083526568362,13.3823932020092,9.74818076138043));
#20754=CARTESIAN_POINT('Ctrl Pts',(50.083526568362,13.3931443825075,9.88567820112658));
#20755=CARTESIAN_POINT('Ctrl Pts',(50.083526568362,13.3931495855304,9.88574474287337));
#20756=CARTESIAN_POINT('Ctrl Pts',(50.083526568362,13.3931547881236,9.88581128464174));
#20757=CARTESIAN_POINT('Ctrl Pts',(50.083526568362,13.3931599902869,9.8858778264317));
#20758=CARTESIAN_POINT('Ctrl Pts',(50.083526568362,13.4229505456848,10.2669340808595));
#20759=CARTESIAN_POINT('Ctrl Pts',(50.083526568362,13.4386401851025,10.6486001469402));
#20760=CARTESIAN_POINT('Ctrl Pts',(50.083526568362,13.4386401876617,11.0309447204208));
#20761=CARTESIAN_POINT('',(50.0835265683621,13.2555819259033,-8.58323321427883));
#20762=CARTESIAN_POINT('Ctrl Pts',(50.083526568362,13.2555819259033,8.74809679815803));
#20763=CARTESIAN_POINT('Ctrl Pts',(50.083526568362,13.0482120855562,7.54112464899445));
#20764=CARTESIAN_POINT('Ctrl Pts',(50.083526568362,12.8826695792778,6.33137948099875));
#20765=CARTESIAN_POINT('Ctrl Pts',(50.083526568362,12.760436564522,5.11876132513915));
#20766=CARTESIAN_POINT('Ctrl Pts',(50.083526568362,12.6392785940108,3.91680819437184));
#20767=CARTESIAN_POINT('Ctrl Pts',(50.083526568362,12.560671682904,2.7120323854556));
#20768=CARTESIAN_POINT('Ctrl Pts',(50.083526568362,12.5260083297323,1.50434227373321));
#20769=CARTESIAN_POINT('Ctrl Pts',(50.083526568362,12.5125314172724,1.03479930038698));
#20770=CARTESIAN_POINT('Ctrl Pts',(50.083526568362,12.5056965050864,0.564815860197846));
#20771=CARTESIAN_POINT('Ctrl Pts',(50.0835265683621,12.5055833090018,0.0943868073395787));
#20772=CARTESIAN_POINT('Ctrl Pts',(50.0835265683621,12.5055832718468,0.0942323956936116));
#20773=CARTESIAN_POINT('Ctrl Pts',(50.083526568362,12.5055832354158,0.0940779840217097));
#20774=CARTESIAN_POINT('Ctrl Pts',(50.083526568362,12.505583199709,0.0939235723238649));
#20775=CARTESIAN_POINT('Ctrl Pts',(50.083526568362,12.5054760332769,-0.369510401693673));
#20776=CARTESIAN_POINT('Ctrl Pts',(50.0835265683624,12.5119501585697,-0.833607667675453));
#20777=CARTESIAN_POINT('Ctrl Pts',(50.0835265683571,12.5248910213244,-1.2978410246897));
#20778=CARTESIAN_POINT('Ctrl Pts',(50.0835265683517,12.537901838647,-1.76458389320593));
#20779=CARTESIAN_POINT('Ctrl Pts',(50.0835265683393,12.5574495854738,-2.23146564927433));
#20780=CARTESIAN_POINT('Ctrl Pts',(50.0835265683302,12.5834701483639,-2.69795234473062));
#20781=CARTESIAN_POINT('Ctrl Pts',(50.0835265683213,12.6088446209642,-3.15285618067797));
#20782=CARTESIAN_POINT('Ctrl Pts',(50.0835265683192,12.6403747667627,-3.60738548981518));
#20783=CARTESIAN_POINT('Ctrl Pts',(50.0835265683316,12.6780474220394,-4.06102862482723));
#20784=CARTESIAN_POINT('Ctrl Pts',(50.0835265683335,12.6835738954316,-4.12757680670609));
#20785=CARTESIAN_POINT('Ctrl Pts',(50.0835265683355,12.6892326346535,-4.19410587081538));
#20786=CARTESIAN_POINT('Ctrl Pts',(50.0835265683378,12.6950236788078,-4.26061414818264));
#20787=CARTESIAN_POINT('Ctrl Pts',(50.083526568338,12.6955171094319,-4.26628104001408));
#20788=CARTESIAN_POINT('Ctrl Pts',(50.0835265683381,12.6960114970034,-4.27194774229855));
#20789=CARTESIAN_POINT('Ctrl Pts',(50.0835265683383,12.6965068414371,-4.27761425314022));
#20790=CARTESIAN_POINT('Ctrl Pts',(50.0835265683662,12.7706053471226,-5.12526683034168));
#20791=CARTESIAN_POINT('Ctrl Pts',(50.0835265683616,12.865971940895,-5.97068200817664));
#20792=CARTESIAN_POINT('Ctrl Pts',(50.083526568362,12.9818931825585,-6.81390647641708));
#20793=CARTESIAN_POINT('Ctrl Pts',(50.0835265683622,13.0631188030526,-7.40475099866104));
#20794=CARTESIAN_POINT('Ctrl Pts',(50.0835265683621,13.1544351593156,-7.99452016890981));
#20795=CARTESIAN_POINT('Ctrl Pts',(50.0835265683621,13.2555819259033,-8.58323321427884));
#20796=CARTESIAN_POINT('',(50.0835265683621,13.4386401876617,-10.8660811365416));
#20797=CARTESIAN_POINT('Ctrl Pts',(50.0835265683621,13.4386401876617,-10.8660811365416));
#20798=CARTESIAN_POINT('Ctrl Pts',(50.0835265683621,13.4386401861139,-10.6249936669031));
#20799=CARTESIAN_POINT('Ctrl Pts',(50.0835265683622,13.4323889945138,-10.3840575949856));
#20800=CARTESIAN_POINT('Ctrl Pts',(50.083526568362,13.4203066131559,-10.1434070400552));
#20801=CARTESIAN_POINT('Ctrl Pts',(50.0835265683619,13.4132400183933,-10.002658300158));
#20802=CARTESIAN_POINT('Ctrl Pts',(50.0835265683617,13.4041776979157,-9.86200706428455));
#20803=CARTESIAN_POINT('Ctrl Pts',(50.0835265683608,13.393195553816,-9.72147949723203));
#20804=CARTESIAN_POINT('Ctrl Pts',(50.0835265683608,13.3931761734939,-9.72123150654036));
#20805=CARTESIAN_POINT('Ctrl Pts',(50.0835265683608,13.3931567875857,-9.72098351656411));
#20806=CARTESIAN_POINT('Ctrl Pts',(50.0835265683608,13.3931373960889,-9.72073552730331));
#20807=CARTESIAN_POINT('Ctrl Pts',(50.0835265683585,13.3633415593949,-9.33968977198554));
#20808=CARTESIAN_POINT('Ctrl Pts',(50.0835265683621,13.320346515891,-8.96018808653365));
#20809=CARTESIAN_POINT('Ctrl Pts',(50.0835265683621,13.2555819259033,-8.58323321427883));
#20810=CARTESIAN_POINT('',(50.0835265683622,13.4386401876617,-44.2925682080604));
#20811=CARTESIAN_POINT('',(50.0835265683621,13.4386401876617,0.0824317919395974));
#20812=CARTESIAN_POINT('',(50.0835265683622,16.4830954176946,-44.2925682080604));
#20813=CARTESIAN_POINT('Origin',(44.4585265683622,16.4830954176946,-44.2925682080604));
#20814=CARTESIAN_POINT('Origin',(44.4585265683622,13.4386401876617,-44.2925682080604));
#20815=CARTESIAN_POINT('Origin',(44.4585265683622,16.1705954176946,-44.2925682080604));
#20816=CARTESIAN_POINT('Origin',(0.0835265683620477,16.4830954176946,0.0824317919394229));
#20817=CARTESIAN_POINT('',(22.6771142305789,16.3915662868157,-48.242741818912));
#20818=CARTESIAN_POINT('',(4.30427685447661,11.5746245485365,-48.2627017315535));
#20819=CARTESIAN_POINT('Ctrl Pts',(22.677114230578,16.3915662868154,-48.2427418189112));
#20820=CARTESIAN_POINT('Ctrl Pts',(19.7455070706072,15.1541680928392,-48.2474043029498));
#20821=CARTESIAN_POINT('Ctrl Pts',(16.756896605017,14.0894359483377,-48.2517517721786));
#20822=CARTESIAN_POINT('Ctrl Pts',(12.1565558613288,12.8480220597895,-48.257033362324));
#20823=CARTESIAN_POINT('Ctrl Pts',(10.6007498763966,12.4934998941785,-48.2585854301897));
#20824=CARTESIAN_POINT('Ctrl Pts',(7.46946850957225,11.9258476364964,-48.261105456389));
#20825=CARTESIAN_POINT('Ctrl Pts',(5.89096210505037,11.7120008366799,-48.2620757256809));
#20826=CARTESIAN_POINT('Ctrl Pts',(4.30427685533896,11.5746245485739,-48.2627017315157));
#20827=CARTESIAN_POINT('',(48.4286600918519,11.5746245485739,-4.13831849464002));
#20828=CARTESIAN_POINT('Origin',(0.0835265683620477,11.5746245485739,0.0824317919394229));
#20829=CARTESIAN_POINT('',(48.4087001792128,16.3915662868156,-22.5111558702767));
#20830=CARTESIAN_POINT('Ctrl Pts',(48.4286600918172,11.5746245485739,-4.13831849503729));
#20831=CARTESIAN_POINT('Ctrl Pts',(48.4280346394369,11.7118793817134,-5.72360094950246));
#20832=CARTESIAN_POINT('Ctrl Pts',(48.4270679171629,11.9249456441311,-7.29678813530604));
#20833=CARTESIAN_POINT('Ctrl Pts',(48.4245562772761,12.4906656417943,-10.4208921803695));
#20834=CARTESIAN_POINT('Ctrl Pts',(48.4230091974657,12.8439804579761,-11.9740784049424));
#20835=CARTESIAN_POINT('Ctrl Pts',(48.4177256478359,14.0856585112706,-16.5800021649963));
#20836=CARTESIAN_POINT('Ctrl Pts',(48.4133613504756,15.1545164964592,-19.5803741378453));
#20837=CARTESIAN_POINT('Ctrl Pts',(48.4087001792127,16.3915662868154,-22.5111558702763));
#20838=CARTESIAN_POINT('Origin',(0.0835265683620477,16.3915662868154,0.0824317919394229));
#20839=CARTESIAN_POINT('Origin',(48.5210265683621,-85.4775827009602,0.0824317919395913));
#20840=CARTESIAN_POINT('',(48.521026568362,11.7955954176946,4.28396341998253));
#20841=CARTESIAN_POINT('',(48.5210265683621,11.6131136241746,0.0824317919395203));
#20842=CARTESIAN_POINT('Origin',(48.5210265683762,84.3502669988373,0.0808847077731101));
#20843=CARTESIAN_POINT('',(48.5210265682489,16.1706033824536,21.518168778977));
#20844=CARTESIAN_POINT('Ctrl Pts',(48.5210265683619,11.7955954176945,4.28396341998253));
#20845=CARTESIAN_POINT('Ctrl Pts',(48.5210265683581,11.9012754513054,5.49904346048471));
#20846=CARTESIAN_POINT('Ctrl Pts',(48.5210265682208,12.0520583741837,6.7088076511187));
#20847=CARTESIAN_POINT('Ctrl Pts',(48.5210265682647,12.245534037766,7.91354042332108));
#20848=CARTESIAN_POINT('Ctrl Pts',(48.5210265682742,12.2874241519058,8.17438146348642));
#20849=CARTESIAN_POINT('Ctrl Pts',(48.5210265682907,12.3313158156439,8.43498661765798));
#20850=CARTESIAN_POINT('Ctrl Pts',(48.5210265683094,12.3771848834538,8.69535873608156));
#20851=CARTESIAN_POINT('Ctrl Pts',(48.521026568315,12.3910255799873,8.77392435009892));
#20852=CARTESIAN_POINT('Ctrl Pts',(48.5210265683122,12.4050450140625,8.85246436981573));
#20853=CARTESIAN_POINT('Ctrl Pts',(48.5210265682998,12.4192427232413,8.93097996771382));
#20854=CARTESIAN_POINT('Ctrl Pts',(48.521026568213,12.5191317203718,9.48338206543068));
#20855=CARTESIAN_POINT('Ctrl Pts',(48.5210265673562,12.6280707956221,10.0352897380736));
#20856=CARTESIAN_POINT('Ctrl Pts',(48.5210265620527,12.7454889374133,10.5858637901934));
#20857=CARTESIAN_POINT('Ctrl Pts',(48.5210265566114,12.8659559514214,11.150734014142));
#20858=CARTESIAN_POINT('Ctrl Pts',(48.5210265462836,12.9953485173926,11.714201755527));
#20859=CARTESIAN_POINT('Ctrl Pts',(48.5210265443164,13.1331031832496,12.2753514078195));
#20860=CARTESIAN_POINT('Ctrl Pts',(48.5210265433988,13.1973553945139,12.5370855987138));
#20861=CARTESIAN_POINT('Ctrl Pts',(48.5210265445818,13.2634275010315,12.7983152304055));
#20862=CARTESIAN_POINT('Ctrl Pts',(48.5210265481732,13.3312657045515,13.0589454818311));
#20863=CARTESIAN_POINT('Ctrl Pts',(48.521026550869,13.382187770071,13.2545849600426));
#20864=CARTESIAN_POINT('Ctrl Pts',(48.521026553119,13.4341067575158,13.4499116170473));
#20865=CARTESIAN_POINT('Ctrl Pts',(48.5210265550302,13.4869947668864,13.6448649932951));
#20866=CARTESIAN_POINT('Ctrl Pts',(48.5210265629102,13.705058467528,14.4486814950525));
#20867=CARTESIAN_POINT('Ctrl Pts',(48.5210265653827,13.9395350033909,15.2473465102858));
#20868=CARTESIAN_POINT('Ctrl Pts',(48.5210265667497,14.1892982824036,16.0411553774744));
#20869=CARTESIAN_POINT('Ctrl Pts',(48.5210265681412,14.4435598429467,16.8492608849858));
#20870=CARTESIAN_POINT('Ctrl Pts',(48.5210265682269,14.7136635664295,17.6523337933097));
#20871=CARTESIAN_POINT('Ctrl Pts',(48.5210265683088,14.998370752621,18.4507061044753));
#20872=CARTESIAN_POINT('Ctrl Pts',(48.5210265683931,15.2915959449578,19.2729645013546));
#20873=CARTESIAN_POINT('Ctrl Pts',(48.5210265683619,15.600311376782,20.0902368738228));
#20874=CARTESIAN_POINT('Ctrl Pts',(48.521026568362,15.9231126709056,20.9029067079027));
#20875=CARTESIAN_POINT('Ctrl Pts',(48.521026568362,16.004689947692,21.1082819439924));
#20876=CARTESIAN_POINT('Ctrl Pts',(48.521026568362,16.0871665859128,21.3133633340306));
#20877=CARTESIAN_POINT('Ctrl Pts',(48.521026568362,16.1705194395551,21.5181572619665));
#20878=CARTESIAN_POINT('',(48.5210265682481,16.1706033612914,-21.3533050824651));
#20879=CARTESIAN_POINT('',(48.5210265683621,16.1705954176946,0.0824317919395913));
#20880=CARTESIAN_POINT('',(48.5210265683621,11.7955954176946,-4.11909983610349));
#20881=CARTESIAN_POINT('Ctrl Pts',(48.5210265683621,16.1705196413332,-21.3532935961081));
#20882=CARTESIAN_POINT('Ctrl Pts',(48.5210265683621,15.8435202227035,-20.5498711716006));
#20883=CARTESIAN_POINT('Ctrl Pts',(48.5210265683753,15.5300086684673,-19.7420199101728));
#20884=CARTESIAN_POINT('Ctrl Pts',(48.5210265683489,15.2313679633776,-18.9293681492881));
#20885=CARTESIAN_POINT('Ctrl Pts',(48.521026568323,14.9390610384528,-18.1339516731999));
#20886=CARTESIAN_POINT('Ctrl Pts',(48.5210265683458,14.661001060326,-17.3339360822784));
#20887=CARTESIAN_POINT('Ctrl Pts',(48.5210265675901,14.3984390227961,-16.5289914655286));
#20888=CARTESIAN_POINT('Ctrl Pts',(48.5210265668539,14.1426624798295,-15.7448493508167));
#20889=CARTESIAN_POINT('Ctrl Pts',(48.5210265655117,13.9015932979829,-14.9560296549517));
#20890=CARTESIAN_POINT('Ctrl Pts',(48.5210265604243,13.6763418780025,-14.162246017455));
#20891=CARTESIAN_POINT('Ctrl Pts',(48.5210265589699,13.6119483517376,-13.9353239074224));
#20892=CARTESIAN_POINT('Ctrl Pts',(48.521026557187,13.5488472151597,-13.7079962448028));
#20893=CARTESIAN_POINT('Ctrl Pts',(48.5210265549389,13.4870636734946,-13.4802566325191));
#20894=CARTESIAN_POINT('Ctrl Pts',(48.5210265530145,13.43417513047,-13.2853047738518));
#20895=CARTESIAN_POINT('Ctrl Pts',(48.5210265507489,13.3822549873809,-13.0899772433496));
#20896=CARTESIAN_POINT('Ctrl Pts',(48.5210265480343,13.3313312754876,-12.8943348440505));
#20897=CARTESIAN_POINT('Ctrl Pts',(48.521026540269,13.1856558716782,-12.334668542036));
#20898=CARTESIAN_POINT('Ctrl Pts',(48.521026545501,13.0481153498219,-11.7722163782289));
#20899=CARTESIAN_POINT('Ctrl Pts',(48.521026552699,12.9192577967369,-11.207918578878));
#20900=CARTESIAN_POINT('Ctrl Pts',(48.5210265597492,12.7930466642987,-10.6552100834632));
#20901=CARTESIAN_POINT('Ctrl Pts',(48.5210265658216,12.6751650327471,-10.1007297054743));
#20902=CARTESIAN_POINT('Ctrl Pts',(48.5210265674002,12.5661734819284,-9.54534356437002));
#20903=CARTESIAN_POINT('Ctrl Pts',(48.5210265681379,12.5152460170547,-9.28583346491732));
#20904=CARTESIAN_POINT('Ctrl Pts',(48.5210265682585,12.4662602454938,-9.02612547553568));
#20905=CARTESIAN_POINT('Ctrl Pts',(48.5210265682996,12.4192773203291,-8.76630779101686));
#20906=CARTESIAN_POINT('Ctrl Pts',(48.521026568312,12.4050773744288,-8.68778145296586));
#20907=CARTESIAN_POINT('Ctrl Pts',(48.5210265683148,12.3910557938721,-8.60923092228166));
#20908=CARTESIAN_POINT('Ctrl Pts',(48.5210265683092,12.3772130393344,-8.53065503615693));
#20909=CARTESIAN_POINT('Ctrl Pts',(48.5210265682229,12.1658567976611,-7.33092965402482));
#20910=CARTESIAN_POINT('Ctrl Pts',(48.5210265682964,11.996481850192,-6.12627208137987));
#20911=CARTESIAN_POINT('Ctrl Pts',(48.521026568344,11.8714667055606,-4.91640245756147));
#20912=CARTESIAN_POINT('Ctrl Pts',(48.5210265683544,11.8440311392596,-4.65088696039834));
#20913=CARTESIAN_POINT('Ctrl Pts',(48.5210265683611,11.8187322178908,-4.38512041878988));
#20914=CARTESIAN_POINT('Ctrl Pts',(48.521026568362,11.7955954176946,-4.11909983610349));
#20915=CARTESIAN_POINT('Origin',(48.5210265743749,84.3502669996413,0.0839788824233628));
#20916=CARTESIAN_POINT('Origin',(41.1841082248303,16.4855954176946,-39.6923246498037));
#20917=CARTESIAN_POINT('',(36.0907279647213,-3.61941807409669,-34.5989443896948));
#20918=CARTESIAN_POINT('',(39.3651742963362,-8.24885981233827,-37.8733907213097));
#20919=CARTESIAN_POINT('Ctrl Pts',(36.0907279647213,-3.61941807409669,-34.5989443896948));
#20920=CARTESIAN_POINT('Ctrl Pts',(36.637239178152,-4.3920600802535,-35.1454556031255));
#20921=CARTESIAN_POINT('Ctrl Pts',(37.1837464394694,-5.16470767732064,-35.6919628644429));
#20922=CARTESIAN_POINT('Ctrl Pts',(38.2752282249955,-6.70785538323104,-36.783444649969));
#20923=CARTESIAN_POINT('Ctrl Pts',(38.8202027672248,-7.4783554666459,-37.3284191921982));
#20924=CARTESIAN_POINT('Ctrl Pts',(39.3651742963362,-8.24885981233827,-37.8733907213097));
#20925=CARTESIAN_POINT('',(40.5211956174679,-8.24885981233827,-39.0294120424414));
#20926=CARTESIAN_POINT('',(36.712778241545,12.8136401876617,-35.2209946665185));
#20927=CARTESIAN_POINT('',(36.6259848372153,12.8136401876617,-35.1342012621888));
#20928=CARTESIAN_POINT('',(36.0907279647213,11.9341984494202,-34.5989443896948));
#20929=CARTESIAN_POINT('',(36.712778241545,12.8136401876617,-35.2209946665185));
#20930=CARTESIAN_POINT('',(36.0907279647213,-3.74885981233827,-34.5989443896948));
#20931=CARTESIAN_POINT('Origin',(39.8582830101055,16.4855954176946,-41.0181498645285));
#20932=CARTESIAN_POINT('',(38.0393490816115,-8.24885981233827,-39.1992159360345));
#20933=CARTESIAN_POINT('',(37.9522314572197,-8.24885981233827,-39.1120983116427));
#20934=CARTESIAN_POINT('Ctrl Pts',(38.0393490816115,-8.24885981233827,-39.1992159360345));
#20935=CARTESIAN_POINT('Ctrl Pts',(37.4943775525,-7.4783554666459,-38.654244406923));
#20936=CARTESIAN_POINT('Ctrl Pts',(36.9494030102707,-6.70785538323103,-38.1092698646938));
#20937=CARTESIAN_POINT('Ctrl Pts',(35.8579212247446,-5.16470767732064,-37.0177880791676));
#20938=CARTESIAN_POINT('Ctrl Pts',(35.3114139634272,-4.39206008025349,-36.4712808178503));
#20939=CARTESIAN_POINT('Ctrl Pts',(34.7649027499965,-3.61941807409669,-35.9247696044196));
#20940=CARTESIAN_POINT('',(35.3869530268202,12.8136401876617,-36.5468198812432));
#20941=CARTESIAN_POINT('',(34.7649027499965,11.9341984494202,-35.9247696044196));
#20942=CARTESIAN_POINT('',(39.1953704027431,12.8136401876617,-40.3552372571661));
#20943=CARTESIAN_POINT('Origin',(0.0835265683620477,-11.0169045823054,0.0824317919394229));
#20944=CARTESIAN_POINT('',(19.5475193794832,-11.3294045823054,-9.90098490018674));
#20945=CARTESIAN_POINT('',(19.5475193794832,-11.0169045823054,-9.90098490018674));
#20946=CARTESIAN_POINT('Origin',(0.0835265683620477,-14.4544045823054,0.0824317919394229));
#20947=CARTESIAN_POINT('Origin',(0.0835265683620477,-11.3294045823054,0.0824317919394229));
#20948=CARTESIAN_POINT('Origin',(0.0835265683620477,-13.2044045823054,0.0824317919394229));
#20949=CARTESIAN_POINT('',(34.7488729746945,-13.2044045823054,-34.1940362076806));
#20950=CARTESIAN_POINT('',(37.084741276154,-13.2044045823054,-41.2777797274919));
#20951=CARTESIAN_POINT('',(37.1711692825102,-13.2044045823054,-41.5398809039896));
#20952=CARTESIAN_POINT('',(38.3461436957037,-13.2044045823054,-40.1137013224621));
#20953=CARTESIAN_POINT('Origin',(0.0835265683620477,-13.2044045823054,0.0824317919394229));
#20954=CARTESIAN_POINT('',(35.9713494567465,-13.2044045823054,-32.9119111827578));
#20955=CARTESIAN_POINT('',(22.6388808156566,-13.2044045823054,7.52007219592841));
#20956=CARTESIAN_POINT('Origin',(0.0835265683620477,-13.2044045823054,0.0824317919394229));
#20957=CARTESIAN_POINT('Origin',(22.9356617925947,16.4855954176946,7.61793588545459));
#20958=CARTESIAN_POINT('',(36.2681304336846,-12.8919045823054,-32.8140474932316));
#20959=CARTESIAN_POINT('',(38.3305777332763,-12.8919045823054,-39.0686157342182));
#20960=CARTESIAN_POINT('',(22.9356617925947,-12.8919045823054,7.61793588545459));
#20961=CARTESIAN_POINT('',(36.2681294096903,-7.07886051013668,-32.8140443877542));
#20962=CARTESIAN_POINT('Ctrl Pts',(38.3305777332763,-12.8919045823054,-39.0686157342182));
#20963=CARTESIAN_POINT('Ctrl Pts',(37.7859832182751,-11.3339023356853,-37.4170809006171));
#20964=CARTESIAN_POINT('Ctrl Pts',(37.2389106772517,-9.78474033348405,-35.7580312166432));
#20965=CARTESIAN_POINT('Ctrl Pts',(36.688444321157,-8.24794399815022,-34.0886894646172));
#20966=CARTESIAN_POINT('Ctrl Pts',(36.5485654401618,-7.85742902966216,-33.6644934103323));
#20967=CARTESIAN_POINT('Ctrl Pts',(36.4084673618567,-7.46771271895524,-33.2396326192889));
#20968=CARTESIAN_POINT('Ctrl Pts',(36.2681349390778,-7.07885337126685,-32.8140611562666));
#20969=CARTESIAN_POINT('',(36.2681304336846,16.4855954176946,-32.8140474932316));
#20970=CARTESIAN_POINT('Origin',(0.0835265683620477,-13.2044045823054,0.0824317919394229));
#20971=CARTESIAN_POINT('',(28.0161439142367,-13.2044045823054,-39.8716842439453));
#20972=CARTESIAN_POINT('',(30.2097727145137,-13.2044045823054,-46.5240729034966));
#20973=CARTESIAN_POINT('',(30.2768410701833,-13.2044045823054,-46.7274640919305));
#20974=CARTESIAN_POINT('',(31.5582959274376,-13.2044045823054,-45.624196617704));
#20975=CARTESIAN_POINT('Origin',(0.0835265683620477,-13.2044045823054,0.0824317919394229));
#20976=CARTESIAN_POINT('',(29.344152791651,-13.2044045823054,-38.9095962781799));
#20977=CARTESIAN_POINT('',(14.8778438489026,-13.2044045823054,4.96086600976507));
#20978=CARTESIAN_POINT('Origin',(0.0835265683620477,-13.2044045823054,0.0824317919394229));
#20979=CARTESIAN_POINT('Origin',(13.0971579872741,16.4855954176946,4.37368387260805));
#20980=CARTESIAN_POINT('',(27.7193629372986,-12.8919045823054,-39.9695479334715));
#20981=CARTESIAN_POINT('',(27.719362975691,-6.59535001059349,-39.9695480499001));
#20982=CARTESIAN_POINT('',(27.7193629372986,-6.01690458230549,-39.9695479334715));
#20983=CARTESIAN_POINT('',(29.7611081292079,-12.8919045823054,-46.1613350574533));
#20984=CARTESIAN_POINT('Ctrl Pts',(27.7193631233119,-6.59534981976386,-39.9695484975747));
#20985=CARTESIAN_POINT('Ctrl Pts',(28.4014849791012,-8.68909917313932,-42.0381481153913));
#20986=CARTESIAN_POINT('Ctrl Pts',(29.0818842509084,-10.7885698299844,-44.101523832908));
#20987=CARTESIAN_POINT('Ctrl Pts',(29.761108129208,-12.8919045823054,-46.1613350574534));
#20988=CARTESIAN_POINT('',(27.6463789144421,-12.8919045823054,-39.7482169198025));
#20989=CARTESIAN_POINT('Origin',(0.0835265683620477,15.5455954176946,0.0824317919394229));
#20990=CARTESIAN_POINT('Origin',(0.0835265683620477,16.1705954176946,0.0824317919394229));
#20991=CARTESIAN_POINT('',(46.7874371828873,15.5455954176946,-28.9648526475816));
#20992=CARTESIAN_POINT('Origin',(0.0835265683620477,15.8580954176946,0.0824317919394229));
#20993=CARTESIAN_POINT('Origin',(42.8347289362664,15.5455954176946,-48.3550682080604));
#20994=CARTESIAN_POINT('',(40.1623618543411,15.8580954176946,-48.3550682080604));
#20995=CARTESIAN_POINT('',(40.1623618543411,16.1705954176946,-48.3550682080604));
#20996=CARTESIAN_POINT('',(40.1623618543411,16.4830954176946,-48.3550682080604));
#20997=CARTESIAN_POINT('',(29.6259351744661,16.1705954176946,-48.3550682080605));
#20998=CARTESIAN_POINT('',(42.8347289362664,15.8580954176946,-48.3550682080604));
#20999=CARTESIAN_POINT('Origin',(48.5210265683621,15.5455954176946,-25.9715236419289));
#21000=CARTESIAN_POINT('',(48.5210265683621,16.4830954176946,-29.4599768141643));
#21001=CARTESIAN_POINT('',(48.5210265683622,16.1705954176946,-39.9964034940393));
#21002=CARTESIAN_POINT('',(48.5210265683622,16.1705954176946,-39.9964034940393));
#21003=CARTESIAN_POINT('',(48.5210265683622,15.8580954176946,-39.9964034940393));
#21004=CARTESIAN_POINT('',(48.5210265683622,15.5455954176946,-39.9964034940393));
#21005=CARTESIAN_POINT('',(48.5210265683621,15.8580954176946,-25.9715236419289));
#21006=CARTESIAN_POINT('Origin',(0.0835265683620477,15.5455954176946,0.0824317919394229));
#21007=CARTESIAN_POINT('',(40.1623618543411,15.5455954176946,-48.0425682080604));
#21008=CARTESIAN_POINT('Origin',(40.1623618543411,15.5455954176946,-47.4175682080604));
#21009=CARTESIAN_POINT('',(29.6259351744661,15.5455954176946,-48.0425682080605));
#21010=CARTESIAN_POINT('',(0.0835265683622157,15.5455954176946,-48.0425682080606));
#21011=CARTESIAN_POINT('',(29.2958523967443,15.5455954176946,-46.8868419510772));
#21012=CARTESIAN_POINT('Origin',(29.6259351744661,15.5455954176946,-47.4175682080605));
#21013=CARTESIAN_POINT('Origin',(0.0835265683620477,15.5455954176946,0.0824317919394229));
#21014=CARTESIAN_POINT('',(48.2085265683622,15.5455954176946,-39.9964034940393));
#21015=CARTESIAN_POINT('',(48.208526568362,15.5455954176946,0.0824317919396409));
#21016=CARTESIAN_POINT('Origin',(47.5835265683622,15.5455954176946,-39.9964034940393));
#21017=CARTESIAN_POINT('Origin',(47.5835265683621,15.5455954176946,-29.4599768141643));
#21018=CARTESIAN_POINT('Origin',(40.1623618543411,15.5455954176946,-47.4175682080604));
#21019=CARTESIAN_POINT('Origin',(40.1623618543411,15.8580954176946,-47.4175682080604));
#21020=CARTESIAN_POINT('Origin',(40.1623618543411,16.1705954176946,-47.4175682080604));
#21021=CARTESIAN_POINT('Origin',(47.5835265683622,15.5455954176946,-39.9964034940393));
#21022=CARTESIAN_POINT('Origin',(47.5835265683622,15.8580954176946,-39.9964034940393));
#21023=CARTESIAN_POINT('Origin',(47.5835265683622,16.1705954176946,-39.9964034940393));
#21024=CARTESIAN_POINT('Origin',(0.0835265683620477,-6.01690458230549,0.0824317919394229));
#21025=CARTESIAN_POINT('',(45.9721485234461,-13.2959337131846,31.6825266249535));
#21026=CARTESIAN_POINT('',(46.8756079148278,-13.2959337131846,30.3286338949778));
#21027=CARTESIAN_POINT('Origin',(0.0835265683620477,-13.2959337131846,0.0824317919394229));
#21028=CARTESIAN_POINT('',(46.611780876039,-12.6709337131846,29.5815526781396));
#21029=CARTESIAN_POINT('Ctrl Pts',(46.8756079148278,-13.2959337131846,30.3286338949778));
#21030=CARTESIAN_POINT('Ctrl Pts',(46.8978549415453,-13.2959337131846,30.2942168570853));
#21031=CARTESIAN_POINT('Ctrl Pts',(46.9164623589588,-13.2919430659178,30.2579882035445));
#21032=CARTESIAN_POINT('Ctrl Pts',(46.9310469253967,-13.2842290832261,30.2210590246762));
#21033=CARTESIAN_POINT('Ctrl Pts',(46.9456755093586,-13.2764918190456,30.1840183902481));
#21034=CARTESIAN_POINT('Ctrl Pts',(46.9562575681815,-13.2650083398673,30.1462712757252));
#21035=CARTESIAN_POINT('Ctrl Pts',(46.96237146099,-13.2500137812688,30.1089284559708));
#21036=CARTESIAN_POINT('Ctrl Pts',(46.964608839739,-13.2445265233453,30.095262853063));
#21037=CARTESIAN_POINT('Ctrl Pts',(46.9662474594096,-13.2385687578732,30.0816514214285));
#21038=CARTESIAN_POINT('Ctrl Pts',(46.967265227178,-13.232151003965,30.0681489513688));
#21039=CARTESIAN_POINT('Ctrl Pts',(46.9672860185445,-13.2320198995247,30.0678731175172));
#21040=CARTESIAN_POINT('Ctrl Pts',(46.9673065509185,-13.2318886036912,30.0675973300348));
#21041=CARTESIAN_POINT('Ctrl Pts',(46.9673268241115,-13.2317571165656,30.0673215894106));
#21042=CARTESIAN_POINT('Ctrl Pts',(46.9707862023296,-13.209320409148,30.0202697455207));
#21043=CARTESIAN_POINT('Ctrl Pts',(46.9670157628007,-13.1821368365731,29.9756324601365));
#21044=CARTESIAN_POINT('Ctrl Pts',(46.9577324696803,-13.1520894282891,29.93427208866));
#21045=CARTESIAN_POINT('Ctrl Pts',(46.949874341568,-13.1266548782133,29.8992613340045));
#21046=CARTESIAN_POINT('Ctrl Pts',(46.9380672717436,-13.0991694705089,29.8665989294526));
#21047=CARTESIAN_POINT('Ctrl Pts',(46.923370924553,-13.0707895719798,29.8368060725869));
#21048=CARTESIAN_POINT('Ctrl Pts',(46.9232310976656,-13.0705195543472,29.8365226115073));
#21049=CARTESIAN_POINT('Ctrl Pts',(46.9230909968264,-13.0702494422352,29.8362394045269));
#21050=CARTESIAN_POINT('Ctrl Pts',(46.922950623042,-13.0699792368,29.8359564522459));
#21051=CARTESIAN_POINT('Ctrl Pts',(46.9128450180912,-13.0505269623212,29.8155865236052));
#21052=CARTESIAN_POINT('Ctrl Pts',(46.9013645568325,-13.0305367697038,29.7963754888012));
#21053=CARTESIAN_POINT('Ctrl Pts',(46.8887239261041,-13.0101903794884,29.7783251791885));
#21054=CARTESIAN_POINT('Ctrl Pts',(46.8813478779631,-12.9983178743144,29.7677924806607));
#21055=CARTESIAN_POINT('Ctrl Pts',(46.8735773726895,-12.9863240855329,29.7576540947851));
#21056=CARTESIAN_POINT('Ctrl Pts',(46.8654587684432,-12.9742444051773,29.7479032361322));
#21057=CARTESIAN_POINT('Ctrl Pts',(46.8543462450059,-12.9577100691025,29.7345565275075));
#21058=CARTESIAN_POINT('Ctrl Pts',(46.8425792590554,-12.9410147689399,29.721939386685));
#21059=CARTESIAN_POINT('Ctrl Pts',(46.8302713751129,-12.9242496162066,29.7100434451263));
#21060=CARTESIAN_POINT('Ctrl Pts',(46.8241174331417,-12.9158670398399,29.704095474347));
#21061=CARTESIAN_POINT('Ctrl Pts',(46.8178282665904,-12.9074670004228,29.6983278033295));
#21062=CARTESIAN_POINT('Ctrl Pts',(46.8114180701719,-12.8990608878296,29.6927393855369));
#21063=CARTESIAN_POINT('Ctrl Pts',(46.8050078737534,-12.8906547752363,29.6871509677443));
#21064=CARTESIAN_POINT('Ctrl Pts',(46.7984766474544,-12.8822425894822,29.6817418031665));
#21065=CARTESIAN_POINT('Ctrl Pts',(46.7918385853592,-12.8738357211132,29.6765108449771));
#21066=CARTESIAN_POINT('Ctrl Pts',(46.7709580422564,-12.8473912596395,29.6600564571789));
#21067=CARTESIAN_POINT('Ctrl Pts',(46.7488241283292,-12.8207472740102,29.6452040077705));
#21068=CARTESIAN_POINT('Ctrl Pts',(46.7256543087531,-12.7940681980269,29.6319196349234));
#21069=CARTESIAN_POINT('Ctrl Pts',(46.7193607757097,-12.7868214585468,29.6283112494891));
#21070=CARTESIAN_POINT('Ctrl Pts',(46.7129907957061,-12.779572258173,29.6248188257318));
#21071=CARTESIAN_POINT('Ctrl Pts',(46.7065487443092,-12.7723242153339,29.6214422648954));
#21072=CARTESIAN_POINT('Ctrl Pts',(46.6831396086853,-12.745986266849,29.6091725132756));
#21073=CARTESIAN_POINT('Ctrl Pts',(46.6587794951275,-12.7196622748047,29.5984290980846));
#21074=CARTESIAN_POINT('Ctrl Pts',(46.6336755188529,-12.6935087390576,29.5891798748265));
#21075=CARTESIAN_POINT('Ctrl Pts',(46.6264373389339,-12.6859679417279,29.5865130645443));
#21076=CARTESIAN_POINT('Ctrl Pts',(46.6191373861398,-12.6784415052653,29.583970722176));
#21077=CARTESIAN_POINT('Ctrl Pts',(46.611780876039,-12.6709337131846,29.5815526781396));
#21078=CARTESIAN_POINT('',(40.153012388794,-6.10843371318466,27.4594837601833));
#21079=CARTESIAN_POINT('Origin',(197.498086264171,-177.510315224915,79.5082955755947));
#21080=CARTESIAN_POINT('',(48.4286600918429,-6.1084337131593,4.30318207832973));
#21081=CARTESIAN_POINT('Origin',(0.0835265683620477,-6.10843371318469,0.0824317919394229));
#21082=CARTESIAN_POINT('',(48.3955019191566,-14.6753754514266,30.5110848543371));
#21083=CARTESIAN_POINT('Ctrl Pts',(48.4286600918172,-6.10843371318471,4.30318207891645));
#21084=CARTESIAN_POINT('Ctrl Pts',(48.4268304353416,-6.50994980321315,8.94066112535899));
#21085=CARTESIAN_POINT('Ctrl Pts',(48.4220707934636,-7.55645913600447,13.422965577783));
#21086=CARTESIAN_POINT('Ctrl Pts',(48.4129675603076,-9.80534906153841,19.9830370480983));
#21087=CARTESIAN_POINT('Ctrl Pts',(48.4096078578849,-10.6692546575742,22.1441467079631));
#21088=CARTESIAN_POINT('Ctrl Pts',(48.4026661196857,-12.5596572871779,26.382358737357));
#21089=CARTESIAN_POINT('Ctrl Pts',(48.3990822056017,-13.58630787804,28.4618866519976));
#21090=CARTESIAN_POINT('Ctrl Pts',(48.3955019191565,-14.6753754514262,30.5110848543364));
#21091=CARTESIAN_POINT('',(47.3365522275616,-14.6753754514262,32.1308553965182));
#21092=CARTESIAN_POINT('Origin',(0.0835265683620477,-14.6753754514262,0.0824317919394229));
#21093=CARTESIAN_POINT('Origin',(-1241.46289905476,-1402.95413115888,-321.604288607832));
#21094=CARTESIAN_POINT('Origin',(-4.89277133898972,-11.0169045823054,15.1735300494181));
#21095=CARTESIAN_POINT('',(46.6192727743382,-14.4544045724546,32.1596547801037));
#21096=CARTESIAN_POINT('',(18.8497068160573,-14.4544045823054,23.0026252115117));
#21097=CARTESIAN_POINT('',(-4.89277133898972,-14.4544045823054,15.1735300494181));
#21098=CARTESIAN_POINT('',(18.8497068160573,-11.3294045823054,23.0026252115117));
#21099=CARTESIAN_POINT('',(18.8497068160573,-11.0169045823054,23.0026252115117));
#21100=CARTESIAN_POINT('',(38.3508237177255,-11.3294045823054,29.4331291796839));
#21101=CARTESIAN_POINT('',(-4.89277133898972,-11.3294045823054,15.1735300494181));
#21102=CARTESIAN_POINT('',(38.3508237177255,-12.8919045823054,29.4331291796839));
#21103=CARTESIAN_POINT('',(38.3508237177255,-11.0169045823054,29.4331291796839));
#21104=CARTESIAN_POINT('',(38.9776909489554,-13.5169045823054,29.6398389921663));
#21105=CARTESIAN_POINT('Ctrl Pts',(38.9776909489554,-13.5169045823054,29.6398389921663));
#21106=CARTESIAN_POINT('Ctrl Pts',(38.9423929660079,-13.516904574972,29.6281994629764));
#21107=CARTESIAN_POINT('Ctrl Pts',(38.9071733611761,-13.5137764691096,29.6165857790133));
#21108=CARTESIAN_POINT('Ctrl Pts',(38.8724709034065,-13.5077394335846,29.6051426245749));
#21109=CARTESIAN_POINT('Ctrl Pts',(38.8352487396173,-13.5012640557713,29.5928685956978));
#21110=CARTESIAN_POINT('Ctrl Pts',(38.7986204242306,-13.4914421682004,29.5807903886535));
#21111=CARTESIAN_POINT('Ctrl Pts',(38.7631069894986,-13.4784883891908,29.5690798141137));
#21112=CARTESIAN_POINT('Ctrl Pts',(38.7270416010364,-13.4653332811151,29.5571872325292));
#21113=CARTESIAN_POINT('Ctrl Pts',(38.6921244765178,-13.4489478321352,29.5456732916074));
#21114=CARTESIAN_POINT('Ctrl Pts',(38.6589020389608,-13.42950318155,29.5347181746438));
#21115=CARTESIAN_POINT('Ctrl Pts',(38.6267589654953,-13.4106902684037,29.52411897858));
#21116=CARTESIAN_POINT('Ctrl Pts',(38.5962009713873,-13.3890130655275,29.5140424633077));
#21117=CARTESIAN_POINT('Ctrl Pts',(38.5677442515497,-13.3645846069919,29.5046588443803));
#21118=CARTESIAN_POINT('Ctrl Pts',(38.558505004034,-13.3566532439914,29.5016121974597));
#21119=CARTESIAN_POINT('Ctrl Pts',(38.5494875136696,-13.3484315569659,29.4986386750814));
#21120=CARTESIAN_POINT('Ctrl Pts',(38.5407102902568,-13.3399225829036,29.4957443808616));
#21121=CARTESIAN_POINT('Ctrl Pts',(38.5406156491554,-13.339830834222,29.4957131729067));
#21122=CARTESIAN_POINT('Ctrl Pts',(38.5405210362793,-13.3397390509053,29.4956819742591));
#21123=CARTESIAN_POINT('Ctrl Pts',(38.5404264516427,-13.3396472329756,29.4956507849234));
#21124=CARTESIAN_POINT('Ctrl Pts',(38.5055810206749,-13.305821070019,29.4841604850084));
#21125=CARTESIAN_POINT('Ctrl Pts',(38.4747122807658,-13.2674403224072,29.4739815011308));
#21126=CARTESIAN_POINT('Ctrl Pts',(38.4485152007503,-13.2257618865581,29.4653429996623));
#21127=CARTESIAN_POINT('Ctrl Pts',(38.4347246221117,-13.2038216647177,29.4607955488109));
#21128=CARTESIAN_POINT('Ctrl Pts',(38.4222290644973,-13.1809667715254,29.4566751318507));
#21129=CARTESIAN_POINT('Ctrl Pts',(38.4111336890027,-13.1573764603983,29.4530164257106));
#21130=CARTESIAN_POINT('Ctrl Pts',(38.3932412272899,-13.1193345988278,29.4471163766711));
#21131=CARTESIAN_POINT('Ctrl Pts',(38.3789843342392,-13.079375361177,29.4424151583871));
#21132=CARTESIAN_POINT('Ctrl Pts',(38.3688260877462,-13.0382175960838,29.4390654710481));
#21133=CARTESIAN_POINT('Ctrl Pts',(38.3588686319705,-12.9978733667896,29.4357819945579));
#21134=CARTESIAN_POINT('Ctrl Pts',(38.3528498623,-12.9563778845286,29.433797301966));
#21135=CARTESIAN_POINT('Ctrl Pts',(38.3512529278809,-12.9144212114187,29.4332707119675));
#21136=CARTESIAN_POINT('Ctrl Pts',(38.3509677633351,-12.9069290091781,29.4331766788025));
#21137=CARTESIAN_POINT('Ctrl Pts',(38.3508237212182,-12.899422137453,29.4331291808356));
#21138=CARTESIAN_POINT('Ctrl Pts',(38.3508237177256,-12.8919045823054,29.4331291796839));
#21139=CARTESIAN_POINT('',(45.6922912884794,-13.5169045823054,31.8539821279529));
#21140=CARTESIAN_POINT('',(-4.89277133898972,-13.5169045823054,15.1735300494181));
#21141=CARTESIAN_POINT('Origin',(-1220.21421106998,-1402.3016656762,-385.579379660149));
#21142=CARTESIAN_POINT('Origin',(-6.76693169846985,-11.0169045823054,20.8571001776055));
#21143=CARTESIAN_POINT('',(33.7901189707501,-12.8919045823054,34.2308098261781));
#21144=CARTESIAN_POINT('',(33.7901189707501,-11.3294045823054,34.2308098261781));
#21145=CARTESIAN_POINT('',(33.7901189707501,-11.0169045823054,34.2308098261781));
#21146=CARTESIAN_POINT('',(-6.76693169846985,-11.3294045823054,20.8571001776055));
#21147=CARTESIAN_POINT('',(-6.76693169846985,-11.3294045823054,20.8571001776055));
#21148=CARTESIAN_POINT('',(-6.76693169846985,-14.4544045823054,20.8571001776055));
#21149=CARTESIAN_POINT('',(-6.76693169846985,-11.0169045823054,20.8571001776055));
#21150=CARTESIAN_POINT('',(42.5114259882145,-14.4544045474401,37.1066655869754));
#21151=CARTESIAN_POINT('',(43.4136327877683,-14.4544045823054,37.4041687727522));
#21152=CARTESIAN_POINT('',(41.5416017773197,-13.5169045823054,36.7868655227931));
#21153=CARTESIAN_POINT('Origin',(-529.90702904109,-669.972712130993,-151.648633150656));
#21154=CARTESIAN_POINT('',(34.4578582575083,-13.5169045823054,34.4509972213337));
#21155=CARTESIAN_POINT('',(34.2758494659228,-13.5169045823054,34.390979722724));
#21156=CARTESIAN_POINT('Ctrl Pts',(33.7901189707501,-12.8919045823054,34.2308098261781));
#21157=CARTESIAN_POINT('Ctrl Pts',(33.7901189707501,-12.9240089539701,34.2308098261781));
#21158=CARTESIAN_POINT('Ctrl Pts',(33.7927314458503,-12.955801183802,34.2316712912717));
#21159=CARTESIAN_POINT('Ctrl Pts',(33.7978675102913,-12.9870390822583,34.2333649113313));
#21160=CARTESIAN_POINT('Ctrl Pts',(33.8031273642748,-13.0190298772567,34.2350993510602));
#21161=CARTESIAN_POINT('Ctrl Pts',(33.8110337447306,-13.0504387215006,34.2377064843414));
#21162=CARTESIAN_POINT('Ctrl Pts',(33.8214395081087,-13.0810143824798,34.2411377905089));
#21163=CARTESIAN_POINT('Ctrl Pts',(33.8287255515569,-13.102423248534,34.2435403673225));
#21164=CARTESIAN_POINT('Ctrl Pts',(33.8372358660587,-13.1234238076975,34.2463466481858));
#21165=CARTESIAN_POINT('Ctrl Pts',(33.8469063040395,-13.1439346499851,34.2495354804013));
#21166=CARTESIAN_POINT('Ctrl Pts',(33.8469498796939,-13.1440270732421,34.2495498494972));
#21167=CARTESIAN_POINT('Ctrl Pts',(33.8469934759197,-13.1441194808469,34.2495642253765));
#21168=CARTESIAN_POINT('Ctrl Pts',(33.8470370927095,-13.144211872797,34.2495786080368));
#21169=CARTESIAN_POINT('Ctrl Pts',(33.8816554487368,-13.2175427491137,34.2609940298788));
#21170=CARTESIAN_POINT('Ctrl Pts',(33.9294439233777,-13.2814833076921,34.276752305537));
#21171=CARTESIAN_POINT('Ctrl Pts',(33.9877805172936,-13.3355724235757,34.2959888293));
#21172=CARTESIAN_POINT('Ctrl Pts',(33.9918226137392,-13.3393202156285,34.2973217128146));
#21173=CARTESIAN_POINT('Ctrl Pts',(33.995915366069,-13.3430206975362,34.2986713001347));
#21174=CARTESIAN_POINT('Ctrl Pts',(34.0000579079991,-13.3466737099127,34.3000373056028));
#21175=CARTESIAN_POINT('Ctrl Pts',(34.0001081300639,-13.346717997171,34.3000538663561));
#21176=CARTESIAN_POINT('Ctrl Pts',(34.0001583569437,-13.3467622754631,34.3000704286972));
#21177=CARTESIAN_POINT('Ctrl Pts',(34.0002085886379,-13.3468065447898,34.3000869926259));
#21178=CARTESIAN_POINT('Ctrl Pts',(34.0641821309938,-13.4031865990189,34.3211823032219));
#21179=CARTESIAN_POINT('Ctrl Pts',(34.1359363403631,-13.44500831055,34.3448432930207));
#21180=CARTESIAN_POINT('Ctrl Pts',(34.2146228130674,-13.4738659092282,34.3707902004465));
#21181=CARTESIAN_POINT('Ctrl Pts',(34.2933529212196,-13.5027395108379,34.3967514966851));
#21182=CARTESIAN_POINT('Ctrl Pts',(34.3745006619984,-13.5169045582356,34.423510008606));
#21183=CARTESIAN_POINT('Ctrl Pts',(34.4578582575083,-13.5169045823054,34.4509972213337));
#21184=CARTESIAN_POINT('Origin',(0.0835265683620477,-6.01690458230549,0.0824317919394229));
#21185=CARTESIAN_POINT('',(4.30427670995454,-6.10843422628143,48.4275654856862));
#21186=CARTESIAN_POINT('',(32.2061415767159,-6.10843371299758,36.4583066734133));
#21187=CARTESIAN_POINT('Origin',(0.0835265683620477,-6.10843371318469,0.0824317919394229));
#21188=CARTESIAN_POINT('',(39.2939826516718,-12.6709337131846,38.7814849549994));
#21189=CARTESIAN_POINT('Ctrl Pts',(32.2061415763564,-6.10843371318765,36.4583066739843));
#21190=CARTESIAN_POINT('Ctrl Pts',(32.6895829804899,-6.54712953976792,36.6166555923948));
#21191=CARTESIAN_POINT('Ctrl Pts',(33.1721101495054,-6.98698298247605,36.7746225070907));
#21192=CARTESIAN_POINT('Ctrl Pts',(33.6537398736913,-7.42790908709483,36.9323189016539));
#21193=CARTESIAN_POINT('Ctrl Pts',(34.1334866890221,-7.86711141175329,37.0893987895464));
#21194=CARTESIAN_POINT('Ctrl Pts',(34.6123431500573,-8.30737802767375,37.2462103272133));
#21195=CARTESIAN_POINT('Ctrl Pts',(35.0903517895406,-8.74862497312237,37.402819026504));
#21196=CARTESIAN_POINT('Ctrl Pts',(35.5674289513232,-9.18901207701961,37.559122548233));
#21197=CARTESIAN_POINT('Ctrl Pts',(36.0436616592707,-9.63037569350405,37.7152240805629));
#21198=CARTESIAN_POINT('Ctrl Pts',(36.5191169505044,-10.0726323507254,37.8711432684101));
#21199=CARTESIAN_POINT('Ctrl Pts',(36.993227181731,-10.5136378666649,38.0266213618626));
#21200=CARTESIAN_POINT('Ctrl Pts',(37.4665644488621,-10.9555313776754,38.1819181817231));
#21201=CARTESIAN_POINT('Ctrl Pts',(37.939218906132,-11.3982301183281,38.3370072007052));
#21202=CARTESIAN_POINT('Ctrl Pts',(38.3913986968972,-11.8217518281976,38.4853780011381));
#21203=CARTESIAN_POINT('Ctrl Pts',(38.8429537376373,-12.246010516087,38.6335583573869));
#21204=CARTESIAN_POINT('Ctrl Pts',(39.2939826516718,-12.6709337131846,38.7814849549994));
#21205=CARTESIAN_POINT('',(40.4397116715677,-13.2959337131846,38.4974020809805));
#21206=CARTESIAN_POINT('Ctrl Pts',(40.4397116715676,-13.2959337131846,38.4974020809807));
#21207=CARTESIAN_POINT('Ctrl Pts',(40.4066868182815,-13.2959336603245,38.5320956948767));
#21208=CARTESIAN_POINT('Ctrl Pts',(40.3709843137298,-13.2916605128677,38.5633120948844));
#21209=CARTESIAN_POINT('Ctrl Pts',(40.3335867953624,-13.2840750781525,38.5914271479214));
#21210=CARTESIAN_POINT('Ctrl Pts',(40.2903824802747,-13.2753118359423,38.6239076884263));
#21211=CARTESIAN_POINT('Ctrl Pts',(40.2449149265883,-13.2621273075678,38.6522492669877));
#21212=CARTESIAN_POINT('Ctrl Pts',(40.1986646417893,-13.2459526169444,38.6769937284272));
#21213=CARTESIAN_POINT('Ctrl Pts',(40.1851376876442,-13.2412219585426,38.6842308124082));
#21214=CARTESIAN_POINT('Ctrl Pts',(40.1715436445126,-13.2362352705239,38.6911599698083));
#21215=CARTESIAN_POINT('Ctrl Pts',(40.1579193431335,-13.2310278528738,38.6977942320586));
#21216=CARTESIAN_POINT('Ctrl Pts',(40.1578742334737,-13.2310106112676,38.6978161979052));
#21217=CARTESIAN_POINT('Ctrl Pts',(40.1578291234839,-13.230993367242,38.6978381605175));
#21218=CARTESIAN_POINT('Ctrl Pts',(40.1577840131655,-13.2309761207982,38.6978601198961));
#21219=CARTESIAN_POINT('Ctrl Pts',(40.0679185768218,-13.1966190323189,38.7416059680517));
#21220=CARTESIAN_POINT('Ctrl Pts',(39.9767121201785,-13.152555648727,38.7724161582456));
#21221=CARTESIAN_POINT('Ctrl Pts',(39.8871981003423,-13.1028429786438,38.7931532120191));
#21222=CARTESIAN_POINT('Ctrl Pts',(39.8766190756684,-13.0969677921157,38.7956039767589));
#21223=CARTESIAN_POINT('Ctrl Pts',(39.8660637060712,-13.091013740083,38.7979140888403));
#21224=CARTESIAN_POINT('Ctrl Pts',(39.855537010514,-13.0849875486837,38.8000883045475));
#21225=CARTESIAN_POINT('Ctrl Pts',(39.8554152338134,-13.0849178354767,38.8001134566775));
#21226=CARTESIAN_POINT('Ctrl Pts',(39.8552934598642,-13.0848481114876,38.8001385901193));
#21227=CARTESIAN_POINT('Ctrl Pts',(39.8551716886783,-13.0847783767298,38.8001637048806));
#21228=CARTESIAN_POINT('Ctrl Pts',(39.8303839263928,-13.0705831581647,38.8052760697483));
#21229=CARTESIAN_POINT('Ctrl Pts',(39.8055929272658,-13.0558793142743,38.8096455507573));
#21230=CARTESIAN_POINT('Ctrl Pts',(39.780884675532,-13.0407301262923,38.8132772606744));
#21231=CARTESIAN_POINT('Ctrl Pts',(39.7436402270521,-13.0178947125452,38.8187515869991));
#21232=CARTESIAN_POINT('Ctrl Pts',(39.7065811166617,-12.9940463246918,38.8225507431792));
#21233=CARTESIAN_POINT('Ctrl Pts',(39.6699900069733,-12.9693962501975,38.8246970808061));
#21234=CARTESIAN_POINT('Ctrl Pts',(39.633398897285,-12.9447461757032,38.8268434184329));
#21235=CARTESIAN_POINT('Ctrl Pts',(39.5972757976144,-12.9192944015675,38.8273369465679));
#21236=CARTESIAN_POINT('Ctrl Pts',(39.5619034483267,-12.8932521061511,38.8262000930124));
#21237=CARTESIAN_POINT('Ctrl Pts',(39.5318432459393,-12.8711207892717,38.8252339697932));
#21238=CARTESIAN_POINT('Ctrl Pts',(39.5022622280843,-12.8485482515855,38.8231336850165));
#21239=CARTESIAN_POINT('Ctrl Pts',(39.4731842379688,-12.8255048445977,38.8198375199283));
#21240=CARTESIAN_POINT('Ctrl Pts',(39.4566401434559,-12.8123941618582,38.8179621473));
#21241=CARTESIAN_POINT('Ctrl Pts',(39.4402593911746,-12.7991308725963,38.8156988765352));
#21242=CARTESIAN_POINT('Ctrl Pts',(39.4240511389472,-12.7857088195892,38.8130305325372));
#21243=CARTESIAN_POINT('Ctrl Pts',(39.3951315085124,-12.7617604748081,38.8082695304741));
#21244=CARTESIAN_POINT('Ctrl Pts',(39.3667585577106,-12.7373067239787,38.802221542794));
#21245=CARTESIAN_POINT('Ctrl Pts',(39.3389584490096,-12.7123167139678,38.7948212644581));
#21246=CARTESIAN_POINT('Ctrl Pts',(39.3237928405683,-12.6986840799789,38.790784239826));
#21247=CARTESIAN_POINT('Ctrl Pts',(39.3087981609348,-12.6848916911023,38.7863440783211));
#21248=CARTESIAN_POINT('Ctrl Pts',(39.2939826516718,-12.6709337131846,38.7814849549994));
#21249=CARTESIAN_POINT('',(41.6084251757828,-13.2959337131846,37.2309770398429));
#21250=CARTESIAN_POINT('Origin',(0.0835265683620477,-13.2959337131846,0.0824317919394229));
#21251=CARTESIAN_POINT('',(43.0359437581361,-14.6753754514262,37.6994458553003));
#21252=CARTESIAN_POINT('Origin',(-537.184566063455,-671.736419692119,-133.458018919704));
#21253=CARTESIAN_POINT('',(30.51217970824,-14.675375306047,48.3944072657487));
#21254=CARTESIAN_POINT('Origin',(0.0835265683620477,-14.6753754514262,0.0824317919394229));
#21255=CARTESIAN_POINT('Ctrl Pts',(30.5121799406814,-14.6753748699083,48.3944076347922));
#21256=CARTESIAN_POINT('Ctrl Pts',(29.6488324750175,-14.2165313293604,48.3959217299873));
#21257=CARTESIAN_POINT('Ctrl Pts',(28.7803560530607,-13.7688961397319,48.3974310167534));
#21258=CARTESIAN_POINT('Ctrl Pts',(27.9060899457771,-13.3339028956054,48.3989301271172));
#21259=CARTESIAN_POINT('Ctrl Pts',(27.056709414216,-12.9112915306634,48.4003865660059));
#21260=CARTESIAN_POINT('Ctrl Pts',(26.2018640443159,-12.5006127566903,48.4018333971136));
#21261=CARTESIAN_POINT('Ctrl Pts',(25.3409737846802,-12.1031392031217,48.4032655009723));
#21262=CARTESIAN_POINT('Ctrl Pts',(25.0217106273087,-11.9557352102624,48.4037966000229));
#21263=CARTESIAN_POINT('Ctrl Pts',(24.7016163733872,-11.8101469191841,48.4043256718175));
#21264=CARTESIAN_POINT('Ctrl Pts',(24.3806624063341,-11.6664376689275,48.4048524492713));
#21265=CARTESIAN_POINT('Ctrl Pts',(24.3484751771087,-11.6520256252868,48.4049052777401));
#21266=CARTESIAN_POINT('Ctrl Pts',(24.3162792494227,-11.6376325718389,48.4049580822714));
#21267=CARTESIAN_POINT('Ctrl Pts',(24.2840745830158,-11.6232585917439,48.4050108624134));
#21268=CARTESIAN_POINT('Ctrl Pts',(23.5112493892555,-11.2783218111032,48.4062774435657));
#21269=CARTESIAN_POINT('Ctrl Pts',(22.7333797368795,-10.9443666917881,48.4075285034311));
#21270=CARTESIAN_POINT('Ctrl Pts',(21.9499770951734,-10.622542813258,48.4087548715985));
#21271=CARTESIAN_POINT('Ctrl Pts',(21.679859986483,-10.5115779901286,48.4091777231513));
#21272=CARTESIAN_POINT('Ctrl Pts',(21.4090853092871,-10.4020550292294,48.409597642173));
#21273=CARTESIAN_POINT('Ctrl Pts',(21.137633790018,-10.2940198074425,48.4100142623316));
#21274=CARTESIAN_POINT('Ctrl Pts',(21.1213606839124,-10.2875432600575,48.410039238077));
#21275=CARTESIAN_POINT('Ctrl Pts',(21.1050848873588,-10.2810720136182,48.4100642022031));
#21276=CARTESIAN_POINT('Ctrl Pts',(21.0888064415878,-10.2746060938733,48.4100891545555));
#21277=CARTESIAN_POINT('Ctrl Pts',(20.6329211858941,-10.0935250792803,48.4107879564984));
#21278=CARTESIAN_POINT('Ctrl Pts',(20.1749952047483,-9.9166326383212,48.4114781297796));
#21279=CARTESIAN_POINT('Ctrl Pts',(19.7152601034564,-9.74425107298764,48.4121573955266));
#21280=CARTESIAN_POINT('Ctrl Pts',(19.2749122844202,-9.57913893314155,48.4128080162631));
#21281=CARTESIAN_POINT('Ctrl Pts',(18.8329032539855,-9.41816464509348,48.4134486342682));
#21282=CARTESIAN_POINT('Ctrl Pts',(18.3894211536449,-9.26165511776138,48.4140771416491));
#21283=CARTESIAN_POINT('Ctrl Pts',(18.2037607417664,-9.19613359325097,48.414340261489));
#21284=CARTESIAN_POINT('Ctrl Pts',(18.0178420881853,-9.13139516038838,48.414601257143));
#21285=CARTESIAN_POINT('Ctrl Pts',(17.8316790387899,-9.06746659619147,48.414859965488));
#21286=CARTESIAN_POINT('Ctrl Pts',(17.8280779083912,-9.06622996466542,48.4148649699316));
#21287=CARTESIAN_POINT('Ctrl Pts',(17.8244767169066,-9.06499364665141,48.4148699734635));
#21288=CARTESIAN_POINT('Ctrl Pts',(17.8208754647278,-9.06375764243283,48.4148749760823));
#21289=CARTESIAN_POINT('Ctrl Pts',(16.9526599969218,-8.76577296167702,48.4160810429658));
#21290=CARTESIAN_POINT('Ctrl Pts',(16.0792020931599,-8.48534970221955,48.4172359828182));
#21291=CARTESIAN_POINT('Ctrl Pts',(15.2000695648677,-8.22405492504872,48.4183278724742));
#21292=CARTESIAN_POINT('Ctrl Pts',(14.9739344468961,-8.15684330068117,48.4186087341057));
#21293=CARTESIAN_POINT('Ctrl Pts',(14.7474238161432,-8.09089757132381,48.4188854218506));
#21294=CARTESIAN_POINT('Ctrl Pts',(14.5205302069433,-8.02624496071279,48.4191577282275));
#21295=CARTESIAN_POINT('Ctrl Pts',(14.0020828443853,-7.87851503754759,48.4197799428567));
#21296=CARTESIAN_POINT('Ctrl Pts',(13.4813283109344,-7.73745329658892,48.4203795067404));
#21297=CARTESIAN_POINT('Ctrl Pts',(12.958692622873,-7.60353311380589,48.4209531569399));
#21298=CARTESIAN_POINT('Ctrl Pts',(12.4566635157299,-7.47489316187225,48.4215041891486));
#21299=CARTESIAN_POINT('Ctrl Pts',(11.9528986695681,-7.35284273129184,48.4220313090909));
#21300=CARTESIAN_POINT('Ctrl Pts',(11.4477849931265,-7.23775611982421,48.4225317776524));
#21301=CARTESIAN_POINT('Ctrl Pts',(11.2675563144811,-7.1966922783921,48.4227103489162));
#21302=CARTESIAN_POINT('Ctrl Pts',(11.0871541074089,-7.15651419440583,48.4228855304241));
#21303=CARTESIAN_POINT('Ctrl Pts',(10.9066091662104,-7.11724012295064,48.423057191374));
#21304=CARTESIAN_POINT('Ctrl Pts',(9.81752556341492,-6.88033098025773,48.4240926849439));
#21305=CARTESIAN_POINT('Ctrl Pts',(8.72304426013872,-6.67627260244091,48.4250002518316));
#21306=CARTESIAN_POINT('Ctrl Pts',(7.62278160794834,-6.50737682456698,48.4257586248259));
#21307=CARTESIAN_POINT('Ctrl Pts',(6.52251895575796,-6.33848104669305,48.4265169978202));
#21308=CARTESIAN_POINT('Ctrl Pts',(5.41647491773991,-6.20474805616561,48.4271261752529));
#21309=CARTESIAN_POINT('Ctrl Pts',(4.30427673497461,-6.10843510301176,48.4275652912163));
#21310=CARTESIAN_POINT('Origin',(0.0835265683620477,11.4830954176946,0.0824317919394229));
#21311=CARTESIAN_POINT('',(34.3285543476724,11.4830954176946,36.0841779807601));
#21312=CARTESIAN_POINT('',(-34.1615012109487,11.4830954176946,36.0841779807597));
#21313=CARTESIAN_POINT('Origin',(0.0835265683620477,12.0636401876617,0.0824317919394229));
#21314=CARTESIAN_POINT('',(-34.8465649140277,13.0346110567823,36.7726127649112));
#21315=CARTESIAN_POINT('',(-34.8465649140274,13.0346110567825,36.7726127649118));
#21316=CARTESIAN_POINT('',(35.0136180507511,13.0346110567825,36.7726127649121));
#21317=CARTESIAN_POINT('',(34.3916369666324,12.1551693185409,36.1504966431761));
#21318=CARTESIAN_POINT('',(8.7871565714169,13.0346110567825,49.98761684888));
#21319=CARTESIAN_POINT('Origin',(0.0835265683620477,13.0346110567825,0.0824317919394229));
#21320=CARTESIAN_POINT('',(-8.62010343469277,13.0346110567825,49.98761684888));
#21321=CARTESIAN_POINT('Ctrl Pts',(8.7871565714169,13.0346110567825,49.98761684888));
#21322=CARTESIAN_POINT('Ctrl Pts',(7.92550064906484,12.8871967548028,49.9882530796749));
#21323=CARTESIAN_POINT('Ctrl Pts',(7.06161609265391,12.7606786217037,49.9888052593523));
#21324=CARTESIAN_POINT('Ctrl Pts',(6.19543459293618,12.6558408129365,49.98926502916));
#21325=CARTESIAN_POINT('Ctrl Pts',(5.61894217814055,12.5860653656916,49.9895710317781));
#21326=CARTESIAN_POINT('Ctrl Pts',(5.04143250829548,12.5258925149755,49.9898361091157));
#21327=CARTESIAN_POINT('Ctrl Pts',(4.46288801112708,12.4755408811181,49.9900578945362));
#21328=CARTESIAN_POINT('Ctrl Pts',(4.45970749302406,12.4752640756455,49.9900591137899));
#21329=CARTESIAN_POINT('Ctrl Pts',(4.45652691494998,12.4749875690291,49.9900603317248));
#21330=CARTESIAN_POINT('Ctrl Pts',(4.45334627723674,12.4747113612835,49.9900615483407));
#21331=CARTESIAN_POINT('Ctrl Pts',(4.030833582814,12.4380202039354,49.9902231623675));
#21332=CARTESIAN_POINT('Ctrl Pts',(3.60755981318608,12.4066244502022,49.9903617724682));
#21333=CARTESIAN_POINT('Ctrl Pts',(3.18378964752083,12.3805167222776,49.9904772560375));
#21334=CARTESIAN_POINT('Ctrl Pts',(2.75593208301871,12.3541571769636,49.9905938534827));
#21335=CARTESIAN_POINT('Ctrl Pts',(2.32756730732015,12.3331879704976,49.9906868771953));
#21336=CARTESIAN_POINT('Ctrl Pts',(1.89895102917436,12.3176520559944,49.9907559814859));
#21337=CARTESIAN_POINT('Ctrl Pts',(1.47793210215791,12.3023915202009,49.9908238608825));
#21338=CARTESIAN_POINT('Ctrl Pts',(1.05666935743236,12.2923733967889,49.9908686614172));
#21339=CARTESIAN_POINT('Ctrl Pts',(0.635406610984126,12.2876877721288,49.9908898373879));
#21340=CARTESIAN_POINT('Ctrl Pts',(0.451513336654972,12.28564236254,49.9908990813066));
#21341=CARTESIAN_POINT('Ctrl Pts',(0.267620182626321,12.2846137392999,49.9909038205458));
#21342=CARTESIAN_POINT('Ctrl Pts',(0.0837483634682333,12.2846124143579,
49.9909039962098));
#21343=CARTESIAN_POINT('Ctrl Pts',(0.0798267472639425,12.2846123860996,
49.9909039999564));
#21344=CARTESIAN_POINT('Ctrl Pts',(0.0759051865461643,12.2846128251744,
49.9909040015881));
#21345=CARTESIAN_POINT('Ctrl Pts',(0.0719836819143394,12.2846137316609,
49.9909040011047));
#21346=CARTESIAN_POINT('Ctrl Pts',(-1.08470971159645,12.2848811103974,49.990903858513));
#21347=CARTESIAN_POINT('Ctrl Pts',(-2.23919271888792,12.3254286614639,49.9907197297609));
#21348=CARTESIAN_POINT('Ctrl Pts',(-3.39148882634123,12.4051717612022,49.990365638491));
#21349=CARTESIAN_POINT('Ctrl Pts',(-3.68831749711159,12.4257133894741,49.9902744254423));
#21350=CARTESIAN_POINT('Ctrl Pts',(-3.98500107435261,12.4488556287919,49.9901719363719));
#21351=CARTESIAN_POINT('Ctrl Pts',(-4.28154000423778,12.4745793828298,49.9900584161199));
#21352=CARTESIAN_POINT('Ctrl Pts',(-4.82827914657013,12.5220071631409,49.9898491148816));
#21353=CARTESIAN_POINT('Ctrl Pts',(-5.37459250935462,12.578220119787,49.9896018888339));
#21354=CARTESIAN_POINT('Ctrl Pts',(-5.92009010621466,12.643043269177,49.9893181539585));
#21355=CARTESIAN_POINT('Ctrl Pts',(-6.47328863096735,12.7087815434037,49.9890304135258));
#21356=CARTESIAN_POINT('Ctrl Pts',(-7.02564819591232,12.7833747882158,49.9887051270459));
#21357=CARTESIAN_POINT('Ctrl Pts',(-7.5767680370208,12.8665869343008,49.9883440006327));
#21358=CARTESIAN_POINT('Ctrl Pts',(-7.92507488019195,12.9191768752799,49.9881157693269));
#21359=CARTESIAN_POINT('Ctrl Pts',(-8.27288667005804,12.9752083234333,49.9878732273165));
#21360=CARTESIAN_POINT('Ctrl Pts',(-8.62010343469276,13.0346110567825,49.98761684888));
#21361=CARTESIAN_POINT('Origin',(0.0835265683620477,13.0346110567825,0.0824317919394229));
#21362=CARTESIAN_POINT('Origin',(0.0835265683620477,16.4830954176946,50.0824317919394));
#21363=CARTESIAN_POINT('',(-22.6217205869088,-8.87385981233827,50.0824317919394));
#21364=CARTESIAN_POINT('',(-21.5367763897373,-8.69080155057986,50.0824317919394));
#21365=CARTESIAN_POINT('Ctrl Pts',(-22.6217205869088,-8.87385981233827,
50.0824317919394));
#21366=CARTESIAN_POINT('Ctrl Pts',(-22.5517841558568,-8.87385981188611,
50.0824317919394));
#21367=CARTESIAN_POINT('Ctrl Pts',(-22.4818161430779,-8.87185808464267,
50.0824317919395));
#21368=CARTESIAN_POINT('Ctrl Pts',(-22.4120212868203,-8.86782837150089,
50.0824317919394));
#21369=CARTESIAN_POINT('Ctrl Pts',(-22.3411456944659,-8.86373626040192,
50.0824317919393));
#21370=CARTESIAN_POINT('Ctrl Pts',(-22.2704470198759,-8.85755327620029,
50.0824317919393));
#21371=CARTESIAN_POINT('Ctrl Pts',(-22.2001193077708,-8.84920383564279,
50.0824317919363));
#21372=CARTESIAN_POINT('Ctrl Pts',(-22.1568417202882,-8.84406583764253,
50.0824317919344));
#21373=CARTESIAN_POINT('Ctrl Pts',(-22.1137043120179,-8.83810648050711,
50.0824317919313));
#21374=CARTESIAN_POINT('Ctrl Pts',(-22.0707526912653,-8.83129827231295,
50.082431791925));
#21375=CARTESIAN_POINT('Ctrl Pts',(-22.0704240016376,-8.83124617212726,
50.082431791925));
#21376=CARTESIAN_POINT('Ctrl Pts',(-22.070095320049,-8.83119402657727,50.0824317919249));
#21377=CARTESIAN_POINT('Ctrl Pts',(-22.0697666464964,-8.83114183558492,
50.0824317919249));
#21378=CARTESIAN_POINT('Ctrl Pts',(-21.9572130892569,-8.81326914154647,
50.0824317919083));
#21379=CARTESIAN_POINT('Ctrl Pts',(-21.8458794227438,-8.79011900697435,
50.0824317919293));
#21380=CARTESIAN_POINT('Ctrl Pts',(-21.7364461053673,-8.75874571241513,
50.0824317919358));
#21381=CARTESIAN_POINT('Ctrl Pts',(-21.6691162959035,-8.73944301744465,
50.0824317919398));
#21382=CARTESIAN_POINT('Ctrl Pts',(-21.6025059895988,-8.71702701269503,
50.0824317919394));
#21383=CARTESIAN_POINT('Ctrl Pts',(-21.5367763897394,-8.69080155058071,
50.0824317919394));
#21384=CARTESIAN_POINT('',(-44.2914734316384,-8.87385981233827,50.082431791939));
#21385=CARTESIAN_POINT('',(0.0835265683620477,-8.87385981233827,50.0824317919394));
#21386=CARTESIAN_POINT('',(-44.2914734316384,-14.4544045823054,50.082431791939));
#21387=CARTESIAN_POINT('',(-44.2914734316384,16.4830954176946,50.082431791939));
#21388=CARTESIAN_POINT('',(44.458526568362,-14.4544045823054,50.0824317919394));
#21389=CARTESIAN_POINT('',(0.0835265683620477,-14.4544045823054,50.0824317919394));
#21390=CARTESIAN_POINT('',(44.458526568362,-8.87385981233827,50.0824317919394));
#21391=CARTESIAN_POINT('',(44.458526568362,16.4830954176946,50.0824317919394));
#21392=CARTESIAN_POINT('',(22.7887737236329,-8.87385981233827,50.0824317919394));
#21393=CARTESIAN_POINT('',(0.0835265683620477,-8.87385981233827,50.0824317919394));
#21394=CARTESIAN_POINT('',(21.7038295264614,-8.69080155057986,50.0824317919394));
#21395=CARTESIAN_POINT('Ctrl Pts',(21.7038295264614,-8.69080155057986,50.0824317919394));
#21396=CARTESIAN_POINT('Ctrl Pts',(21.8139951203631,-8.7347565461317,50.0824317919394));
#21397=CARTESIAN_POINT('Ctrl Pts',(21.9275645136047,-8.76821292000628,50.0824317919394));
#21398=CARTESIAN_POINT('Ctrl Pts',(22.0424292060519,-8.79411643469838,50.0824317919394));
#21399=CARTESIAN_POINT('Ctrl Pts',(22.1075139143365,-8.80879390138867,50.0824317919394));
#21400=CARTESIAN_POINT('Ctrl Pts',(22.1730141788683,-8.82104760689908,50.0824317919394));
#21401=CARTESIAN_POINT('Ctrl Pts',(22.2385467888997,-8.83141832822413,50.0824317919393));
#21402=CARTESIAN_POINT('Ctrl Pts',(22.2386507853477,-8.83143478595685,50.0824317919393));
#21403=CARTESIAN_POINT('Ctrl Pts',(22.2387547823744,-8.83145123875071,50.0824317919393));
#21404=CARTESIAN_POINT('Ctrl Pts',(22.2388587799798,-8.83146768660594,50.0824317919393));
#21405=CARTESIAN_POINT('Ctrl Pts',(22.4201525755661,-8.86014040550798,50.0824317919389));
#21406=CARTESIAN_POINT('Ctrl Pts',(22.6035144602885,-8.87385980853305,50.0824317919394));
#21407=CARTESIAN_POINT('Ctrl Pts',(22.7887737236329,-8.87385981233827,50.0824317919394));
#21408=CARTESIAN_POINT('Ctrl Pts',(21.7038295264614,-8.69080155057986,50.0824317919394));
#21409=CARTESIAN_POINT('Ctrl Pts',(20.8438722721191,-8.34768669240134,50.0824317919394));
#21410=CARTESIAN_POINT('Ctrl Pts',(19.9790807826263,-8.0198017877672,50.0824317919394));
#21411=CARTESIAN_POINT('Ctrl Pts',(19.1089707832958,-7.70866381791472,50.0824317919393));
#21412=CARTESIAN_POINT('Ctrl Pts',(18.2388607839653,-7.39752584806224,50.0824317919392));
#21413=CARTESIAN_POINT('Ctrl Pts',(17.3634321497246,-7.10313511035514,50.0824317919392));
#21414=CARTESIAN_POINT('Ctrl Pts',(16.4822225240427,-6.82695644195446,50.0824317919394));
#21415=CARTESIAN_POINT('Ctrl Pts',(16.4713288078639,-6.82354225770076,50.0824317919394));
#21416=CARTESIAN_POINT('Ctrl Pts',(16.4604342061586,-6.8201308617252,50.0824317919394));
#21417=CARTESIAN_POINT('Ctrl Pts',(16.4495387178998,-6.81672225716408,50.0824317919394));
#21418=CARTESIAN_POINT('Ctrl Pts',(15.7049370028632,-6.58377695523626,50.0824317919395));
#21419=CARTESIAN_POINT('Ctrl Pts',(14.9561560013555,-6.36386066915742,50.0824317919409));
#21420=CARTESIAN_POINT('Ctrl Pts',(14.2029817792061,-6.15798672786968,50.0824317919379));
#21421=CARTESIAN_POINT('Ctrl Pts',(14.0708035005379,-6.12185688913941,50.0824317919374));
#21422=CARTESIAN_POINT('Ctrl Pts',(13.9384899672118,-6.08615941362245,50.0824317919367));
#21423=CARTESIAN_POINT('Ctrl Pts',(13.8060400877123,-6.05089962282538,50.0824317919355));
#21424=CARTESIAN_POINT('Ctrl Pts',(13.7943582912455,-6.04778978458991,50.0824317919354));
#21425=CARTESIAN_POINT('Ctrl Pts',(13.7826750481892,-6.04468327282916,50.0824317919353));
#21426=CARTESIAN_POINT('Ctrl Pts',(13.7709903766333,-6.04158009539295,50.0824317919352));
#21427=CARTESIAN_POINT('Ctrl Pts',(13.2422785619911,-5.90116651460846,50.0824317919303));
#21428=CARTESIAN_POINT('Ctrl Pts',(12.7107942008915,-5.76761845987533,50.082431791934));
#21429=CARTESIAN_POINT('Ctrl Pts',(12.1776858808268,-5.64153128315994,50.0824317919343));
#21430=CARTESIAN_POINT('Ctrl Pts',(11.8131021981237,-5.5553024146573,50.0824317919345));
#21431=CARTESIAN_POINT('Ctrl Pts',(11.4477578757322,-5.47256360697682,50.0824317919357));
#21432=CARTESIAN_POINT('Ctrl Pts',(11.0820121822203,-5.39351662111253,50.0824317919211));
#21433=CARTESIAN_POINT('Ctrl Pts',(11.073124940469,-5.3915958611814,50.0824317919208));
#21434=CARTESIAN_POINT('Ctrl Pts',(11.0642375260462,-5.38967730441635,50.0824317919204));
#21435=CARTESIAN_POINT('Ctrl Pts',(11.055349936817,-5.38776095106557,50.0824317919201));
#21436=CARTESIAN_POINT('Ctrl Pts',(7.4174461363494,-4.60335148320463,50.0824317917656));
#21437=CARTESIAN_POINT('Ctrl Pts',(3.74693618253599,-4.18752460344888,50.0824317918031));
#21438=CARTESIAN_POINT('Ctrl Pts',(0.0393470995888544,-4.1908181579504,
50.0824317919243));
#21439=CARTESIAN_POINT('Ctrl Pts',(0.0324484243578657,-4.19082428623548,
50.0824317919245));
#21440=CARTESIAN_POINT('Ctrl Pts',(0.0255496208096622,-4.19083186535561,
50.0824317919247));
#21441=CARTESIAN_POINT('Ctrl Pts',(0.0186506889146812,-4.19084089563808,
50.082431791925));
#21442=CARTESIAN_POINT('Ctrl Pts',(-0.901382134976211,-4.19204516267696,
50.0824317919539));
#21443=CARTESIAN_POINT('Ctrl Pts',(-1.82367679464876,-4.21882226363321,
50.0824317919392));
#21444=CARTESIAN_POINT('Ctrl Pts',(-2.7482570531487,-4.27143022964227,50.0824317919393));
#21445=CARTESIAN_POINT('Ctrl Pts',(-2.75919896624817,-4.27205281679695,
50.0824317919393));
#21446=CARTESIAN_POINT('Ctrl Pts',(-2.7701413179277,-4.27267902824778,50.0824317919394));
#21447=CARTESIAN_POINT('Ctrl Pts',(-2.78108410830146,-4.27330886465574,
50.0824317919394));
#21448=CARTESIAN_POINT('Ctrl Pts',(-3.70172929220981,-4.32629862648306,
50.0824317919395));
#21449=CARTESIAN_POINT('Ctrl Pts',(-4.616569426888,-4.40442769523306,50.0824317919392));
#21450=CARTESIAN_POINT('Ctrl Pts',(-5.52572806394492,-4.50641515619345,
50.0824317919393));
#21451=CARTESIAN_POINT('Ctrl Pts',(-5.53960751684282,-4.50797212337484,
50.0824317919393));
#21452=CARTESIAN_POINT('Ctrl Pts',(-5.55348564086543,-4.50953465011809,
50.0824317919393));
#21453=CARTESIAN_POINT('Ctrl Pts',(-5.56736243615774,-4.51110273180162,
50.0824317919393));
#21454=CARTESIAN_POINT('Ctrl Pts',(-6.6470334253265,-4.63310585043909,50.0824317919394));
#21455=CARTESIAN_POINT('Ctrl Pts',(-7.71878011925584,-4.78875206539942,
50.0824317919394));
#21456=CARTESIAN_POINT('Ctrl Pts',(-8.78314336260521,-4.9757301443796,50.0824317919394));
#21457=CARTESIAN_POINT('Ctrl Pts',(-9.5185957422456,-5.10492802300404,50.0824317919393));
#21458=CARTESIAN_POINT('Ctrl Pts',(-10.2505231824639,-5.24908423888419,
50.0824317919393));
#21459=CARTESIAN_POINT('Ctrl Pts',(-10.979107895046,-5.40742232363259,50.0824317919393));
#21460=CARTESIAN_POINT('Ctrl Pts',(-10.9937292654063,-5.41059988107961,
50.0824317919393));
#21461=CARTESIAN_POINT('Ctrl Pts',(-11.0083492885202,-5.41378314936643,
50.0824317919393));
#21462=CARTESIAN_POINT('Ctrl Pts',(-11.0229679658942,-5.41697212217387,
50.0824317919393));
#21463=CARTESIAN_POINT('Ctrl Pts',(-12.1324973546702,-5.65900900138861,
50.0824317919394));
#21464=CARTESIAN_POINT('Ctrl Pts',(-13.2343102827012,-5.93379674455981,
50.0824317919394));
#21465=CARTESIAN_POINT('Ctrl Pts',(-14.3290278568824,-6.23869144822421,
50.0824317919394));
#21466=CARTESIAN_POINT('Ctrl Pts',(-15.4414775636244,-6.5485248076935,50.0824317919394));
#21467=CARTESIAN_POINT('Ctrl Pts',(-16.5466002367016,-6.88944821125723,
50.0824317919394));
#21468=CARTESIAN_POINT('Ctrl Pts',(-17.6450618211739,-7.25863482930252,
50.0824317919394));
#21469=CARTESIAN_POINT('Ctrl Pts',(-18.7713890095441,-7.63718691648054,
50.0824317919394));
#21470=CARTESIAN_POINT('Ctrl Pts',(-19.8907128989818,-8.04545424379275,
50.0824317919394));
#21471=CARTESIAN_POINT('Ctrl Pts',(-21.0037656572773,-8.4803367087874,50.0824317919394));
#21472=CARTESIAN_POINT('Ctrl Pts',(-21.1815949414308,-8.54981664750956,
50.0824317919394));
#21473=CARTESIAN_POINT('Ctrl Pts',(-21.3592641797394,-8.61997584796747,
50.0824317919394));
#21474=CARTESIAN_POINT('Ctrl Pts',(-21.5367763897373,-8.69080155057986,
50.0824317919394));
#21475=CARTESIAN_POINT('Origin',(44.4585265683621,16.4830954176946,44.4574317919394));
#21476=CARTESIAN_POINT('Origin',(44.4585265683621,-8.87385981233827,44.4574317919394));
#21477=CARTESIAN_POINT('Origin',(44.4585265683621,-14.4544045823054,44.4574317919394));
#21478=CARTESIAN_POINT('Origin',(0.0835265683620477,16.4830954176946,50.0824317919394));
#21479=CARTESIAN_POINT('',(-44.2914734316384,16.1705954176946,50.082431791939));
#21480=CARTESIAN_POINT('',(-44.2914734316384,13.4386401876617,50.082431791939));
#21481=CARTESIAN_POINT('',(-44.2914734316384,16.4830954176946,50.082431791939));
#21482=CARTESIAN_POINT('',(-10.8649863601191,13.4386401876617,50.0824317919394));
#21483=CARTESIAN_POINT('',(0.0835265683620477,13.4386401876617,50.0824317919394));
#21484=CARTESIAN_POINT('',(-8.58213843785641,13.2555819259033,50.0824317919394));
#21485=CARTESIAN_POINT('Ctrl Pts',(-8.5821384378566,13.2555819259034,50.0824317919394));
#21486=CARTESIAN_POINT('Ctrl Pts',(-8.82298135330014,13.2969611280073,50.0824317919394));
#21487=CARTESIAN_POINT('Ctrl Pts',(-9.06501105460157,13.3294628821421,50.0824317919394));
#21488=CARTESIAN_POINT('Ctrl Pts',(-9.3077915193297,13.3553162053718,50.0824317919394));
#21489=CARTESIAN_POINT('Ctrl Pts',(-9.44488714767125,13.3699153107688,50.0824317919394));
#21490=CARTESIAN_POINT('Ctrl Pts',(-9.58222240123873,13.3823932020222,50.0824317919394));
#21491=CARTESIAN_POINT('Ctrl Pts',(-9.71971984082492,13.3931443825079,50.0824317919394));
#21492=CARTESIAN_POINT('Ctrl Pts',(-9.71978638257171,13.3931495855308,50.0824317919394));
#21493=CARTESIAN_POINT('Ctrl Pts',(-9.71985292434008,13.3931547881239,50.0824317919394));
#21494=CARTESIAN_POINT('Ctrl Pts',(-9.71991946613004,13.3931599902873,50.0824317919394));
#21495=CARTESIAN_POINT('Ctrl Pts',(-10.1009757205579,13.4229505456848,50.0824317919394));
#21496=CARTESIAN_POINT('Ctrl Pts',(-10.4826417866386,13.4386401851025,50.0824317919394));
#21497=CARTESIAN_POINT('Ctrl Pts',(-10.8649863601191,13.4386401876617,50.0824317919394));
#21498=CARTESIAN_POINT('',(8.74919157458055,13.2555819259033,50.0824317919394));
#21499=CARTESIAN_POINT('Ctrl Pts',(-8.58213843785641,13.2555819259033,50.0824317919394));
#21500=CARTESIAN_POINT('Ctrl Pts',(-7.37516628549685,13.0482120850067,50.0824317919394));
#21501=CARTESIAN_POINT('Ctrl Pts',(-6.16542111429013,12.8826695784009,50.0824317919394));
#21502=CARTESIAN_POINT('Ctrl Pts',(-4.95280295520423,12.7604365635511,50.0824317919394));
#21503=CARTESIAN_POINT('Ctrl Pts',(-3.75084982134647,12.6392785929576,50.0824317919394));
#21504=CARTESIAN_POINT('Ctrl Pts',(-2.54607400932527,12.5606716819902,50.0824317919394));
#21505=CARTESIAN_POINT('Ctrl Pts',(-1.3383838944826,12.5260083291904,50.0824317919394));
#21506=CARTESIAN_POINT('Ctrl Pts',(-0.868840927440839,12.5125314170909,
50.0824317919394));
#21507=CARTESIAN_POINT('Ctrl Pts',(-0.398857493567957,12.5056965050877,
50.0824317919394));
#21508=CARTESIAN_POINT('Ctrl Pts',(0.0715715529620946,12.5055833090051,
50.0824317919394));
#21509=CARTESIAN_POINT('Ctrl Pts',(0.071725964608064,12.5055832718501,50.0824317919394));
#21510=CARTESIAN_POINT('Ctrl Pts',(0.0718803762799654,12.5055832354192,
50.0824317919394));
#21511=CARTESIAN_POINT('Ctrl Pts',(0.0720347879778126,12.5055831997124,
50.0824317919394));
#21512=CARTESIAN_POINT('Ctrl Pts',(0.535468761960413,12.5054760332808,50.0824317919394));
#21513=CARTESIAN_POINT('Ctrl Pts',(0.99956602790721,12.5119501585725,50.0824317919398));
#21514=CARTESIAN_POINT('Ctrl Pts',(1.4637993848865,12.5248910213249,50.0824317919345));
#21515=CARTESIAN_POINT('Ctrl Pts',(1.9305422533797,12.5379018386455,50.0824317919291));
#21516=CARTESIAN_POINT('Ctrl Pts',(2.39742400942509,12.5574495854694,50.0824317919166));
#21517=CARTESIAN_POINT('Ctrl Pts',(2.86391070485841,12.5834701483563,50.0824317919075));
#21518=CARTESIAN_POINT('Ctrl Pts',(3.31881454076369,12.6088446209523,50.0824317918986));
#21519=CARTESIAN_POINT('Ctrl Pts',(3.77334384985895,12.6403747667456,50.0824317918966));
#21520=CARTESIAN_POINT('Ctrl Pts',(4.22698698482929,12.6780474220166,50.082431791909));
#21521=CARTESIAN_POINT('Ctrl Pts',(4.29353516680801,12.6835738954168,50.0824317919108));
#21522=CARTESIAN_POINT('Ctrl Pts',(4.36006423101712,12.6892326346471,50.0824317919129));
#21523=CARTESIAN_POINT('Ctrl Pts',(4.42657250848413,12.6950236788102,50.0824317919151));
#21524=CARTESIAN_POINT('Ctrl Pts',(4.43223940031558,12.6955171094344,50.0824317919153));
#21525=CARTESIAN_POINT('Ctrl Pts',(4.43790610260004,12.6960114970058,50.0824317919155));
#21526=CARTESIAN_POINT('Ctrl Pts',(4.44357261344172,12.6965068414395,50.0824317919157));
#21527=CARTESIAN_POINT('Ctrl Pts',(5.29122519267014,12.7706053473037,50.0824317919435));
#21528=CARTESIAN_POINT('Ctrl Pts',(6.13664037252339,12.865971941344,50.082431791939));
#21529=CARTESIAN_POINT('Ctrl Pts',(6.97986484277041,12.9818931833795,50.0824317919393));
#21530=CARTESIAN_POINT('Ctrl Pts',(7.57070936299085,13.0631188036627,50.0824317919395));
#21531=CARTESIAN_POINT('Ctrl Pts',(8.16047853122286,13.1544351596487,50.0824317919394));
#21532=CARTESIAN_POINT('Ctrl Pts',(8.74919157458055,13.2555819259033,50.0824317919394));
#21533=CARTESIAN_POINT('',(11.0320394968433,13.4386401876617,50.0824317919394));
#21534=CARTESIAN_POINT('Ctrl Pts',(11.0320394968433,13.4386401876617,50.0824317919394));
#21535=CARTESIAN_POINT('Ctrl Pts',(10.7909520272503,13.4386401861139,50.0824317919394));
#21536=CARTESIAN_POINT('Ctrl Pts',(10.5500159553784,13.4323889945159,50.0824317919395));
#21537=CARTESIAN_POINT('Ctrl Pts',(10.3093654004934,13.4203066131624,50.0824317919393));
#21538=CARTESIAN_POINT('Ctrl Pts',(10.1686166605505,13.4132400183987,50.0824317919392));
#21539=CARTESIAN_POINT('Ctrl Pts',(10.0279654246317,13.4041776979188,50.082431791939));
#21540=CARTESIAN_POINT('Ctrl Pts',(9.88743785753373,13.3931955538157,50.0824317919381));
#21541=CARTESIAN_POINT('Ctrl Pts',(9.88718986684206,13.3931761734936,50.0824317919381));
#21542=CARTESIAN_POINT('Ctrl Pts',(9.88694187686581,13.3931567875853,50.0824317919381));
#21543=CARTESIAN_POINT('Ctrl Pts',(9.88669388760501,13.3931373960886,50.0824317919381));
#21544=CARTESIAN_POINT('Ctrl Pts',(9.50564813228723,13.363341559395,50.0824317919358));
#21545=CARTESIAN_POINT('Ctrl Pts',(9.12614644683353,13.3203465159016,50.0824317919394));
#21546=CARTESIAN_POINT('Ctrl Pts',(8.74919157458055,13.2555819259033,50.0824317919394));
#21547=CARTESIAN_POINT('',(44.458526568362,13.4386401876617,50.0824317919394));
#21548=CARTESIAN_POINT('',(0.0835265683620477,13.4386401876617,50.0824317919394));
#21549=CARTESIAN_POINT('',(44.458526568362,16.1705954176946,50.0824317919394));
#21550=CARTESIAN_POINT('',(44.458526568362,16.4830954176946,50.0824317919394));
#21551=CARTESIAN_POINT('',(-44.2914734316384,16.1705954176946,50.0824317919394));
#21552=CARTESIAN_POINT('Origin',(44.4585265683621,16.4830954176946,44.4574317919394));
#21553=CARTESIAN_POINT('Origin',(44.4585265683621,13.4386401876617,44.4574317919394));
#21554=CARTESIAN_POINT('Origin',(44.4585265683621,16.1705954176946,44.4574317919394));
#21555=CARTESIAN_POINT('Origin',(0.0835265683620477,16.4830954176946,0.0824317919394229));
#21556=CARTESIAN_POINT('',(48.4087001792127,16.3915662868156,22.6760194541559));
#21557=CARTESIAN_POINT('',(48.428660091855,11.5746245485365,4.30318207805399));
#21558=CARTESIAN_POINT('Ctrl Pts',(48.4087001792126,16.3915662868154,22.6760194541555));
#21559=CARTESIAN_POINT('Ctrl Pts',(48.4133626632511,15.1541680928392,19.7444122941847));
#21560=CARTESIAN_POINT('Ctrl Pts',(48.41771013248,14.0894359483376,16.7558018285945));
#21561=CARTESIAN_POINT('Ctrl Pts',(48.4229917226254,12.8480220597894,12.1554610849062));
#21562=CARTESIAN_POINT('Ctrl Pts',(48.4245437904912,12.4934998941785,10.599655099974));
#21563=CARTESIAN_POINT('Ctrl Pts',(48.4270638166904,11.9258476364963,7.46837373314965));
#21564=CARTESIAN_POINT('Ctrl Pts',(48.4280340859824,11.7120008366799,5.88986732862775));
#21565=CARTESIAN_POINT('Ctrl Pts',(48.4286600918172,11.5746245485738,4.30318207891633));
#21566=CARTESIAN_POINT('',(4.30427685494149,11.5746245485738,48.4275653154293));
#21567=CARTESIAN_POINT('Origin',(0.0835265683620477,11.5746245485738,0.0824317919394229));
#21568=CARTESIAN_POINT('',(22.6771142305786,16.3915662868157,48.4076054027901));
#21569=CARTESIAN_POINT('Ctrl Pts',(4.30427685533877,11.5746245485738,48.4275653153946));
#21570=CARTESIAN_POINT('Ctrl Pts',(5.88955930980395,11.7118793817134,48.4269398630142));
#21571=CARTESIAN_POINT('Ctrl Pts',(7.46274649560755,11.9249456441311,48.4259731407403));
#21572=CARTESIAN_POINT('Ctrl Pts',(10.5868505406711,12.4906656417943,48.4234615008534));
#21573=CARTESIAN_POINT('Ctrl Pts',(12.140036765244,12.843980457976,48.4219144210431));
#21574=CARTESIAN_POINT('Ctrl Pts',(16.7459605252979,14.0856585112706,48.4166308714132));
#21575=CARTESIAN_POINT('Ctrl Pts',(19.7463324981469,15.1545164964592,48.4122665740529));
#21576=CARTESIAN_POINT('Ctrl Pts',(22.677114230578,16.3915662868154,48.40760540279));
#21577=CARTESIAN_POINT('Origin',(0.0835265683620477,16.3915662868154,0.0824317919394229));
#21578=CARTESIAN_POINT('Origin',(0.0835265683620484,-85.4775827009602,48.5199317919394));
#21579=CARTESIAN_POINT('',(-4.11800505968102,11.7955954176946,48.5199317919394));
#21580=CARTESIAN_POINT('',(0.0835265683619702,11.6131136241746,48.5199317919394));
#21581=CARTESIAN_POINT('Origin',(0.0850736516346928,84.3502669679634,48.5199317979947));
#21582=CARTESIAN_POINT('',(-21.3522104186698,16.1706033824526,48.5199317918264));
#21583=CARTESIAN_POINT('Ctrl Pts',(-4.11800505968102,11.7955954176946,48.5199317919393));
#21584=CARTESIAN_POINT('Ctrl Pts',(-5.3330850955866,11.9012754509056,48.5199317919355));
#21585=CARTESIAN_POINT('Ctrl Pts',(-6.54284928166413,12.052058373043,48.5199317917982));
#21586=CARTESIAN_POINT('Ctrl Pts',(-7.74758204934735,12.2455340355694,48.5199317918421));
#21587=CARTESIAN_POINT('Ctrl Pts',(-8.00842309407842,12.2874241503709,48.5199317918516));
#21588=CARTESIAN_POINT('Ctrl Pts',(-8.26902825280743,12.3313158148411,48.5199317918681));
#21589=CARTESIAN_POINT('Ctrl Pts',(-8.52940037578031,12.3771848834521,48.5199317918868));
#21590=CARTESIAN_POINT('Ctrl Pts',(-8.60796598979772,12.3910255799855,48.5199317918924));
#21591=CARTESIAN_POINT('Ctrl Pts',(-8.68650600951455,12.4050450140606,48.5199317918896));
#21592=CARTESIAN_POINT('Ctrl Pts',(-8.76502160741265,12.4192427232393,48.5199317918772));
#21593=CARTESIAN_POINT('Ctrl Pts',(-9.31742370497652,12.5191317203411,48.5199317917904));
#21594=CARTESIAN_POINT('Ctrl Pts',(-9.86933137746676,12.628070795559,48.5199317909336));
#21595=CARTESIAN_POINT('Ctrl Pts',(-10.4199054294347,12.7454889373136,48.5199317856301));
#21596=CARTESIAN_POINT('Ctrl Pts',(-10.9847756532994,12.8659559512995,48.5199317801888));
#21597=CARTESIAN_POINT('Ctrl Pts',(-11.5482433946011,12.9953485172464,48.5199317698611));
#21598=CARTESIAN_POINT('Ctrl Pts',(-12.1093930468112,13.1331031830766,48.5199317678938));
#21599=CARTESIAN_POINT('Ctrl Pts',(-12.3711272379419,13.1973553943959,48.5199317669762));
#21600=CARTESIAN_POINT('Ctrl Pts',(-12.6323568698691,13.2634275009716,48.5199317681592));
#21601=CARTESIAN_POINT('Ctrl Pts',(-12.8929871215291,13.3312657045529,48.5199317717506));
#21602=CARTESIAN_POINT('Ctrl Pts',(-13.0886265997407,13.3821877700727,48.5199317744464));
#21603=CARTESIAN_POINT('Ctrl Pts',(-13.2839532567454,13.4341067575178,48.5199317766964));
#21604=CARTESIAN_POINT('Ctrl Pts',(-13.4789066329929,13.4869947668886,48.5199317786076));
#21605=CARTESIAN_POINT('Ctrl Pts',(-14.2827231347708,13.7050584675371,48.5199317864876));
#21606=CARTESIAN_POINT('Ctrl Pts',(-15.0813881500244,13.9395350034094,48.5199317889602));
#21607=CARTESIAN_POINT('Ctrl Pts',(-15.8751970172333,14.1892982824324,48.5199317903271));
#21608=CARTESIAN_POINT('Ctrl Pts',(-16.6833025247604,14.4435598429844,48.5199317917186));
#21609=CARTESIAN_POINT('Ctrl Pts',(-17.4863754330999,14.7136635664768,48.5199317918044));
#21610=CARTESIAN_POINT('Ctrl Pts',(-18.2847477442816,14.9983707526771,48.5199317918862));
#21611=CARTESIAN_POINT('Ctrl Pts',(-19.1070061411662,15.2915959450188,48.5199317919706));
#21612=CARTESIAN_POINT('Ctrl Pts',(-19.9242785136404,15.6003113768466,48.5199317919394));
#21613=CARTESIAN_POINT('Ctrl Pts',(-20.7369483477271,15.9231126709707,48.5199317919394));
#21614=CARTESIAN_POINT('Ctrl Pts',(-20.9423235837733,16.0046899477393,48.5199317919394));
#21615=CARTESIAN_POINT('Ctrl Pts',(-21.1474049737681,16.0871665859416,48.5199317919394));
#21616=CARTESIAN_POINT('Ctrl Pts',(-21.3521989016608,16.170519439565,48.5199317919394));
#21617=CARTESIAN_POINT('',(21.5192634427593,16.17060336129,48.5199317918263));
#21618=CARTESIAN_POINT('',(0.0835265683620484,16.1705954176946,48.5199317919394));
#21619=CARTESIAN_POINT('',(4.28505819640496,11.7955954176946,48.5199317919394));
#21620=CARTESIAN_POINT('Ctrl Pts',(21.5192519564043,16.1705196413466,48.5199317919394));
#21621=CARTESIAN_POINT('Ctrl Pts',(20.7158295319576,15.8435202227492,48.5199317919394));
#21622=CARTESIAN_POINT('Ctrl Pts',(19.9079782705932,15.5300086685378,48.5199317919526));
#21623=CARTESIAN_POINT('Ctrl Pts',(19.0953265097735,15.2313679634678,48.5199317919262));
#21624=CARTESIAN_POINT('Ctrl Pts',(18.299910033755,14.9390610385645,48.5199317919003));
#21625=CARTESIAN_POINT('Ctrl Pts',(17.4998944429049,14.6610010604542,48.5199317919232));
#21626=CARTESIAN_POINT('Ctrl Pts',(16.6949498262278,14.3984390229379,48.5199317911674));
#21627=CARTESIAN_POINT('Ctrl Pts',(15.9108077115892,14.1426624799854,48.5199317904312));
#21628=CARTESIAN_POINT('Ctrl Pts',(15.1219880157985,13.90159329815,48.519931789089));
#21629=CARTESIAN_POINT('Ctrl Pts',(14.3282043783767,13.6763418781801,48.5199317840016));
#21630=CARTESIAN_POINT('Ctrl Pts',(14.1012822681381,13.6119483518537,48.5199317825472));
#21631=CARTESIAN_POINT('Ctrl Pts',(13.8739546053117,13.5488472152168,48.5199317807643));
#21632=CARTESIAN_POINT('Ctrl Pts',(13.6462149928204,13.4870636734954,48.5199317785163));
#21633=CARTESIAN_POINT('Ctrl Pts',(13.4512631341532,13.4341751304708,48.5199317765919));
#21634=CARTESIAN_POINT('Ctrl Pts',(13.255935603651,13.3822549873816,48.5199317743262));
#21635=CARTESIAN_POINT('Ctrl Pts',(13.0602932043519,13.3313312754882,48.5199317716117));
#21636=CARTESIAN_POINT('Ctrl Pts',(12.500626902414,13.1856558716985,48.5199317638463));
#21637=CARTESIAN_POINT('Ctrl Pts',(11.9381747386843,13.0481153498591,48.5199317690783));
#21638=CARTESIAN_POINT('Ctrl Pts',(11.3738769394113,12.9192577967887,48.5199317762763));
#21639=CARTESIAN_POINT('Ctrl Pts',(10.8211684440881,12.7930466643683,48.5199317833265));
#21640=CARTESIAN_POINT('Ctrl Pts',(10.2666880661914,12.6751650328318,48.5199317893989));
#21641=CARTESIAN_POINT('Ctrl Pts',(9.71130192517919,12.5661734820257,48.5199317909776));
#21642=CARTESIAN_POINT('Ctrl Pts',(9.45179182555766,12.5152460171163,48.5199317917152));
#21643=CARTESIAN_POINT('Ctrl Pts',(9.19208383600685,12.4662602455223,48.5199317918358));
#21644=CARTESIAN_POINT('Ctrl Pts',(8.93226615131867,12.4192773203273,48.5199317918769));
#21645=CARTESIAN_POINT('Ctrl Pts',(8.85373981326765,12.4050773744271,48.5199317918893));
#21646=CARTESIAN_POINT('Ctrl Pts',(8.77518928258344,12.3910557938706,48.5199317918922));
#21647=CARTESIAN_POINT('Ctrl Pts',(8.69661339645869,12.377213039333,48.5199317918865));
#21648=CARTESIAN_POINT('Ctrl Pts',(7.49688801165072,12.1658567971894,48.5199317918003));
#21649=CARTESIAN_POINT('Ctrl Pts',(6.29223043630813,11.9964818494364,48.5199317918738));
#21650=CARTESIAN_POINT('Ctrl Pts',(5.08236080976824,11.871466704724,48.5199317919214));
#21651=CARTESIAN_POINT('Ctrl Pts',(4.81684531529824,11.8440311387453,48.5199317919318));
#21652=CARTESIAN_POINT('Ctrl Pts',(4.55107877638799,11.8187322176555,48.5199317919385));
#21653=CARTESIAN_POINT('Ctrl Pts',(4.28505819640497,11.7955954176945,48.5199317919394));
#21654=CARTESIAN_POINT('Origin',(0.0819794773143091,84.3502670306517,48.5199317979381));
#21655=CARTESIAN_POINT('Origin',(39.8582830101054,16.4855954176946,41.1830134484075));
#21656=CARTESIAN_POINT('',(34.7649027499964,-3.61941807409669,36.0896331882986));
#21657=CARTESIAN_POINT('',(38.0393490816114,-8.24885981233827,39.3640795199135));
#21658=CARTESIAN_POINT('Ctrl Pts',(34.7649027499964,-3.61941807409669,36.0896331882986));
#21659=CARTESIAN_POINT('Ctrl Pts',(35.3114139634271,-4.3920600802535,36.6361444017293));
#21660=CARTESIAN_POINT('Ctrl Pts',(35.8579212247445,-5.16470767732065,37.1826516630466));
#21661=CARTESIAN_POINT('Ctrl Pts',(36.9494030102706,-6.70785538323105,38.2741334485728));
#21662=CARTESIAN_POINT('Ctrl Pts',(37.4943775524999,-7.4783554666459,38.819107990802));
#21663=CARTESIAN_POINT('Ctrl Pts',(38.0393490816114,-8.24885981233827,39.3640795199135));
#21664=CARTESIAN_POINT('',(39.195370402743,-8.24885981233827,40.5201008410451));
#21665=CARTESIAN_POINT('',(35.3869530268201,12.8136401876617,36.7116834651222));
#21666=CARTESIAN_POINT('',(35.3001596224904,12.8136401876617,36.6248900607926));
#21667=CARTESIAN_POINT('',(34.7649027499964,11.9341984494202,36.0896331882986));
#21668=CARTESIAN_POINT('',(35.3869530268201,12.8136401876617,36.7116834651222));
#21669=CARTESIAN_POINT('',(34.7649027499964,-3.74885981233827,36.0896331882986));
#21670=CARTESIAN_POINT('Origin',(41.1841082248301,16.4855954176946,39.8571882336827));
#21671=CARTESIAN_POINT('',(39.3651742963361,-8.24885981233827,38.0382543051887));
#21672=CARTESIAN_POINT('',(39.2780566719443,-8.24885981233827,37.9511366807969));
#21673=CARTESIAN_POINT('',(36.0907279647212,-3.61941807409669,34.7638079735738));
#21674=CARTESIAN_POINT('Ctrl Pts',(39.3651742963361,-8.24885981233827,38.0382543051887));
#21675=CARTESIAN_POINT('Ctrl Pts',(38.8202027672246,-7.4783554666459,37.4932827760772));
#21676=CARTESIAN_POINT('Ctrl Pts',(38.2752282249954,-6.70785538323104,36.948308233848));
#21677=CARTESIAN_POINT('Ctrl Pts',(37.1837464394692,-5.16470767732064,35.8568264483218));
#21678=CARTESIAN_POINT('Ctrl Pts',(36.6372391781519,-4.3920600802535,35.3103191870045));
#21679=CARTESIAN_POINT('Ctrl Pts',(36.0907279647212,-3.61941807409669,34.7638079735738));
#21680=CARTESIAN_POINT('',(36.0907279647215,11.9341984494207,34.7638079735741));
#21681=CARTESIAN_POINT('',(36.0907279647212,12.0636401876617,34.7638079735738));
#21682=CARTESIAN_POINT('',(36.7127782415448,12.8136401876617,35.3858582503974));
#21683=CARTESIAN_POINT('',(36.0907279647212,11.9341984494202,34.7638079735738));
#21684=CARTESIAN_POINT('',(40.5211956174677,12.8136401876617,39.1942756263203));
#21685=CARTESIAN_POINT('Origin',(0.0835265683620477,-11.0169045823054,0.0824317919394229));
#21686=CARTESIAN_POINT('',(10.0669432604883,-11.3294045823054,19.5464246030606));
#21687=CARTESIAN_POINT('',(10.0669432604883,-14.4544045823054,19.5464246030606));
#21688=CARTESIAN_POINT('',(10.0669432604883,-11.0169045823054,19.5464246030606));
#21689=CARTESIAN_POINT('Origin',(0.0835265683620477,-14.4544045823054,0.0824317919394229));
#21690=CARTESIAN_POINT('Origin',(0.0835265683620477,-11.3294045823054,0.0824317919394229));
#21691=CARTESIAN_POINT('Origin',(0.0835265683620477,-13.2044045823054,0.0824317919394229));
#21692=CARTESIAN_POINT('',(34.3599945679822,-13.2044045823054,34.7477781982718));
#21693=CARTESIAN_POINT('',(41.4437380877936,-13.2044045823054,37.0836464997312));
#21694=CARTESIAN_POINT('',(41.7058392642912,-13.2044045823054,37.1700745060874));
#21695=CARTESIAN_POINT('',(40.2796596827637,-13.2044045823054,38.3450489192809));
#21696=CARTESIAN_POINT('Origin',(0.0835265683620477,-13.2044045823054,0.0824317919394229));
#21697=CARTESIAN_POINT('',(33.0778695430594,-13.2044045823054,35.9702546803237));
#21698=CARTESIAN_POINT('',(-7.35411383562686,-13.2044045823054,22.6377860392341));
#21699=CARTESIAN_POINT('Origin',(0.0835265683620477,-13.2044045823054,0.0824317919394229));
#21700=CARTESIAN_POINT('Origin',(-7.45197752515304,16.4855954176946,22.9345670161721));
#21701=CARTESIAN_POINT('',(32.9800058535332,-12.8919045823054,36.2670356572618));
#21702=CARTESIAN_POINT('',(39.2345740945198,-12.8919045823054,38.3294829568536));
#21703=CARTESIAN_POINT('',(-7.45197752515304,-12.8919045823054,22.9345670161721));
#21704=CARTESIAN_POINT('',(32.9800027480559,-7.07886051013688,36.2670346332676));
#21705=CARTESIAN_POINT('Ctrl Pts',(39.2345740945198,-12.8919045823054,38.3294829568536));
#21706=CARTESIAN_POINT('Ctrl Pts',(37.5830392601106,-11.3339023349487,37.7848884415858));
#21707=CARTESIAN_POINT('Ctrl Pts',(35.9239895753391,-9.78474033199855,37.2378159002995));
#21708=CARTESIAN_POINT('Ctrl Pts',(34.2546478225026,-8.24794399593134,36.6873495439375));
#21709=CARTESIAN_POINT('Ctrl Pts',(33.8304517690206,-7.85742902818579,36.5474706632071));
#21710=CARTESIAN_POINT('Ctrl Pts',(33.4055909787826,-7.46771271821857,36.4073725851676));
#21711=CARTESIAN_POINT('Ctrl Pts',(32.9800195165679,-7.07885337126715,36.267040162655));
#21712=CARTESIAN_POINT('',(32.9800058535332,16.4855954176946,36.2670356572618));
#21713=CARTESIAN_POINT('Origin',(0.0835265683620477,-13.2044045823054,0.0824317919394229));
#21714=CARTESIAN_POINT('',(40.0376426042469,-13.2044045823054,28.0150491378139));
#21715=CARTESIAN_POINT('',(46.6900312637982,-13.2044045823054,30.2086779380909));
#21716=CARTESIAN_POINT('',(46.8934224522321,-13.2044045823054,30.2757462937605));
#21717=CARTESIAN_POINT('',(45.7901549780056,-13.2044045823054,31.5572011510148));
#21718=CARTESIAN_POINT('Origin',(0.0835265683620477,-13.2044045823054,0.0824317919394229));
#21719=CARTESIAN_POINT('',(39.0755546384815,-13.2044045823054,29.3430580152282));
#21720=CARTESIAN_POINT('',(-4.79490764946354,-13.2044045823054,14.87674907248));
#21721=CARTESIAN_POINT('Origin',(0.0835265683620477,-13.2044045823054,0.0824317919394229));
#21722=CARTESIAN_POINT('Origin',(-4.20772551230653,16.4855954176946,13.0960632108515));
#21723=CARTESIAN_POINT('',(46.3272934177549,-12.8919045823054,29.7600133527852));
#21724=CARTESIAN_POINT('Ctrl Pts',(40.1355068578762,-6.59534981976388,27.7182683468891));
#21725=CARTESIAN_POINT('Ctrl Pts',(42.2041064756925,-8.68909917313972,28.4003902026783));
#21726=CARTESIAN_POINT('Ctrl Pts',(44.2674821932045,-10.7885698299899,29.0807894744839));
#21727=CARTESIAN_POINT('Ctrl Pts',(46.327293417755,-12.8919045823054,29.7600133527852));
#21728=CARTESIAN_POINT('',(39.9141752801041,-12.8919045823054,27.6452841380193));
#21729=CARTESIAN_POINT('Origin',(0.0835265683620477,15.5455954176946,0.0824317919394229));
#21730=CARTESIAN_POINT('',(29.1308110078832,16.1705954176946,46.7863424064645));
#21731=CARTESIAN_POINT('Origin',(0.0835265683620477,16.1705954176946,0.0824317919394229));
#21732=CARTESIAN_POINT('',(29.1308110078832,15.8580954176946,46.7863424064645));
#21733=CARTESIAN_POINT('',(29.1308110078832,15.5455954176946,46.7863424064645));
#21734=CARTESIAN_POINT('Origin',(0.0835265683620477,15.8580954176946,0.0824317919394229));
#21735=CARTESIAN_POINT('Origin',(48.5210265683621,15.5455954176946,42.8336341598436));
#21736=CARTESIAN_POINT('',(48.5210265683621,15.8580954176946,35.8884670232579));
#21737=CARTESIAN_POINT('',(48.5210265683621,15.8580954176946,42.8336341598436));
#21738=CARTESIAN_POINT('',(48.5210265683621,16.1705954176946,35.8884670232579));
#21739=CARTESIAN_POINT('',(48.5210265683621,15.5455954176946,35.8884670232579));
#21740=CARTESIAN_POINT('',(48.5210265683621,16.1705954176946,29.6248403980433));
#21741=CARTESIAN_POINT('Origin',(26.1374820022305,15.5455954176946,48.5199317919394));
#21742=CARTESIAN_POINT('',(29.625935174466,15.8580954176946,48.5199317919394));
#21743=CARTESIAN_POINT('',(29.625935174466,16.1705954176946,48.5199317919394));
#21744=CARTESIAN_POINT('',(29.625935174466,16.4830954176946,48.5199317919394));
#21745=CARTESIAN_POINT('',(40.162361854341,16.1705954176946,48.5199317919394));
#21746=CARTESIAN_POINT('',(40.162361854341,16.1705954176946,48.5199317919394));
#21747=CARTESIAN_POINT('',(40.162361854341,15.8580954176946,48.5199317919394));
#21748=CARTESIAN_POINT('',(40.162361854341,15.5455954176946,48.5199317919394));
#21749=CARTESIAN_POINT('',(26.1374820022305,15.8580954176946,48.5199317919394));
#21750=CARTESIAN_POINT('Origin',(0.0835265683620477,15.5455954176946,0.0824317919394229));
#21751=CARTESIAN_POINT('',(48.2085265683621,15.5455954176946,35.8884670232579));
#21752=CARTESIAN_POINT('',(46.958526568362,15.5455954176946,35.8884670232579));
#21753=CARTESIAN_POINT('',(0.0835265683620477,15.5455954176946,35.8884670232579));
#21754=CARTESIAN_POINT('',(48.2085265683621,15.5455954176946,29.6248403980433));
#21755=CARTESIAN_POINT('',(48.2085265683621,15.5455954176946,0.0824317919394229));
#21756=CARTESIAN_POINT('',(47.0528003113788,15.5455954176946,29.2947576203215));
#21757=CARTESIAN_POINT('Origin',(47.583526568362,15.5455954176946,29.6248403980433));
#21758=CARTESIAN_POINT('',(29.2958523967441,15.5455954176946,47.0517055349562));
#21759=CARTESIAN_POINT('Origin',(0.0835265683620477,15.5455954176946,0.0824317919394229));
#21760=CARTESIAN_POINT('',(29.625935174466,15.5455954176946,48.2074317919394));
#21761=CARTESIAN_POINT('Origin',(29.625935174466,15.5455954176946,47.5824317919394));
#21762=CARTESIAN_POINT('',(40.162361854341,15.5455954176946,48.2074317919394));
#21763=CARTESIAN_POINT('',(0.0835265683619977,15.5455954176946,48.2074317919394));
#21764=CARTESIAN_POINT('',(40.667792997167,15.5455954176946,47.2147847331159));
#21765=CARTESIAN_POINT('Origin',(40.162361854341,15.5455954176946,47.5824317919394));
#21766=CARTESIAN_POINT('Origin',(44.4585265683621,15.5455954176946,44.4574317919394));
#21767=CARTESIAN_POINT('',(46.9585265683621,15.5455954176946,38.3884670232579));
#21768=CARTESIAN_POINT('',(0.0835265683620477,15.5455954176946,38.3884670232579));
#21769=CARTESIAN_POINT('',(46.9585265683619,15.5455954176946,0.0824317919392602));
#21770=CARTESIAN_POINT('Origin',(29.625935174466,15.5455954176946,47.5824317919394));
#21771=CARTESIAN_POINT('Origin',(29.625935174466,15.8580954176946,47.5824317919394));
#21772=CARTESIAN_POINT('Origin',(29.625935174466,16.1705954176946,47.5824317919394));
#21773=CARTESIAN_POINT('Origin',(47.583526568362,15.5455954176946,40.1612670779183));
#21774=CARTESIAN_POINT('Origin',(40.162361854341,15.5455954176946,47.5824317919394));
#21775=CARTESIAN_POINT('Origin',(40.162361854341,15.8580954176946,47.5824317919394));
#21776=CARTESIAN_POINT('Origin',(40.162361854341,16.1705954176946,47.5824317919394));
#21777=CARTESIAN_POINT('Origin',(0.0835265683620477,-6.01690458230549,0.0824317919394229));
#21778=CARTESIAN_POINT('',(-31.5165682646525,-13.2959337131846,45.9710537470232));
#21779=CARTESIAN_POINT('',(-30.1626755346769,-13.2959337131846,46.8745131384048));
#21780=CARTESIAN_POINT('Origin',(0.0835265683620477,-13.2959337131846,0.0824317919394229));
#21781=CARTESIAN_POINT('',(-29.4155943178386,-12.6709337131846,46.6106860996161));
#21782=CARTESIAN_POINT('Ctrl Pts',(-30.1626755346769,-13.2959337131846,
46.8745131384048));
#21783=CARTESIAN_POINT('Ctrl Pts',(-30.128258496796,-13.2959337131846,46.8967601651148));
#21784=CARTESIAN_POINT('Ctrl Pts',(-30.0920298432681,-13.2919430659205,
46.9153675825233));
#21785=CARTESIAN_POINT('Ctrl Pts',(-30.0551006644128,-13.2842290832339,
46.929952148959));
#21786=CARTESIAN_POINT('Ctrl Pts',(-30.0180600299975,-13.2764918190586,
46.9445807329187));
#21787=CARTESIAN_POINT('Ctrl Pts',(-29.9803129154874,-13.2650083398877,
46.9551627917423));
#21788=CARTESIAN_POINT('Ctrl Pts',(-29.9429700957448,-13.2500137812989,
46.9612766845548));
#21789=CARTESIAN_POINT('Ctrl Pts',(-29.9293044928118,-13.244526523367,46.96351406331));
#21790=CARTESIAN_POINT('Ctrl Pts',(-29.9156930611522,-13.238568757885,46.9651526829848));
#21791=CARTESIAN_POINT('Ctrl Pts',(-29.9021905910678,-13.232151003965,46.9661704507551));
#21792=CARTESIAN_POINT('Ctrl Pts',(-29.9019147572162,-13.2320198995247,
46.9661912421216));
#21793=CARTESIAN_POINT('Ctrl Pts',(-29.9016389697338,-13.2318886036912,
46.9662117744956));
#21794=CARTESIAN_POINT('Ctrl Pts',(-29.9013632291097,-13.2317571165656,
46.9662320476885));
#21795=CARTESIAN_POINT('Ctrl Pts',(-29.8543113852301,-13.2093204091529,
46.9696914259059));
#21796=CARTESIAN_POINT('Ctrl Pts',(-29.8096740998552,-13.1821368365851,
46.9659209863793));
#21797=CARTESIAN_POINT('Ctrl Pts',(-29.7683137283865,-13.1520894283089,
46.9566376932634));
#21798=CARTESIAN_POINT('Ctrl Pts',(-29.7333029737206,-13.1266548782276,
46.9487795651511));
#21799=CARTESIAN_POINT('Ctrl Pts',(-29.7006405691595,-13.0991694705162,
46.9369724953244));
#21800=CARTESIAN_POINT('Ctrl Pts',(-29.670847712286,-13.0707895719797,46.92227614813));
#21801=CARTESIAN_POINT('Ctrl Pts',(-29.6705642512064,-13.0705195543472,
46.9221363212426));
#21802=CARTESIAN_POINT('Ctrl Pts',(-29.670281044226,-13.0702494422352,46.9219962204034));
#21803=CARTESIAN_POINT('Ctrl Pts',(-29.669998091945,-13.0699792367999,46.921855846619));
#21804=CARTESIAN_POINT('Ctrl Pts',(-29.649628163306,-13.0505269623229,46.9117502416691));
#21805=CARTESIAN_POINT('Ctrl Pts',(-29.6304171285035,-13.0305367697073,
46.9002697804115));
#21806=CARTESIAN_POINT('Ctrl Pts',(-29.6123668188922,-13.0101903794937,
46.8876291496845));
#21807=CARTESIAN_POINT('Ctrl Pts',(-29.6018341203628,-12.9983178743179,
46.8802531015425));
#21808=CARTESIAN_POINT('Ctrl Pts',(-29.5916957344855,-12.9863240855347,
46.8724825962677));
#21809=CARTESIAN_POINT('Ctrl Pts',(-29.5819448758312,-12.9742444051773,
46.8643639920203));
#21810=CARTESIAN_POINT('Ctrl Pts',(-29.5685981672066,-12.9577100691025,
46.853251468583));
#21811=CARTESIAN_POINT('Ctrl Pts',(-29.555981026384,-12.9410147689399,46.8414844826325));
#21812=CARTESIAN_POINT('Ctrl Pts',(-29.5440850848253,-12.9242496162066,
46.82917659869));
#21813=CARTESIAN_POINT('Ctrl Pts',(-29.538137114046,-12.9158670398399,46.8230226567187));
#21814=CARTESIAN_POINT('Ctrl Pts',(-29.5323694430285,-12.9074670004228,
46.8167334901675));
#21815=CARTESIAN_POINT('Ctrl Pts',(-29.5267810252359,-12.8990608878296,
46.810323293749));
#21816=CARTESIAN_POINT('Ctrl Pts',(-29.5211926074433,-12.8906547752363,
46.8039130973305));
#21817=CARTESIAN_POINT('Ctrl Pts',(-29.5157834428655,-12.8822425894822,
46.7973818710315));
#21818=CARTESIAN_POINT('Ctrl Pts',(-29.5105524846761,-12.8738357211132,
46.7907438089363));
#21819=CARTESIAN_POINT('Ctrl Pts',(-29.4940980968796,-12.8473912596422,
46.7698632658357));
#21820=CARTESIAN_POINT('Ctrl Pts',(-29.4792456474726,-12.8207472740157,
46.7477293519109));
#21821=CARTESIAN_POINT('Ctrl Pts',(-29.4659612746266,-12.7940681980352,
46.7245595323374));
#21822=CARTESIAN_POINT('Ctrl Pts',(-29.4623528891908,-12.7868214585523,
46.7182659992916));
#21823=CARTESIAN_POINT('Ctrl Pts',(-29.4588604654321,-12.7795722581758,
46.7118960192856));
#21824=CARTESIAN_POINT('Ctrl Pts',(-29.4554839045944,-12.7723242153339,
46.7054539678863));
#21825=CARTESIAN_POINT('Ctrl Pts',(-29.4432141529765,-12.745986266853,46.6820448322659));
#21826=CARTESIAN_POINT('Ctrl Pts',(-29.432470737787,-12.7196622748127,46.657684718712));
#21827=CARTESIAN_POINT('Ctrl Pts',(-29.4232215145298,-12.6935087390695,
46.6325807424414));
#21828=CARTESIAN_POINT('Ctrl Pts',(-29.420554704246,-12.6859679417359,46.6253425625187));
#21829=CARTESIAN_POINT('Ctrl Pts',(-29.4180123618763,-12.6784415052693,
46.6180426097208));
#21830=CARTESIAN_POINT('Ctrl Pts',(-29.4155943178386,-12.6709337131846,
46.6106860996161));
#21831=CARTESIAN_POINT('',(-27.2935253998822,-6.10843371318464,40.1519176123711));
#21832=CARTESIAN_POINT('Origin',(-79.3423351452487,-177.510308399964,197.496985230816));
#21833=CARTESIAN_POINT('',(-4.13722371802816,-6.1084337131593,48.4275653154203));
#21834=CARTESIAN_POINT('Origin',(0.0835265683620477,-6.10843371318469,0.0824317919394229));
#21835=CARTESIAN_POINT('',(-30.3451264940354,-14.6753754514266,48.394407142734));
#21836=CARTESIAN_POINT('Ctrl Pts',(-4.13722371861488,-6.10843371318471,
48.4275653153946));
#21837=CARTESIAN_POINT('Ctrl Pts',(-8.77470276505741,-6.50994980321315,
48.425735658919));
#21838=CARTESIAN_POINT('Ctrl Pts',(-13.2570072174814,-7.55645913600449,
48.420976017041));
#21839=CARTESIAN_POINT('Ctrl Pts',(-19.8170786877967,-9.80534906153842,
48.411872783885));
#21840=CARTESIAN_POINT('Ctrl Pts',(-21.9781883476615,-10.6692546575742,
48.4085130814623));
#21841=CARTESIAN_POINT('Ctrl Pts',(-26.2164003770554,-12.5596572871779,
48.4015713432632));
#21842=CARTESIAN_POINT('Ctrl Pts',(-28.295928291696,-13.58630787804,48.3979874291792));
#21843=CARTESIAN_POINT('Ctrl Pts',(-30.3451264940348,-14.6753754514262,
48.3944071427339));
#21844=CARTESIAN_POINT('',(-31.9648970362172,-14.6753754514262,47.3354574511386));
#21845=CARTESIAN_POINT('Origin',(0.0835265683620477,-14.6753754514262,0.0824317919394229));
#21846=CARTESIAN_POINT('Origin',(321.770247061695,-1402.95413116479,-1241.46399381397));
#21847=CARTESIAN_POINT('Origin',(-15.0075716891166,-11.0169045823054,-4.8938661154125));
#21848=CARTESIAN_POINT('',(-29.2671708193829,-11.3294045823054,38.3497289413026));
#21849=CARTESIAN_POINT('',(-15.0075716891166,-11.3294045823054,-4.8938661154125));
#21850=CARTESIAN_POINT('',(-29.2671708193829,-12.8919045823054,38.3497289413026));
#21851=CARTESIAN_POINT('',(-29.2671708193829,-11.0169045823054,38.3497289413026));
#21852=CARTESIAN_POINT('',(-29.4738806318652,-13.5169045823054,38.9765961725324));
#21853=CARTESIAN_POINT('Ctrl Pts',(-29.4738806318652,-13.5169045823054,
38.9765961725324));
#21854=CARTESIAN_POINT('Ctrl Pts',(-29.4622411026741,-13.516904574972,38.9412981895812));
#21855=CARTESIAN_POINT('Ctrl Pts',(-29.4506274187098,-13.5137764691089,
38.9060785847456));
#21856=CARTESIAN_POINT('Ctrl Pts',(-29.4391842642702,-13.5077394335828,
38.8713761269725));
#21857=CARTESIAN_POINT('Ctrl Pts',(-29.4269102353917,-13.501264055768,38.8341539631789));
#21858=CARTESIAN_POINT('Ctrl Pts',(-29.414832028346,-13.491442168195,38.797525647788));
#21859=CARTESIAN_POINT('Ctrl Pts',(-29.4031214538049,-13.4784883891823,
38.7620122130522));
#21860=CARTESIAN_POINT('Ctrl Pts',(-29.3912288722191,-13.4653332811037,
38.725946824586));
#21861=CARTESIAN_POINT('Ctrl Pts',(-29.3797149312961,-13.4489478321199,
38.6910297000638));
#21862=CARTESIAN_POINT('Ctrl Pts',(-29.3687598143315,-13.4295031815302,
38.6578072625039));
#21863=CARTESIAN_POINT('Ctrl Pts',(-29.3581606182668,-13.4106902683796,
38.6256641890356));
#21864=CARTESIAN_POINT('Ctrl Pts',(-29.3480841029937,-13.3890130654984,
38.5951061949253));
#21865=CARTESIAN_POINT('Ctrl Pts',(-29.3387004840658,-13.3645846069573,
38.5666494750863));
#21866=CARTESIAN_POINT('Ctrl Pts',(-29.3356538371499,-13.3566532439675,
38.5574102275847));
#21867=CARTESIAN_POINT('Ctrl Pts',(-29.332680314776,-13.3484315569536,38.5483927372337));
#21868=CARTESIAN_POINT('Ctrl Pts',(-29.3297860205605,-13.3399225829038,
38.5396155138337));
#21869=CARTESIAN_POINT('Ctrl Pts',(-29.3297548126056,-13.3398308342221,
38.5395208727323));
#21870=CARTESIAN_POINT('Ctrl Pts',(-29.329723613958,-13.3397390509054,38.5394262598562));
#21871=CARTESIAN_POINT('Ctrl Pts',(-29.3296924246223,-13.3396472329757,
38.5393316752196));
#21872=CARTESIAN_POINT('Ctrl Pts',(-29.3182021246964,-13.3058210699871,
38.5044862442188));
#21873=CARTESIAN_POINT('Ctrl Pts',(-29.3080231408104,-13.2674403223344,
38.4736175042842));
#21874=CARTESIAN_POINT('Ctrl Pts',(-29.2993846393367,-13.2257618864395,
38.4474204242529));
#21875=CARTESIAN_POINT('Ctrl Pts',(-29.294837188495,-13.2038216646352,38.433629845644));
#21876=CARTESIAN_POINT('Ctrl Pts',(-29.2907167715431,-13.1809667714828,
38.4211342880547));
#21877=CARTESIAN_POINT('Ctrl Pts',(-29.2870580654097,-13.1573764603981,
38.4100389125803));
#21878=CARTESIAN_POINT('Ctrl Pts',(-29.2811580163661,-13.1193345988007,
38.392146450855));
#21879=CARTESIAN_POINT('Ctrl Pts',(-29.2764567980797,-13.0793753611201,
38.377889557797));
#21880=CARTESIAN_POINT('Ctrl Pts',(-29.2731071107402,-13.0382175959962,
38.3677313113026));
#21881=CARTESIAN_POINT('Ctrl Pts',(-29.2698236342539,-12.9978733667247,
38.3577738555386));
#21882=CARTESIAN_POINT('Ctrl Pts',(-29.2678389416643,-12.9563778844883,
38.3517550858753));
#21883=CARTESIAN_POINT('Ctrl Pts',(-29.2673123516664,-12.9144212114036,
38.3501581514577));
#21884=CARTESIAN_POINT('Ctrl Pts',(-29.2672183185014,-12.906929009168,38.3498729869122));
#21885=CARTESIAN_POINT('Ctrl Pts',(-29.2671708205346,-12.899422137448,38.3497289447954));
#21886=CARTESIAN_POINT('Ctrl Pts',(-29.2671708193829,-12.8919045823054,
38.3497289413026));
#21887=CARTESIAN_POINT('',(-31.6880237676519,-13.5169045823054,45.6911965120565));
#21888=CARTESIAN_POINT('',(-15.0075716891166,-13.5169045823054,-4.8938661154125));
#21889=CARTESIAN_POINT('',(-31.9936964198019,-14.4544045724565,46.6181779979126));
#21890=CARTESIAN_POINT('Origin',(385.745342703142,-1402.30168122098,-1220.21532002388));
#21891=CARTESIAN_POINT('',(-15.0075716891166,-14.4544045823054,-4.8938661154125));
#21892=CARTESIAN_POINT('Origin',(-20.691141817304,-11.0169045823054,-6.76802647489269));
#21893=CARTESIAN_POINT('',(-34.064851465877,-12.8919045823054,33.7890241943272));
#21894=CARTESIAN_POINT('',(-34.064851465877,-11.3294045823054,33.7890241943272));
#21895=CARTESIAN_POINT('',(-34.064851465877,-11.0169045823054,33.7890241943272));
#21896=CARTESIAN_POINT('',(-20.691141817304,-11.3294045823054,-6.76802647489269));
#21897=CARTESIAN_POINT('',(-36.9407072266747,-14.4544045474394,42.5103312117922));
#21898=CARTESIAN_POINT('',(-37.2382104124512,-14.4544045823054,43.4125380113454));
#21899=CARTESIAN_POINT('',(-36.6209071624921,-13.5169045823054,41.5405070008967));
#21900=CARTESIAN_POINT('Origin',(151.814591741463,-669.972712918203,-529.908124501381));
#21901=CARTESIAN_POINT('',(-34.2850388610326,-13.5169045823054,34.4567634810854));
#21902=CARTESIAN_POINT('',(-34.2250213624229,-13.5169045823054,34.2747546894998));
#21903=CARTESIAN_POINT('Ctrl Pts',(-34.064851465877,-12.8919045823054,33.7890241943272));
#21904=CARTESIAN_POINT('Ctrl Pts',(-34.064851465877,-12.9240089539691,33.7890241943272));
#21905=CARTESIAN_POINT('Ctrl Pts',(-34.0657129309706,-12.9558011837999,
33.7916366694271));
#21906=CARTESIAN_POINT('Ctrl Pts',(-34.06740655103,-12.9870390822551,33.7967727338678));
#21907=CARTESIAN_POINT('Ctrl Pts',(-34.0691409907585,-13.0190298772458,
33.8020325878498));
#21908=CARTESIAN_POINT('Ctrl Pts',(-34.0717481240388,-13.0504387214823,
33.8099389683029));
#21909=CARTESIAN_POINT('Ctrl Pts',(-34.0751794302049,-13.0810143824546,
33.8203447316771));
#21910=CARTESIAN_POINT('Ctrl Pts',(-34.0775820070192,-13.1024232485175,
33.8276307751273));
#21911=CARTESIAN_POINT('Ctrl Pts',(-34.0803882878835,-13.1234238076895,
33.8361410896319));
#21912=CARTESIAN_POINT('Ctrl Pts',(-34.0835771201002,-13.1439346499851,
33.8458115276165));
#21913=CARTESIAN_POINT('Ctrl Pts',(-34.0835914891961,-13.1440270732421,
33.8458551032709));
#21914=CARTESIAN_POINT('Ctrl Pts',(-34.0836058650754,-13.1441194808469,
33.8458986994968));
#21915=CARTESIAN_POINT('Ctrl Pts',(-34.0836202477357,-13.144211872797,33.8459423162866));
#21916=CARTESIAN_POINT('Ctrl Pts',(-34.0950356695748,-13.2175427490952,
33.8805606723052));
#21917=CARTESIAN_POINT('Ctrl Pts',(-34.1107939452279,-13.2814833076597,
33.9283491469307));
#21918=CARTESIAN_POINT('Ctrl Pts',(-34.1300304689843,-13.3355724235347,
33.9866857408265));
#21919=CARTESIAN_POINT('Ctrl Pts',(-34.1313633525036,-13.3393202156014,
33.9907278372865));
#21920=CARTESIAN_POINT('Ctrl Pts',(-34.1327129398286,-13.3430206975228,
33.994820589631));
#21921=CARTESIAN_POINT('Ctrl Pts',(-34.1340789453017,-13.3466737099126,
33.9989631315761));
#21922=CARTESIAN_POINT('Ctrl Pts',(-34.134095506055,-13.3467179971709,33.999013353641));
#21923=CARTESIAN_POINT('Ctrl Pts',(-34.1341120683961,-13.346762275463,33.9990635805207));
#21924=CARTESIAN_POINT('Ctrl Pts',(-34.1341286323248,-13.3468065447897,
33.999113812215));
#21925=CARTESIAN_POINT('Ctrl Pts',(-34.1552239429207,-13.4031865990188,
34.0630873545708));
#21926=CARTESIAN_POINT('Ctrl Pts',(-34.1788849327196,-13.4450083105498,
34.1348415639403));
#21927=CARTESIAN_POINT('Ctrl Pts',(-34.2048318401454,-13.4738659092281,
34.2135280366445));
#21928=CARTESIAN_POINT('Ctrl Pts',(-34.230793136384,-13.502739510838,34.2922581447966));
#21929=CARTESIAN_POINT('Ctrl Pts',(-34.2575516483048,-13.5169045582356,
34.3734058855754));
#21930=CARTESIAN_POINT('Ctrl Pts',(-34.2850388610326,-13.5169045823054,
34.4567634810853));
#21931=CARTESIAN_POINT('Origin',(0.0835265683620477,-6.01690458230549,0.0824317919394229));
#21932=CARTESIAN_POINT('',(-48.2616071253848,-6.10843422628149,4.30318193353179));
#21933=CARTESIAN_POINT('',(-36.2923483131121,-6.10843371299756,32.2050468002929));
#21934=CARTESIAN_POINT('Origin',(0.0835265683620477,-6.10843371318468,0.0824317919394229));
#21935=CARTESIAN_POINT('',(-38.6155265946984,-12.6709337131846,39.2928878752488));
#21936=CARTESIAN_POINT('Ctrl Pts',(-36.2923483136832,-6.10843371318764,
32.2050467999334));
#21937=CARTESIAN_POINT('Ctrl Pts',(-36.4506972320925,-6.54712953976467,
32.6884882040633));
#21938=CARTESIAN_POINT('Ctrl Pts',(-36.6086641467873,-6.98698298246954,
33.1710153730752));
#21939=CARTESIAN_POINT('Ctrl Pts',(-36.7663605413492,-7.42790908708504,
33.6526450972576));
#21940=CARTESIAN_POINT('Ctrl Pts',(-36.9234404292421,-7.8671114117444,34.1323919125894));
#21941=CARTESIAN_POINT('Ctrl Pts',(-37.0802519669093,-8.30737802766575,
34.6112483736256));
#21942=CARTESIAN_POINT('Ctrl Pts',(-37.2368606662004,-8.74862497311526,
35.0892570131099));
#21943=CARTESIAN_POINT('Ctrl Pts',(-37.3931641879297,-9.18901207701331,
35.5663341748934));
#21944=CARTESIAN_POINT('Ctrl Pts',(-37.5492657202599,-9.63037569349855,
36.0425668828417));
#21945=CARTESIAN_POINT('Ctrl Pts',(-37.7051849081074,-10.0726323507207,
36.5180221740763));
#21946=CARTESIAN_POINT('Ctrl Pts',(-37.8606630015596,-10.5136378666595,
36.9921324053022));
#21947=CARTESIAN_POINT('Ctrl Pts',(-38.0159598214199,-10.9555313776692,
37.4654696724325));
#21948=CARTESIAN_POINT('Ctrl Pts',(-38.1710488404017,-11.3982301183212,
37.9381241297016));
#21949=CARTESIAN_POINT('Ctrl Pts',(-38.3194196408354,-11.8217518281929,
38.3903039204693));
#21950=CARTESIAN_POINT('Ctrl Pts',(-38.467599997085,-12.2460105160847,38.8418589612118));
#21951=CARTESIAN_POINT('Ctrl Pts',(-38.6155265946984,-12.6709337131846,
39.2928878752488));
#21952=CARTESIAN_POINT('',(-38.3314437206795,-13.2959337131846,40.4386168951447));
#21953=CARTESIAN_POINT('Ctrl Pts',(-38.3314437206796,-13.2959337131846,
40.4386168951445));
#21954=CARTESIAN_POINT('Ctrl Pts',(-38.366137334587,-13.2959336603242,40.4055920418474));
#21955=CARTESIAN_POINT('Ctrl Pts',(-38.3973537346038,-13.2916605128646,
40.369889537283));
#21956=CARTESIAN_POINT('Ctrl Pts',(-38.425468787648,-13.2840750781447,40.3324920189021));
#21957=CARTESIAN_POINT('Ctrl Pts',(-38.4579493281595,-13.2753118359295,
40.2892877038012));
#21958=CARTESIAN_POINT('Ctrl Pts',(-38.4862909067256,-13.2621273075482,
40.2438201501008));
#21959=CARTESIAN_POINT('Ctrl Pts',(-38.511035368168,-13.2459526169172,40.1975698652882));
#21960=CARTESIAN_POINT('Ctrl Pts',(-38.5182724521339,-13.2412219585235,
40.1840429111689));
#21961=CARTESIAN_POINT('Ctrl Pts',(-38.5252016095202,-13.236235270514,40.1704488680634));
#21962=CARTESIAN_POINT('Ctrl Pts',(-38.5318358717577,-13.2310278528739,
40.1568245667105));
#21963=CARTESIAN_POINT('Ctrl Pts',(-38.5318578376043,-13.2310106112677,
40.1567794570507));
#21964=CARTESIAN_POINT('Ctrl Pts',(-38.5318798002166,-13.2309933672421,
40.1567343470609));
#21965=CARTESIAN_POINT('Ctrl Pts',(-38.5319017595952,-13.2309761207983,
40.1566892367425));
#21966=CARTESIAN_POINT('Ctrl Pts',(-38.5756476076969,-13.1966190323616,
40.0668238005097));
#21967=CARTESIAN_POINT('Ctrl Pts',(-38.6064577978686,-13.1525556488358,
39.9756173439807));
#21968=CARTESIAN_POINT('Ctrl Pts',(-38.6271948516412,-13.1028429788279,
39.8861033242508));
#21969=CARTESIAN_POINT('Ctrl Pts',(-38.6296456164096,-13.0969677922401,
39.8755242994658));
#21970=CARTESIAN_POINT('Ctrl Pts',(-38.6319557285166,-13.091013740146,39.8649689297581));
#21971=CARTESIAN_POINT('Ctrl Pts',(-38.6341299442465,-13.0849875486837,
39.8544422340909));
#21972=CARTESIAN_POINT('Ctrl Pts',(-38.6341550963765,-13.0849178354768,
39.8543204573904));
#21973=CARTESIAN_POINT('Ctrl Pts',(-38.6341802298183,-13.0848481114876,
39.8541986834411));
#21974=CARTESIAN_POINT('Ctrl Pts',(-38.6342053445796,-13.0847783767298,
39.8540769122552));
#21975=CARTESIAN_POINT('Ctrl Pts',(-38.6393177094473,-13.0705831581647,
39.8292891499698));
#21976=CARTESIAN_POINT('Ctrl Pts',(-38.6436871904562,-13.0558793142743,
39.8044981508428));
#21977=CARTESIAN_POINT('Ctrl Pts',(-38.6473189003734,-13.0407301262923,
39.779789899109));
#21978=CARTESIAN_POINT('Ctrl Pts',(-38.6527932266981,-13.0178947125452,
39.7425454506291));
#21979=CARTESIAN_POINT('Ctrl Pts',(-38.6565923828782,-12.9940463246918,
39.7054863402387));
#21980=CARTESIAN_POINT('Ctrl Pts',(-38.658738720505,-12.9693962501975,39.6688952305503));
#21981=CARTESIAN_POINT('Ctrl Pts',(-38.6608850581318,-12.9447461757032,
39.6323041208619));
#21982=CARTESIAN_POINT('Ctrl Pts',(-38.6613785862668,-12.9192944015675,
39.5961810211914));
#21983=CARTESIAN_POINT('Ctrl Pts',(-38.6602417327113,-12.893252106151,39.5608086719037));
#21984=CARTESIAN_POINT('Ctrl Pts',(-38.6592756094922,-12.8711207892723,
39.530748469517));
#21985=CARTESIAN_POINT('Ctrl Pts',(-38.6571753247155,-12.8485482515866,
39.5011674516628));
#21986=CARTESIAN_POINT('Ctrl Pts',(-38.6538791596275,-12.8255048445994,
39.472089461548));
#21987=CARTESIAN_POINT('Ctrl Pts',(-38.6520037869991,-12.8123941618594,
39.4555453670344));
#21988=CARTESIAN_POINT('Ctrl Pts',(-38.6497405162343,-12.7991308725969,
39.4391646147524));
#21989=CARTESIAN_POINT('Ctrl Pts',(-38.6470721722362,-12.7857088195892,
39.4229563625242));
#21990=CARTESIAN_POINT('Ctrl Pts',(-38.6423111701721,-12.7617604748036,
39.394036732084));
#21991=CARTESIAN_POINT('Ctrl Pts',(-38.6362631824905,-12.7373067239694,
39.3656637812769));
#21992=CARTESIAN_POINT('Ctrl Pts',(-38.6288629041527,-12.7123167139536,
39.337863672571));
#21993=CARTESIAN_POINT('Ctrl Pts',(-38.6248258795218,-12.6986840799693,
39.3226980641349));
#21994=CARTESIAN_POINT('Ctrl Pts',(-38.6203857180183,-12.6848916910974,
39.3077033845067));
#21995=CARTESIAN_POINT('Ctrl Pts',(-38.6155265946984,-12.6709337131846,
39.2928878752488));
#21996=CARTESIAN_POINT('',(-37.0650186795419,-13.2959337131846,41.6073303993598));
#21997=CARTESIAN_POINT('Origin',(0.0835265683620477,-13.2959337131846,0.0824317919394229));
#21998=CARTESIAN_POINT('',(-37.5334874949993,-14.6753754514262,43.0348489817131));
#21999=CARTESIAN_POINT('Origin',(133.62398877783,-671.736422462057,-537.185659742862));
#22000=CARTESIAN_POINT('',(-48.2284489054473,-14.6753753060473,30.5110849318178));
#22001=CARTESIAN_POINT('Origin',(0.0835265683620477,-14.6753754514262,0.0824317919394229));
#22002=CARTESIAN_POINT('Ctrl Pts',(-48.2284492744908,-14.6753748699083,
30.5110851642587));
#22003=CARTESIAN_POINT('Ctrl Pts',(-48.2299633696893,-14.2165313283052,
29.6477376966094));
#22004=CARTESIAN_POINT('Ctrl Pts',(-48.2314726564589,-13.7688961376732,
28.7792612726429));
#22005=CARTESIAN_POINT('Ctrl Pts',(-48.2329717668262,-13.3339028926044,
27.9049951633218));
#22006=CARTESIAN_POINT('Ctrl Pts',(-48.2344282057187,-12.911291526629,27.0556146295442));
#22007=CARTESIAN_POINT('Ctrl Pts',(-48.2358750368302,-12.5006127516871,
26.2007692573981));
#22008=CARTESIAN_POINT('Ctrl Pts',(-48.2373071406924,-12.1031391972242,
25.3398789954832));
#22009=CARTESIAN_POINT('Ctrl Pts',(-48.2378382397359,-11.9557352063792,
25.0206158423475));
#22010=CARTESIAN_POINT('Ctrl Pts',(-48.2383673115233,-11.8101469172675,
24.7005215926836));
#22011=CARTESIAN_POINT('Ctrl Pts',(-48.2388940889699,-11.6664376689275,
24.3795676299112));
#22012=CARTESIAN_POINT('Ctrl Pts',(-48.2389469174388,-11.6520256252869,
24.3473804006859));
#22013=CARTESIAN_POINT('Ctrl Pts',(-48.2389997219701,-11.6376325718389,
24.315184473));
#22014=CARTESIAN_POINT('Ctrl Pts',(-48.2390525021121,-11.623258591744,24.2829798065931));
#22015=CARTESIAN_POINT('Ctrl Pts',(-48.2403190832725,-11.2783218088442,
23.5101546077717));
#22016=CARTESIAN_POINT('Ctrl Pts',(-48.2415701431461,-10.9443666874141,
22.732284950268));
#22017=CARTESIAN_POINT('Ctrl Pts',(-48.242796511321,-10.6225428069351,21.9488823033592));
#22018=CARTESIAN_POINT('Ctrl Pts',(-48.2432193628657,-10.511577985968,21.6787651997743));
#22019=CARTESIAN_POINT('Ctrl Pts',(-48.2436392818792,-10.4020550271772,
21.4079905277086));
#22020=CARTESIAN_POINT('Ctrl Pts',(-48.2440559020298,-10.2940198074422,
21.1365390135953));
#22021=CARTESIAN_POINT('Ctrl Pts',(-48.2440808777753,-10.2875432600572,
21.1202659074898));
#22022=CARTESIAN_POINT('Ctrl Pts',(-48.2441058419013,-10.2810720136179,
21.1039901109362));
#22023=CARTESIAN_POINT('Ctrl Pts',(-48.2441307942536,-10.274606093873,21.0877116651653));
#22024=CARTESIAN_POINT('Ctrl Pts',(-48.2448295961963,-10.0935250793195,
20.6318264095713));
#22025=CARTESIAN_POINT('Ctrl Pts',(-48.2455197694772,-9.91663263839809,
20.1739004285262));
#22026=CARTESIAN_POINT('Ctrl Pts',(-48.246199035224,-9.74425107310023,19.7141653273356));
#22027=CARTESIAN_POINT('Ctrl Pts',(-48.2468496559605,-9.5791389332757,19.2738175083628));
#22028=CARTESIAN_POINT('Ctrl Pts',(-48.2474902739655,-9.418164645248,18.831808477992));
#22029=CARTESIAN_POINT('Ctrl Pts',(-48.2481187813464,-9.26165511793492,
18.3883263777155));
#22030=CARTESIAN_POINT('Ctrl Pts',(-48.2483819011865,-9.19613359336515,
18.2026659656731));
#22031=CARTESIAN_POINT('Ctrl Pts',(-48.2486428968409,-9.13139516044456,
18.0167473119276));
#22032=CARTESIAN_POINT('Ctrl Pts',(-48.2489016051861,-9.06746659619111,
17.8305842623673));
#22033=CARTESIAN_POINT('Ctrl Pts',(-48.2489066096297,-9.06622996466504,
17.8269831319686));
#22034=CARTESIAN_POINT('Ctrl Pts',(-48.2489116131617,-9.06499364665102,
17.823381940484));
#22035=CARTESIAN_POINT('Ctrl Pts',(-48.2489166157804,-9.06375764243243,
17.8197806883051));
#22036=CARTESIAN_POINT('Ctrl Pts',(-48.2501226826645,-8.76577296160725,
16.9515652202961));
#22037=CARTESIAN_POINT('Ctrl Pts',(-48.2512776225182,-8.48534970208909,
16.0781073163287));
#22038=CARTESIAN_POINT('Ctrl Pts',(-48.252369512175,-8.22405492486658,15.1989747878282));
#22039=CARTESIAN_POINT('Ctrl Pts',(-48.2526503738063,-8.1568433005625,14.9728396700614));
#22040=CARTESIAN_POINT('Ctrl Pts',(-48.2529270615511,-8.09089757126633,
14.746329039514));
#22041=CARTESIAN_POINT('Ctrl Pts',(-48.2531993679279,-8.02624496071412,
14.5194354305203));
#22042=CARTESIAN_POINT('Ctrl Pts',(-48.2538215825573,-7.87851503755292,
14.0009880679757));
#22043=CARTESIAN_POINT('Ctrl Pts',(-48.2544211464411,-7.73745329659788,
13.4802335345385));
#22044=CARTESIAN_POINT('Ctrl Pts',(-48.2549947966408,-7.60353311381806,
12.957597846491));
#22045=CARTESIAN_POINT('Ctrl Pts',(-48.2555458288495,-7.47489316188283,
12.4555687393428));
#22046=CARTESIAN_POINT('Ctrl Pts',(-48.2560729487919,-7.35284273130093,
11.951803893176));
#22047=CARTESIAN_POINT('Ctrl Pts',(-48.2565734173535,-7.23775611983193,
11.4466902167293));
#22048=CARTESIAN_POINT('Ctrl Pts',(-48.2567519886166,-7.19669227855575,
11.2664615387687));
#22049=CARTESIAN_POINT('Ctrl Pts',(-48.2569271701239,-7.15651419471867,
11.0860593323825));
#22050=CARTESIAN_POINT('Ctrl Pts',(-48.2570988310731,-7.11724012340575,
10.9055143918711));
#22051=CARTESIAN_POINT('Ctrl Pts',(-48.2581343246436,-6.88033098059543,
9.81643078873517));
#22052=CARTESIAN_POINT('Ctrl Pts',(-48.2590418915315,-6.67627260268059,
8.72194948511542));
#22053=CARTESIAN_POINT('Ctrl Pts',(-48.2598002645257,-6.50737682473014,
7.62168683257795));
#22054=CARTESIAN_POINT('Ctrl Pts',(-48.2605586375199,-6.3384810467797,6.52142418004048));
#22055=CARTESIAN_POINT('Ctrl Pts',(-48.2611678149523,-6.20474805619726,
5.41538014167176));
#22056=CARTESIAN_POINT('Ctrl Pts',(-48.2616069309149,-6.10843510301187,
4.30318195855187));
#22057=CARTESIAN_POINT('Origin',(0.0835265683613308,-8.56135981233827,68.5199317919394));
#22058=CARTESIAN_POINT('',(-49.6039734316379,-8.56135981233827,22.7876789472102));
#22059=CARTESIAN_POINT('',(-49.603973431638,-8.56135981233827,44.4574317919389));
#22060=CARTESIAN_POINT('',(-49.603973431638,-8.56135981233827,68.5199317919394));
#22061=CARTESIAN_POINT('',(-44.2914734316384,-8.56135981233827,49.7699317919394));
#22062=CARTESIAN_POINT('Origin',(-44.2914734316384,-8.56135981233827,44.457431791939));
#22063=CARTESIAN_POINT('',(-22.6217205869088,-8.56135981233827,49.7699317919394));
#22064=CARTESIAN_POINT('',(0.0835265683613272,-8.56135981233827,49.7699317919394));
#22065=CARTESIAN_POINT('',(-37.6513250757669,-8.56135981233827,39.5850503890339));
#22066=CARTESIAN_POINT('Origin',(0.0835265683620477,-8.56135981233827,0.0824317919394229));
#22067=CARTESIAN_POINT('',(-38.8073463968985,-8.56135981233827,40.7410717101655));
#22068=CARTESIAN_POINT('',(-38.8073463968985,-8.56135981233827,40.7410717101655));
#22069=CARTESIAN_POINT('',(-40.5751133498648,-8.56135981233827,38.9733047571991));
#22070=CARTESIAN_POINT('Origin',(-39.6912298733817,-8.56135981233827,39.8571882336823));
#22071=CARTESIAN_POINT('',(-39.4190920287332,-8.56135981233827,37.8172834360675));
#22072=CARTESIAN_POINT('',(-39.3319744043414,-8.56135981233827,37.7301658116757));
#22073=CARTESIAN_POINT('Origin',(0.0835265683620477,-8.56135981233827,0.0824317919394229));
#22074=CARTESIAN_POINT('Origin',(0.0835265683615161,13.1261401876617,50.8324317919394));
#22075=CARTESIAN_POINT('',(-10.8649863601191,13.1261401876617,49.7699317919394));
#22076=CARTESIAN_POINT('',(-44.2914734316384,13.1261401876617,49.7699317919394));
#22077=CARTESIAN_POINT('',(0.0835265683615159,13.1261401876617,49.7699317919394));
#22078=CARTESIAN_POINT('',(-49.603973431638,13.1261401876617,44.4574317919389));
#22079=CARTESIAN_POINT('Origin',(-44.2914734316384,13.1261401876617,44.457431791939));
#22080=CARTESIAN_POINT('',(-49.603973431638,13.1261401876617,11.0309447204206));
#22081=CARTESIAN_POINT('',(-49.603973431638,13.1261401876617,50.8324317919394));
#22082=CARTESIAN_POINT('',(-36.7666959739419,13.1261401876617,35.1648873812763));
#22083=CARTESIAN_POINT('Origin',(0.0835265683620477,13.1261401876617,0.0824317919394229));
#22084=CARTESIAN_POINT('',(-40.5751133498648,13.1261401876617,38.9733047571991));
#22085=CARTESIAN_POINT('',(-34.9989290209756,13.1261401876617,36.9326543342427));
#22086=CARTESIAN_POINT('',(-34.9121356166459,13.1261401876617,36.845860929913));
#22087=CARTESIAN_POINT('Origin',(0.0835265683620477,13.1261401876617,0.0824317919394229));
#22088=CARTESIAN_POINT('Origin',(-44.2914734316384,16.4830954176946,44.457431791939));
#22089=CARTESIAN_POINT('Origin',(-44.2914734316384,-8.87385981233827,44.457431791939));
#22090=CARTESIAN_POINT('Origin',(-44.2914734316384,-14.4544045823054,44.457431791939));
#22091=CARTESIAN_POINT('Origin',(-44.2914734316384,16.4830954176946,44.457431791939));
#22092=CARTESIAN_POINT('Origin',(-44.2914734316384,13.4386401876617,44.457431791939));
#22093=CARTESIAN_POINT('Origin',(-44.2914734316384,16.1705954176946,44.457431791939));
#22094=CARTESIAN_POINT('Origin',(0.0835265683620477,16.4830954176946,0.0824317919394229));
#22095=CARTESIAN_POINT('',(-22.5100610938546,16.3915662868155,48.4076054027908));
#22096=CARTESIAN_POINT('',(-4.13722371782189,11.5746245485739,48.4275653154638));
#22097=CARTESIAN_POINT('Ctrl Pts',(-22.5100610938539,16.3915662868154,48.40760540279));
#22098=CARTESIAN_POINT('Ctrl Pts',(-19.5784539338831,15.1541680928392,48.4122678868286));
#22099=CARTESIAN_POINT('Ctrl Pts',(-16.5898434682929,14.0894359483377,48.4166153560574));
#22100=CARTESIAN_POINT('Ctrl Pts',(-11.9895027246046,12.8480220597895,48.4218969462028));
#22101=CARTESIAN_POINT('Ctrl Pts',(-10.4336967396725,12.4934998941785,48.4234490140686));
#22102=CARTESIAN_POINT('Ctrl Pts',(-7.30241537284812,11.9258476364963,48.4259690402679));
#22103=CARTESIAN_POINT('Ctrl Pts',(-5.72390896832624,11.7120008366799,48.4269393095598));
#22104=CARTESIAN_POINT('Ctrl Pts',(-4.13722371861483,11.5746245485739,48.4275653153946));
#22105=CARTESIAN_POINT('',(-48.261606955131,11.5746245485364,4.30318207805214));
#22106=CARTESIAN_POINT('Origin',(0.0835265683620477,11.5746245485738,0.0824317919394229));
#22107=CARTESIAN_POINT('',(-48.2416470424886,16.3915662868156,22.6760194541557));
#22108=CARTESIAN_POINT('Ctrl Pts',(-48.2616069550931,11.5746245485739,4.30318207891625));
#22109=CARTESIAN_POINT('Ctrl Pts',(-48.2609815027128,11.7118793817134,5.88846453338143));
#22110=CARTESIAN_POINT('Ctrl Pts',(-48.2600147804388,11.9249456441311,7.46165171918502));
#22111=CARTESIAN_POINT('Ctrl Pts',(-48.257503140552,12.4906656417943,10.5857557642485));
#22112=CARTESIAN_POINT('Ctrl Pts',(-48.2559560607416,12.843980457976,12.1389419888214));
#22113=CARTESIAN_POINT('Ctrl Pts',(-48.2506725111118,14.0856585112706,16.7448657488753));
#22114=CARTESIAN_POINT('Ctrl Pts',(-48.2463082137514,15.1545164964592,19.7452377217243));
#22115=CARTESIAN_POINT('Ctrl Pts',(-48.2416470424886,16.3915662868154,22.6760194541553));
#22116=CARTESIAN_POINT('Origin',(0.0835265683620477,16.3915662868154,0.0824317919394229));
#22117=CARTESIAN_POINT('Origin',(-41.0170550881064,16.4855954176946,39.8571882336823));
#22118=CARTESIAN_POINT('',(-35.9236748279974,-3.61941807409669,34.7638079735734));
#22119=CARTESIAN_POINT('',(-39.1981211596124,-8.24885981233827,38.0382543051883));
#22120=CARTESIAN_POINT('Ctrl Pts',(-35.9236748279974,-3.61941807409669,
34.7638079735734));
#22121=CARTESIAN_POINT('Ctrl Pts',(-36.4701860414282,-4.3920600802535,35.3103191870041));
#22122=CARTESIAN_POINT('Ctrl Pts',(-37.0166933027455,-5.16470767732066,
35.8568264483215));
#22123=CARTESIAN_POINT('Ctrl Pts',(-38.1081750882717,-6.70785538323106,
36.9483082338476));
#22124=CARTESIAN_POINT('Ctrl Pts',(-38.6531496305009,-7.47835546664591,
37.4932827760768));
#22125=CARTESIAN_POINT('Ctrl Pts',(-39.1981211596124,-8.24885981233827,
38.0382543051883));
#22126=CARTESIAN_POINT('',(-40.354142480744,-8.24885981233827,39.1942756263199));
#22127=CARTESIAN_POINT('',(-36.5457251048211,12.8136401876617,35.3858582503971));
#22128=CARTESIAN_POINT('',(-36.4589317004915,12.8136401876617,35.2990648460674));
#22129=CARTESIAN_POINT('',(-35.9236748279974,11.9341984494202,34.7638079735734));
#22130=CARTESIAN_POINT('',(-36.5457251048211,12.8136401876617,35.3858582503971));
#22131=CARTESIAN_POINT('',(-35.9236748279975,-3.74885981233827,34.7638079735734));
#22132=CARTESIAN_POINT('Origin',(-39.6912298733817,16.4855954176946,41.1830134484071));
#22133=CARTESIAN_POINT('',(-37.8722959448877,-8.24885981233827,39.3640795199131));
#22134=CARTESIAN_POINT('',(-37.7851783204959,-8.24885981233827,39.2769618955213));
#22135=CARTESIAN_POINT('',(-34.5978496132727,-3.61941807409669,36.0896331882982));
#22136=CARTESIAN_POINT('Ctrl Pts',(-37.8722959448877,-8.24885981233827,
39.3640795199131));
#22137=CARTESIAN_POINT('Ctrl Pts',(-37.3273244157762,-7.4783554666459,38.8191079908016));
#22138=CARTESIAN_POINT('Ctrl Pts',(-36.7823498735469,-6.70785538323104,
38.2741334485724));
#22139=CARTESIAN_POINT('Ctrl Pts',(-35.6908680880207,-5.16470767732064,
37.1826516630462));
#22140=CARTESIAN_POINT('Ctrl Pts',(-35.1443608267034,-4.39206008025349,
36.6361444017289));
#22141=CARTESIAN_POINT('Ctrl Pts',(-34.5978496132727,-3.61941807409669,
36.0896331882982));
#22142=CARTESIAN_POINT('',(-34.5978496132729,11.9341984494205,36.0896331882984));
#22143=CARTESIAN_POINT('',(-34.5978496132727,12.0636401876617,36.0896331882982));
#22144=CARTESIAN_POINT('',(-35.2198998900963,12.8136401876617,36.7116834651218));
#22145=CARTESIAN_POINT('',(-34.5978496132727,11.9341984494202,36.0896331882982));
#22146=CARTESIAN_POINT('',(-39.0283172660193,12.8136401876617,40.5201008410447));
#22147=CARTESIAN_POINT('Origin',(0.0835265683620477,-11.0169045823054,0.0824317919394229));
#22148=CARTESIAN_POINT('Origin',(0.0835265683620477,-14.4544045823054,0.0824317919394229));
#22149=CARTESIAN_POINT('Origin',(0.0835265683620477,-11.3294045823054,0.0824317919394229));
#22150=CARTESIAN_POINT('Origin',(0.0835265683620477,-13.2044045823054,0.0824317919394229));
#22151=CARTESIAN_POINT('',(-34.5818198379706,-13.2044045823054,34.3588997915592));
#22152=CARTESIAN_POINT('',(-36.9176881394301,-13.2044045823054,41.4426433113705));
#22153=CARTESIAN_POINT('',(-37.0041161457864,-13.2044045823054,41.7047444878682));
#22154=CARTESIAN_POINT('',(-38.1790905589799,-13.2044045823054,40.2785649063406));
#22155=CARTESIAN_POINT('Origin',(0.0835265683620477,-13.2044045823054,0.0824317919394229));
#22156=CARTESIAN_POINT('',(-35.8042963200226,-13.2044045823054,33.0767747666364));
#22157=CARTESIAN_POINT('',(-22.4718276789325,-13.2044045823054,-7.35520861204973));
#22158=CARTESIAN_POINT('Origin',(0.0835265683620477,-13.2044045823054,0.0824317919394229));
#22159=CARTESIAN_POINT('Origin',(-22.7686086558706,16.4855954176946,-7.4530723015759));
#22160=CARTESIAN_POINT('',(-38.1635245965525,-12.8919045823054,39.2334793180968));
#22161=CARTESIAN_POINT('',(-22.7686086558706,-12.8919045823054,-7.4530723015759));
#22162=CARTESIAN_POINT('Ctrl Pts',(-38.1635245965525,-12.8919045823054,
39.2334793180967));
#22163=CARTESIAN_POINT('Ctrl Pts',(-37.6189300816584,-11.3339023360117,
37.5819444848208));
#22164=CARTESIAN_POINT('Ctrl Pts',(-37.0718575407512,-9.78474033410477,
35.9228948011991));
#22165=CARTESIAN_POINT('Ctrl Pts',(-36.52139118477,-8.24794399907487,34.2535530495173));
#22166=CARTESIAN_POINT('Ctrl Pts',(-36.3815123036638,-7.85742903027376,
33.8293569948958));
#22167=CARTESIAN_POINT('Ctrl Pts',(-36.2414142252472,-7.46771271925601,
33.4044962035141));
#22168=CARTESIAN_POINT('Ctrl Pts',(-36.1010818023558,-7.07885337125988,
32.9789247401509));
#22169=CARTESIAN_POINT('Origin',(0.0835265683620477,-13.2044045823054,0.0824317919394229));
#22170=CARTESIAN_POINT('',(-27.8490907775129,-13.2044045823054,40.036547827824));
#22171=CARTESIAN_POINT('',(-30.0427195777899,-13.2044045823054,46.6889364873753));
#22172=CARTESIAN_POINT('',(-30.1097879334595,-13.2044045823054,46.8923276758091));
#22173=CARTESIAN_POINT('',(-31.3912427907138,-13.2044045823054,45.7890602015826));
#22174=CARTESIAN_POINT('Origin',(0.0835265683620477,-13.2044045823054,0.0824317919394229));
#22175=CARTESIAN_POINT('',(-29.1770996549271,-13.2044045823054,39.0744598620586));
#22176=CARTESIAN_POINT('',(-14.7107907121785,-13.2044045823054,-4.79600242588632));
#22177=CARTESIAN_POINT('Origin',(0.0835265683620477,-13.2044045823054,0.0824317919394229));
#22178=CARTESIAN_POINT('Origin',(-12.93010485055,16.4855954176946,-4.20882028872929));
#22179=CARTESIAN_POINT('',(-27.5523098005748,-12.8919045823054,40.1344115173502));
#22180=CARTESIAN_POINT('',(-27.5523098389671,-6.59535001059396,40.1344116337787));
#22181=CARTESIAN_POINT('',(-27.5523098005748,-6.01690458230549,40.1344115173502));
#22182=CARTESIAN_POINT('',(-29.5940549924842,-12.8919045823054,46.326198641332));
#22183=CARTESIAN_POINT('Ctrl Pts',(-27.5523099865879,-6.59534981976455,
40.1344120814527));
#22184=CARTESIAN_POINT('Ctrl Pts',(-28.2344318423759,-8.68909917314417,
42.2030116992655));
#22185=CARTESIAN_POINT('Ctrl Pts',(-28.914831114185,-10.7885698299828,44.266387416788));
#22186=CARTESIAN_POINT('Ctrl Pts',(-29.5940549924842,-12.8919045823054,
46.326198641332));
#22187=CARTESIAN_POINT('',(-27.4793257777183,-12.8919045823054,39.9130805036812));
#22188=CARTESIAN_POINT('Origin',(0.0835265683620477,15.5455954176946,0.0824317919394229));
#22189=CARTESIAN_POINT('',(-46.6203840461634,16.1705954176946,29.1297162314601));
#22190=CARTESIAN_POINT('Origin',(0.0835265683620477,16.1705954176946,0.0824317919394229));
#22191=CARTESIAN_POINT('',(-46.6203840461634,15.8580954176946,29.1297162314601));
#22192=CARTESIAN_POINT('',(-46.6203840461634,15.5455954176946,29.1297162314601));
#22193=CARTESIAN_POINT('Origin',(0.0835265683620477,15.8580954176946,0.0824317919394229));
#22194=CARTESIAN_POINT('Origin',(-42.6676757995426,15.5455954176946,48.519931791939));
#22195=CARTESIAN_POINT('',(-39.9953087176173,15.8580954176946,48.519931791939));
#22196=CARTESIAN_POINT('',(-39.9953087176173,16.1705954176946,48.519931791939));
#22197=CARTESIAN_POINT('',(-39.9953087176173,16.4830954176946,48.519931791939));
#22198=CARTESIAN_POINT('',(-29.4588820377423,16.1705954176946,48.5199317919391));
#22199=CARTESIAN_POINT('',(-42.6676757995426,15.8580954176946,48.519931791939));
#22200=CARTESIAN_POINT('Origin',(-48.3539734316382,15.5455954176946,26.1363872258074));
#22201=CARTESIAN_POINT('',(-48.3539734316382,15.8580954176946,29.6248403980428));
#22202=CARTESIAN_POINT('',(-48.3539734316382,16.1705954176946,29.6248403980428));
#22203=CARTESIAN_POINT('',(-48.3539734316382,16.4830954176946,29.6248403980428));
#22204=CARTESIAN_POINT('',(-48.3539734316384,16.1705954176946,40.1612670779178));
#22205=CARTESIAN_POINT('',(-48.3539734316384,15.5455954176946,40.1612670779178));
#22206=CARTESIAN_POINT('',(-48.3539734316382,15.8580954176946,26.1363872258074));
#22207=CARTESIAN_POINT('Origin',(0.0835265683620477,15.5455954176946,0.0824317919394229));
#22208=CARTESIAN_POINT('',(-40.5007398604433,15.5455954176946,47.2147847331155));
#22209=CARTESIAN_POINT('Origin',(-44.2914734316384,15.5455954176946,44.457431791939));
#22210=CARTESIAN_POINT('',(-39.9953087176173,15.5455954176946,48.207431791939));
#22211=CARTESIAN_POINT('Origin',(-39.9953087176173,15.5455954176946,47.582431791939));
#22212=CARTESIAN_POINT('',(-29.4588820377423,15.5455954176946,48.2074317919391));
#22213=CARTESIAN_POINT('',(0.0835265683615436,15.5455954176946,48.2074317919394));
#22214=CARTESIAN_POINT('',(-29.1287992600205,15.5455954176946,47.0517055349559));
#22215=CARTESIAN_POINT('Origin',(-29.4588820377423,15.5455954176946,47.5824317919391));
#22216=CARTESIAN_POINT('',(-46.885747174655,15.5455954176946,29.294757620321));
#22217=CARTESIAN_POINT('Origin',(0.0835265683620477,15.5455954176946,0.0824317919394229));
#22218=CARTESIAN_POINT('',(-48.0414734316383,15.5455954176946,29.6248403980429));
#22219=CARTESIAN_POINT('Origin',(-47.4164734316383,15.5455954176946,29.6248403980429));
#22220=CARTESIAN_POINT('',(-48.0414734316379,15.5455954176946,0.0824317919388688));
#22221=CARTESIAN_POINT('Origin',(-47.4164734316383,15.5455954176946,29.6248403980429));
#22222=CARTESIAN_POINT('Origin',(-47.4164734316383,15.8580954176946,29.6248403980429));
#22223=CARTESIAN_POINT('Origin',(-47.4164734316383,16.1705954176946,29.6248403980429));
#22224=CARTESIAN_POINT('Origin',(-39.9953087176173,15.5455954176946,47.582431791939));
#22225=CARTESIAN_POINT('Origin',(-39.9953087176173,15.8580954176946,47.582431791939));
#22226=CARTESIAN_POINT('Origin',(-39.9953087176173,16.1705954176946,47.582431791939));
#22227=CARTESIAN_POINT('Origin',(-47.4164734316384,15.5455954176946,40.1612670779178));
#22228=CARTESIAN_POINT('Origin',(-44.2914734316384,16.1705954176946,44.457431791939));
#22229=CARTESIAN_POINT('Origin',(-41.0061710032694,16.1705954176946,46.8471376742919));
#22230=CARTESIAN_POINT('Origin',(-39.9953087176173,16.1705954176946,47.582431791939));
#22231=CARTESIAN_POINT('Origin',(-39.9953087176173,16.1705954176946,48.832431791939));
#22232=CARTESIAN_POINT('Origin',(-42.6676757995426,16.1705954176946,48.832431791939));
#22233=CARTESIAN_POINT('Origin',(-29.4588820377424,16.1705954176946,48.8324317919391));
#22234=CARTESIAN_POINT('Origin',(-48.6664734316382,16.1705954176946,26.1363872258074));
#22235=CARTESIAN_POINT('Origin',(-48.6664734316382,16.1705954176946,29.6248403980428));
#22236=CARTESIAN_POINT('Origin',(-29.4588820377423,16.1705954176946,47.5824317919391));
#22237=CARTESIAN_POINT('Origin',(-28.7987164822987,16.1705954176946,46.5209792779726));
#22238=CARTESIAN_POINT('Origin',(-47.4164734316383,16.1705954176946,29.6248403980429));
#22239=CARTESIAN_POINT('Origin',(-46.3550209176718,16.1705954176946,28.9646748425992));
#22240=CARTESIAN_POINT('Origin',(0.0835265683620477,16.1705954176946,0.0824317919394229));
#22241=CARTESIAN_POINT('Origin',(-44.2914734316384,15.8580954176946,44.457431791939));
#22242=CARTESIAN_POINT('Origin',(-40.5007398604433,15.8580954176946,47.2147847331155));
#22243=CARTESIAN_POINT('Origin',(-39.9953087176173,15.8580954176946,47.582431791939));
#22244=CARTESIAN_POINT('Origin',(-39.9953087176173,15.8580954176946,48.207431791939));
#22245=CARTESIAN_POINT('Origin',(0.0835265683615436,15.8580954176946,48.2074317919394));
#22246=CARTESIAN_POINT('Origin',(-29.4588820377423,15.8580954176946,48.2074317919391));
#22247=CARTESIAN_POINT('Origin',(-48.0414734316379,15.8580954176946,0.0824317919388688));
#22248=CARTESIAN_POINT('Origin',(-48.0414734316382,15.8580954176946,29.6248403980429));
#22249=CARTESIAN_POINT('Origin',(-29.4588820377423,15.8580954176946,47.5824317919391));
#22250=CARTESIAN_POINT('Origin',(-29.1287992600205,15.8580954176946,47.0517055349559));
#22251=CARTESIAN_POINT('Origin',(-47.4164734316383,15.8580954176946,29.6248403980429));
#22252=CARTESIAN_POINT('Origin',(-46.885747174655,15.8580954176946,29.294757620321));
#22253=CARTESIAN_POINT('Origin',(0.0835265683620477,15.8580954176946,0.0824317919394229));
#22254=CARTESIAN_POINT('Ctrl Pts',(0.0835265683815503,-6.00666333723547,
48.5199460669664));
#22255=CARTESIAN_POINT('Ctrl Pts',(0.434571873255604,-6.0013252951217,48.519945950593));
#22256=CARTESIAN_POINT('Ctrl Pts',(0.78566911589282,-5.99973567328053,48.5184885224505));
#22257=CARTESIAN_POINT('Ctrl Pts',(1.48799467904377,-5.99820579736959,48.508757702106));
#22258=CARTESIAN_POINT('Ctrl Pts',(1.83922299955751,-5.99826554329982,48.5004843099039));
#22259=CARTESIAN_POINT('Ctrl Pts',(2.54183792081169,-5.99418693015785,48.4732202209189));
#22260=CARTESIAN_POINT('Ctrl Pts',(2.89280484433907,-5.99381953117288,48.4556040546384));
#22261=CARTESIAN_POINT('Ctrl Pts',(3.59436240935176,-5.99717808806743,48.4131737559656));
#22262=CARTESIAN_POINT('Ctrl Pts',(3.94495305083707,-6.00090404394696,48.3883596235733));
#22263=CARTESIAN_POINT('Ctrl Pts',(4.29550794738001,-6.007051447105,48.3603316468569));
#22264=CARTESIAN_POINT('Ctrl Pts',(0.0835265683810243,-5.9853111687807,
48.5199456014727));
#22265=CARTESIAN_POINT('Ctrl Pts',(0.356716052653991,-5.98270666392053,
48.5198859104315));
#22266=CARTESIAN_POINT('Ctrl Pts',(0.652301278133249,-5.98152768121034,
48.5186918880741));
#22267=CARTESIAN_POINT('Ctrl Pts',(1.29495516994804,-5.97907559060103,48.5103258778986));
#22268=CARTESIAN_POINT('Ctrl Pts',(1.64203235073192,-5.97774718230165,48.5030276183598));
#22269=CARTESIAN_POINT('Ctrl Pts',(2.39436889948374,-5.97194742955331,48.4746917382514));
#22270=CARTESIAN_POINT('Ctrl Pts',(2.76993041040138,-5.97081802552572,48.455949685341));
#22271=CARTESIAN_POINT('Ctrl Pts',(3.5267082710891,-5.97321241327176,48.409676657807));
#22272=CARTESIAN_POINT('Ctrl Pts',(3.90792462085919,-5.97673620504541,48.3821456831835));
#22273=CARTESIAN_POINT('Ctrl Pts',(4.29540257294,-5.98314272027373,48.3503998997031));
#22274=CARTESIAN_POINT('Ctrl Pts',(0.0835265683704475,-5.96223275463529,
48.5195872927805));
#22275=CARTESIAN_POINT('Ctrl Pts',(0.339530012943145,-5.96240686080331,
48.5196215918919));
#22276=CARTESIAN_POINT('Ctrl Pts',(0.626534465003536,-5.96239709811646,
48.5182575867091));
#22277=CARTESIAN_POINT('Ctrl Pts',(1.26276365256779,-5.96099214798698,48.509167391216));
#22278=CARTESIAN_POINT('Ctrl Pts',(1.61199486653157,-5.95954166014411,48.5013148775363));
#22279=CARTESIAN_POINT('Ctrl Pts',(2.3728618208734,-5.95413393118491,48.4721918658653));
#22280=CARTESIAN_POINT('Ctrl Pts',(2.75490258993289,-5.95257589046813,48.4528734062177));
#22281=CARTESIAN_POINT('Ctrl Pts',(3.52251156374742,-5.95314193699468,48.4051808771888));
#22282=CARTESIAN_POINT('Ctrl Pts',(3.90807774412224,-5.95526602423799,48.3768070663115));
#22283=CARTESIAN_POINT('Ctrl Pts',(4.29560464263447,-5.95992641567859,48.3444127441005));
#22284=CARTESIAN_POINT('Ctrl Pts',(0.0835265683683665,-5.92795641804995,
48.5154826407816));
#22285=CARTESIAN_POINT('Ctrl Pts',(0.36133241049536,-5.92787973562297,48.5154600083354));
#22286=CARTESIAN_POINT('Ctrl Pts',(0.667559641547024,-5.92723732580272,
48.5133469044261));
#22287=CARTESIAN_POINT('Ctrl Pts',(1.32724155701544,-5.92511301754089,48.5020950495901));
#22288=CARTESIAN_POINT('Ctrl Pts',(1.68069642931525,-5.92360346889918,48.4928930594121));
#22289=CARTESIAN_POINT('Ctrl Pts',(2.42513999617731,-5.91998502842382,48.4637155122407));
#22290=CARTESIAN_POINT('Ctrl Pts',(2.80138061701086,-5.91860436677903,48.4445443128851));
#22291=CARTESIAN_POINT('Ctrl Pts',(3.55227792514613,-5.91737158402242,48.3973032871643));
#22292=CARTESIAN_POINT('Ctrl Pts',(3.92693056632441,-5.91751946291059,48.369233977527));
#22293=CARTESIAN_POINT('Ctrl Pts',(4.29606146924342,-5.91876732373882,48.3374043064722));
#22294=CARTESIAN_POINT('Ctrl Pts',(0.0835265683679874,-5.90583775506839,
48.5199317919394));
#22295=CARTESIAN_POINT('Ctrl Pts',(0.400320847750857,-5.9058377550684,48.5199317919394));
#22296=CARTESIAN_POINT('Ctrl Pts',(0.734351631213873,-5.90562906540037,
48.5168141308035));
#22297=CARTESIAN_POINT('Ctrl Pts',(1.42391097883914,-5.90495067814671,48.5026532295386));
#22298=CARTESIAN_POINT('Ctrl Pts',(1.77943547629603,-5.90448098056109,48.4916098859256));
#22299=CARTESIAN_POINT('Ctrl Pts',(2.49892525008987,-5.90343694889075,48.4610292841221));
#22300=CARTESIAN_POINT('Ctrl Pts',(2.86288646455625,-5.90286261480602,48.4414922321787));
#22301=CARTESIAN_POINT('Ctrl Pts',(3.58624099388631,-5.90176568155595,48.3944770847012));
#22302=CARTESIAN_POINT('Ctrl Pts',(3.94563026526353,-5.9012430823906,48.3669995056144));
#22303=CARTESIAN_POINT('Ctrl Pts',(4.2963162261579,-5.90082453639418,48.3363830244465));
#22304=CARTESIAN_POINT('Ctrl Pts',(0.0835265683620106,-5.88746284406389,
48.5199317919394));
#22305=CARTESIAN_POINT('Ctrl Pts',(0.43481398105989,-5.88746284406389,48.5199317919394));
#22306=CARTESIAN_POINT('Ctrl Pts',(0.786101399028904,-5.88746284406389,
48.5161104362146));
#22307=CARTESIAN_POINT('Ctrl Pts',(1.48859334813907,-5.88746284406389,48.50082319184));
#22308=CARTESIAN_POINT('Ctrl Pts',(1.8397978898232,-5.88746284406389,48.489357302818));
#22309=CARTESIAN_POINT('Ctrl Pts',(2.5420408938028,-5.88746284406389,48.4587755322629));
#22310=CARTESIAN_POINT('Ctrl Pts',(2.89307936664319,-5.88746284406389,48.439659649984));
#22311=CARTESIAN_POINT('Ctrl Pts',(3.59490640778672,-5.88746284406389,48.3937688119853));
#22312=CARTESIAN_POINT('Ctrl Pts',(3.9456949866378,-5.88746284406389,48.3669938551438));
#22313=CARTESIAN_POINT('Ctrl Pts',(4.2963162261579,-5.88746284406389,48.3363830244465));
#22314=CARTESIAN_POINT('',(0.0835265683815503,-6.00666333723547,48.5199460669664));
#22315=CARTESIAN_POINT('Ctrl Pts',(0.0835265683620321,-5.88746284406389,
48.5199317919394));
#22316=CARTESIAN_POINT('Ctrl Pts',(0.0835265683679874,-5.90583775506839,
48.5199317919394));
#22317=CARTESIAN_POINT('Ctrl Pts',(0.0835265683683665,-5.92795641804995,
48.5154826407816));
#22318=CARTESIAN_POINT('Ctrl Pts',(0.0835265683704475,-5.96223275463529,
48.5195872927805));
#22319=CARTESIAN_POINT('Ctrl Pts',(0.0835265683810243,-5.9853111687807,
48.5199456014727));
#22320=CARTESIAN_POINT('Ctrl Pts',(0.0835265683815503,-6.00666333723547,
48.5199460669664));
#22321=CARTESIAN_POINT('',(4.29550794738001,-6.00705144710501,48.360331646857));
#22322=CARTESIAN_POINT('Ctrl Pts',(4.2963162261579,-5.88746284406389,48.3363830244465));
#22323=CARTESIAN_POINT('Ctrl Pts',(4.2963162261579,-5.89466520940775,48.3363830244465));
#22324=CARTESIAN_POINT('Ctrl Pts',(4.2962385509138,-5.90314351486558,48.3366383003061));
#22325=CARTESIAN_POINT('Ctrl Pts',(4.29613103097065,-5.9126635514535,48.3374208419226));
#22326=CARTESIAN_POINT('Ctrl Pts',(4.29603170548146,-5.92145803425842,48.338143743429));
#22327=CARTESIAN_POINT('Ctrl Pts',(4.29590711917709,-5.93114147445235,48.339318986334));
#22328=CARTESIAN_POINT('Ctrl Pts',(4.29579418047257,-5.94148964487015,48.3411521533193));
#22329=CARTESIAN_POINT('Ctrl Pts',(4.29568497044383,-5.95149617003368,48.3429247982243));
#22330=CARTESIAN_POINT('Ctrl Pts',(4.29558678798446,-5.96212379582482,48.3453142106815));
#22331=CARTESIAN_POINT('Ctrl Pts',(4.29552981876319,-5.97313476325662,48.3484700316399));
#22332=CARTESIAN_POINT('Ctrl Pts',(4.29547705488659,-5.98333292489416,48.3513928967225));
#22333=CARTESIAN_POINT('Ctrl Pts',(4.29545968136764,-5.99385899411772,48.354973634109));
#22334=CARTESIAN_POINT('Ctrl Pts',(4.29549777905033,-6.00450404015459,48.3592865236346));
#22335=CARTESIAN_POINT('Ctrl Pts',(4.29550081548163,-6.00535246317496,48.3596302661365));
#22336=CARTESIAN_POINT('Ctrl Pts',(4.29550420195006,-6.00620163512509,48.3599786327558));
#22337=CARTESIAN_POINT('Ctrl Pts',(4.29550794738001,-6.00705144710501,48.360331646857));
#22338=CARTESIAN_POINT('Ctrl Pts',(4.29550794738001,-6.00705144710501,48.360331646857));
#22339=CARTESIAN_POINT('Ctrl Pts',(3.59439815429413,-5.99475664078893,48.4163876002896));
#22340=CARTESIAN_POINT('Ctrl Pts',(2.89314538143878,-5.99214762358687,48.4595881764264));
#22341=CARTESIAN_POINT('Ctrl Pts',(1.48791553893041,-6.0003048498708,48.5141163543965));
#22342=CARTESIAN_POINT('Ctrl Pts',(0.785617178129657,-5.99598725300791,
48.5199458342196));
#22343=CARTESIAN_POINT('Ctrl Pts',(0.0835265683815503,-6.00666333723547,
48.5199460669664));
#22344=CARTESIAN_POINT('Ctrl Pts',(0.0835265683815503,-6.00666333723547,
48.5199460669664));
#22345=CARTESIAN_POINT('Ctrl Pts',(0.434571873255867,-6.01200137934908,
48.5199461833399));
#22346=CARTESIAN_POINT('Ctrl Pts',(0.785441202115477,-6.02125184123583,
48.5184889915199));
#22347=CARTESIAN_POINT('Ctrl Pts',(1.48685396085203,-6.04818290219913,48.5151613829932));
#22348=CARTESIAN_POINT('Ctrl Pts',(1.83739739072896,-6.06586350127568,48.5132909662866));
#22349=CARTESIAN_POINT('Ctrl Pts',(2.88857791145589,-6.13245845075531,48.5108119660871));
#22350=CARTESIAN_POINT('Ctrl Pts',(3.59085026662451,-6.17306838545285,48.5061181031007));
#22351=CARTESIAN_POINT('Ctrl Pts',(4.29256571553473,-6.20946968450873,48.4959174422579));
#22352=CARTESIAN_POINT('Ctrl Pts',(0.434571873255604,-6.0013252951217,48.519945950593));
#22353=CARTESIAN_POINT('Ctrl Pts',(0.707588293216581,-6.00879525432306,
48.5190043349161));
#22354=CARTESIAN_POINT('Ctrl Pts',(0.99833096149102,-6.01828947675665,48.5172889554697));
#22355=CARTESIAN_POINT('Ctrl Pts',(1.61221600115967,-6.04432658407314,48.5134046445675));
#22356=CARTESIAN_POINT('Ctrl Pts',(1.93535675298704,-6.06089216512314,48.5112385621328));
#22357=CARTESIAN_POINT('Ctrl Pts',(2.94880361840312,-6.12571278894254,48.5075991346784));
#22358=CARTESIAN_POINT('Ctrl Pts',(3.62682139079342,-6.16367997403223,48.5021196905958));
#22359=CARTESIAN_POINT('Ctrl Pts',(4.29322406284948,-6.19747947412217,48.4909193590357));
#22360=CARTESIAN_POINT('Ctrl Pts',(0.78566911589282,-5.99973567328053,48.5184885224505));
#22361=CARTESIAN_POINT('Ctrl Pts',(0.998676155525609,-6.00835114797884,
48.5169166777064));
#22362=CARTESIAN_POINT('Ctrl Pts',(1.24336152129271,-6.01789996842701,48.5149008816205));
#22363=CARTESIAN_POINT('Ctrl Pts',(1.78640027159867,-6.04289085428944,48.5103147763974));
#22364=CARTESIAN_POINT('Ctrl Pts',(2.08475122678728,-6.05836696395433,48.5077487407917));
#22365=CARTESIAN_POINT('Ctrl Pts',(3.04577953853793,-6.11975101512501,48.5025662257011));
#22366=CARTESIAN_POINT('Ctrl Pts',(3.68879008339862,-6.15479195325804,48.4962278198683));
#22367=CARTESIAN_POINT('Ctrl Pts',(4.29389279897283,-6.18527410484422,48.4847891628839));
#22368=CARTESIAN_POINT('Ctrl Pts',(1.48799467904377,-5.99820579736959,48.508757702106));
#22369=CARTESIAN_POINT('Ctrl Pts',(1.61377824566997,-6.00829173506077,48.5070409830128));
#22370=CARTESIAN_POINT('Ctrl Pts',(1.78770681959273,-6.01814206512117,48.505001360523));
#22371=CARTESIAN_POINT('Ctrl Pts',(2.21034411610889,-6.04173521008607,48.4999506928767));
#22372=CARTESIAN_POINT('Ctrl Pts',(2.45904980201447,-6.05552058030387,48.4969449896348));
#22373=CARTESIAN_POINT('Ctrl Pts',(3.28508024419413,-6.10935599904099,48.4895414181676));
#22374=CARTESIAN_POINT('Ctrl Pts',(3.8343859391826,-6.13882811018934,48.4820050858304));
#22375=CARTESIAN_POINT('Ctrl Pts',(4.29532856800228,-6.16205725113852,48.4713889284506));
#22376=CARTESIAN_POINT('Ctrl Pts',(1.83922299955751,-5.99826554329982,48.5004843099039));
#22377=CARTESIAN_POINT('Ctrl Pts',(1.93779750844287,-6.00864450579839,48.4992338112119));
#22378=CARTESIAN_POINT('Ctrl Pts',(2.0870291104974,-6.0187257861122,48.4974612117992));
#22379=CARTESIAN_POINT('Ctrl Pts',(2.46011313068803,-6.04195544062546,48.4926406006817));
#22380=CARTESIAN_POINT('Ctrl Pts',(2.68396271458218,-6.05514353311732,48.4895975747639));
#22381=CARTESIAN_POINT('Ctrl Pts',(3.42741006465308,-6.10489083408599,48.4815303852945));
#22382=CARTESIAN_POINT('Ctrl Pts',(3.91801310236138,-6.13175228789483,48.4736742225201));
#22383=CARTESIAN_POINT('Ctrl Pts',(4.29609560090838,-6.15104576671075,48.464118890169));
#22384=CARTESIAN_POINT('Ctrl Pts',(2.89314538143878,-5.99214762358687,48.4595881764264));
#22385=CARTESIAN_POINT('Ctrl Pts',(2.95442665208855,-6.00381665756757,48.4591554550777));
#22386=CARTESIAN_POINT('Ctrl Pts',(3.05143599671236,-6.01569196513297,48.4585450694277));
#22387=CARTESIAN_POINT('Ctrl Pts',(3.28969174328989,-6.04033961885394,48.4565445600394));
#22388=CARTESIAN_POINT('Ctrl Pts',(3.43093652567676,-6.0531346611766,48.455157285322));
#22389=CARTESIAN_POINT('Ctrl Pts',(3.88020206841996,-6.09364276617912,48.4510874243783));
#22390=CARTESIAN_POINT('Ctrl Pts',(4.15587729830959,-6.11446024451104,48.4470450295077));
#22391=CARTESIAN_POINT('Ctrl Pts',(4.2986604235491,-6.12223844465217,48.4422855877233));
#22392=CARTESIAN_POINT('Ctrl Pts',(3.59439815429413,-5.99475664078893,48.4163876002896));
#22393=CARTESIAN_POINT('Ctrl Pts',(3.631373897052,-6.00697011627484,48.4176356671024));
#22394=CARTESIAN_POINT('Ctrl Pts',(3.69355131163527,-6.02014444454774,48.4189800887165));
#22395=CARTESIAN_POINT('Ctrl Pts',(3.838713446485,-6.04594588203951,48.4216081073813));
#22396=CARTESIAN_POINT('Ctrl Pts',(3.92169816675145,-6.05857299125839,48.422891704432));
#22397=CARTESIAN_POINT('Ctrl Pts',(4.15746922912413,-6.0919301033921,48.4262709574895));
#22398=CARTESIAN_POINT('Ctrl Pts',(4.29707247280368,-6.10813589078398,48.4278950754018));
#22399=CARTESIAN_POINT('Ctrl Pts',(4.30071410004382,-6.10843369230011,48.4278763391901));
#22400=CARTESIAN_POINT('Ctrl Pts',(4.29550794738001,-6.007051447105,48.3603316468569));
#22401=CARTESIAN_POINT('Ctrl Pts',(4.29556063460001,-6.01900581052064,48.3652975204339));
#22402=CARTESIAN_POINT('Ctrl Pts',(4.29569371583991,-6.03128117156189,48.3719827330256));
#22403=CARTESIAN_POINT('Ctrl Pts',(4.29625434599585,-6.05467770199134,48.3864516772668));
#22404=CARTESIAN_POINT('Ctrl Pts',(4.29668189491191,-6.06579887137954,48.3942354089164));
#22405=CARTESIAN_POINT('Ctrl Pts',(4.29860676262888,-6.09473681170808,48.4157241439942));
#22406=CARTESIAN_POINT('Ctrl Pts',(4.3007463023986,-6.10812801481236,48.4275666875517));
#22407=CARTESIAN_POINT('Ctrl Pts',(4.30427685533891,-6.1084337131847,48.4275653153946));
#22408=CARTESIAN_POINT('Ctrl Pts',(4.29550794738001,-6.00705144710501,48.360331646857));
#22409=CARTESIAN_POINT('Ctrl Pts',(4.29571869526291,-6.05486867452994,48.3801950471849));
#22410=CARTESIAN_POINT('Ctrl Pts',(4.29721573529237,-6.10782181536582,48.4275676114412));
#22411=CARTESIAN_POINT('Ctrl Pts',(4.30427675511517,-6.10843370450313,48.4275653154304));
#22412=CARTESIAN_POINT('',(4.29256570756032,-6.20946977623549,48.4959172211618));
#22413=CARTESIAN_POINT('Ctrl Pts',(4.30427669622714,-6.10843371319295,48.4275653292943));
#22414=CARTESIAN_POINT('Ctrl Pts',(4.30071403889905,-6.10843410331512,48.4278767682018));
#22415=CARTESIAN_POINT('Ctrl Pts',(4.29866039809464,-6.12223873054906,48.4422858044068));
#22416=CARTESIAN_POINT('Ctrl Pts',(4.29524066002814,-6.16064820739695,48.4713966576509));
#22417=CARTESIAN_POINT('Ctrl Pts',(4.29388241016422,-6.18548926373562,48.4859212758134));
#22418=CARTESIAN_POINT('Ctrl Pts',(4.29256571553473,-6.20946968450872,48.4959174422579));
#22419=CARTESIAN_POINT('Ctrl Pts',(4.29256571553473,-6.20946968450872,48.4959174422579));
#22420=CARTESIAN_POINT('Ctrl Pts',(3.59085026662451,-6.17306838545285,48.5061181031007));
#22421=CARTESIAN_POINT('Ctrl Pts',(2.88857791145589,-6.13245845075531,48.5108119660871));
#22422=CARTESIAN_POINT('Ctrl Pts',(1.48700388381999,-6.04366518478247,48.5141172996865));
#22423=CARTESIAN_POINT('Ctrl Pts',(0.785617178130183,-6.01733942146269,
48.5199462997133));
#22424=CARTESIAN_POINT('Ctrl Pts',(0.0835265683815503,-6.00666333723547,
48.5199460669664));
#22425=CARTESIAN_POINT('Ctrl Pts',(0.0835265683815503,-6.00666333723547,
48.5199460669664));
#22426=CARTESIAN_POINT('Ctrl Pts',(0.083526568382076,-6.02801550569024,
48.5199465324602));
#22427=CARTESIAN_POINT('Ctrl Pts',(0.0835265683917245,-6.05386667280684,
48.5195892904706));
#22428=CARTESIAN_POINT('Ctrl Pts',(0.0835265683750737,-6.10694539169996,
48.521354690718));
#22429=CARTESIAN_POINT('Ctrl Pts',(0.0835265683690384,-6.12148849588211,
48.5199317919394));
#22430=CARTESIAN_POINT('Ctrl Pts',(0.0835265683620147,-6.14692278878554,
48.5199317919394));
#22431=CARTESIAN_POINT('Ctrl Pts',(0.434571873255867,-6.01200137934908,
48.5199461833399));
#22432=CARTESIAN_POINT('Ctrl Pts',(0.356369924026296,-6.03090918789886,
48.5198869612841));
#22433=CARTESIAN_POINT('Ctrl Pts',(0.356156584407958,-6.05382055712373,
48.519586959623));
#22434=CARTESIAN_POINT('Ctrl Pts',(0.394869806313788,-6.10695822375808,
48.5213559145512));
#22435=CARTESIAN_POINT('Ctrl Pts',(0.433796367857451,-6.12148849588211,
48.5199317919394));
#22436=CARTESIAN_POINT('Ctrl Pts',(0.433874220973527,-6.14692278878554,
48.5199317919394));
#22437=CARTESIAN_POINT('Ctrl Pts',(0.785441202115477,-6.02125184123583,
48.5184889915199));
#22438=CARTESIAN_POINT('Ctrl Pts',(0.651973538428245,-6.03698783585496,
48.5195752075049));
#22439=CARTESIAN_POINT('Ctrl Pts',(0.651610339577195,-6.05830967273444,
48.5196902430867));
#22440=CARTESIAN_POINT('Ctrl Pts',(0.717676140419002,-6.11145963930962,
48.5214911612938));
#22441=CARTESIAN_POINT('Ctrl Pts',(0.784105140129702,-6.12687873284897,
48.5199317919388));
#22442=CARTESIAN_POINT('Ctrl Pts',(0.784221873585039,-6.15072449281721,
48.5199317919388));
#22443=CARTESIAN_POINT('Ctrl Pts',(1.48685396085203,-6.04818290219913,48.5151613829932));
#22444=CARTESIAN_POINT('Ctrl Pts',(1.29453399477866,-6.05935112779906,48.5183112784905));
#22445=CARTESIAN_POINT('Ctrl Pts',(1.29397444382209,-6.07865710025977,48.5193460059679));
#22446=CARTESIAN_POINT('Ctrl Pts',(1.3890700537892,-6.12977840933564,48.5214366576208));
#22447=CARTESIAN_POINT('Ctrl Pts',(1.48472521472664,-6.14643370208422,48.5199317919371));
#22448=CARTESIAN_POINT('Ctrl Pts',(1.48483467245509,-6.16593130894387,48.5199317919372));
#22449=CARTESIAN_POINT('Ctrl Pts',(1.83739739072896,-6.06586350127568,48.5132909662866));
#22450=CARTESIAN_POINT('Ctrl Pts',(1.64148768190344,-6.07568031733619,48.5173741424648));
#22451=CARTESIAN_POINT('Ctrl Pts',(1.64088163807406,-6.09455995772352,48.518913524595));
#22452=CARTESIAN_POINT('Ctrl Pts',(1.73765605564234,-6.14361803658467,48.5212544268102));
#22453=CARTESIAN_POINT('Ctrl Pts',(1.83503651705134,-6.16059843435261,48.5199317919361));
#22454=CARTESIAN_POINT('Ctrl Pts',(1.83509981871363,-6.17733642103887,48.5199317919363));
#22455=CARTESIAN_POINT('Ctrl Pts',(2.88857791145589,-6.13245845075531,48.5108119660871));
#22456=CARTESIAN_POINT('Ctrl Pts',(2.76813631530143,-6.14582978514633,48.5172046544333));
#22457=CARTESIAN_POINT('Ctrl Pts',(2.7675104507475,-6.16286923349053,48.5194534620087));
#22458=CARTESIAN_POINT('Ctrl Pts',(2.82637284101024,-6.19966838879308,48.5212339924787));
#22459=CARTESIAN_POINT('Ctrl Pts',(2.88586109583122,-6.21324540616175,48.5199317919341));
#22460=CARTESIAN_POINT('Ctrl Pts',(2.88564773843035,-6.22295686941886,48.5199317919344));
#22461=CARTESIAN_POINT('Ctrl Pts',(3.59085026662451,-6.17306838545285,48.5061181031007));
#22462=CARTESIAN_POINT('Ctrl Pts',(3.5189080182867,-6.1918452082941,48.5141149281106));
#22463=CARTESIAN_POINT('Ctrl Pts',(3.51790722546928,-6.21237399283442,48.5175683503188));
#22464=CARTESIAN_POINT('Ctrl Pts',(3.55158573837203,-6.24739159904062,48.5204767822306));
#22465=CARTESIAN_POINT('Ctrl Pts',(3.58626504409221,-6.2618804207065,48.5199317919341));
#22466=CARTESIAN_POINT('Ctrl Pts',(3.58568299282961,-6.26857731779886,48.5199317919344));
#22467=CARTESIAN_POINT('Ctrl Pts',(4.29256571553473,-6.20946968450873,48.4959174422579));
#22468=CARTESIAN_POINT('Ctrl Pts',(4.29124902090524,-6.23345010528185,48.5059136087023));
#22469=CARTESIAN_POINT('Ctrl Pts',(4.28995382260361,-6.25674581560883,48.5119171961227));
#22470=CARTESIAN_POINT('Ctrl Pts',(4.28744009183432,-6.29803503999845,48.5189262877413));
#22471=CARTESIAN_POINT('Ctrl Pts',(4.28622155936666,-6.31602855406109,48.5199317919394));
#22472=CARTESIAN_POINT('Ctrl Pts',(4.2850581964051,-6.32940458230552,48.5199317919394));
#22473=CARTESIAN_POINT('Ctrl Pts',(4.2925656916115,-6.20946995968903,48.4959167789697));
#22474=CARTESIAN_POINT('Ctrl Pts',(4.29202349410917,-6.21934480701988,48.5000331414517));
#22475=CARTESIAN_POINT('Ctrl Pts',(4.2914804459715,-6.2291557048318,48.503523063216));
#22476=CARTESIAN_POINT('Ctrl Pts',(4.29094213463875,-6.23871408127371,48.5064309619194));
#22477=CARTESIAN_POINT('Ctrl Pts',(4.29037097470351,-6.24885572484954,48.5095163051661));
#22478=CARTESIAN_POINT('Ctrl Pts',(4.28980525582109,-6.25871184341276,48.5119471308067));
#22479=CARTESIAN_POINT('Ctrl Pts',(4.28924924924487,-6.26808527594654,48.5138297415884));
#22480=CARTESIAN_POINT('Ctrl Pts',(4.28866783601525,-6.27788702634898,48.5157983780426));
#22481=CARTESIAN_POINT('Ctrl Pts',(4.2880971014353,-6.28716030960548,48.5171691011132));
#22482=CARTESIAN_POINT('Ctrl Pts',(4.28753800272483,-6.2957252017121,48.5181018578833));
#22483=CARTESIAN_POINT('Ctrl Pts',(4.28693020589066,-6.30503610551124,48.5191158588125));
#22484=CARTESIAN_POINT('Ctrl Pts',(4.28633616809252,-6.31350977078174,48.5196144990409));
#22485=CARTESIAN_POINT('Ctrl Pts',(4.28575192091124,-6.32097498479555,48.5198172708104));
#22486=CARTESIAN_POINT('Ctrl Pts',(4.28551932677286,-6.323946954669,48.5198979961036));
#22487=CARTESIAN_POINT('Ctrl Pts',(4.28528823042114,-6.32675971428291,48.5199317800711));
#22488=CARTESIAN_POINT('Ctrl Pts',(4.2850581964051,-6.32940458230551,48.5199317919363));
#22489=CARTESIAN_POINT('Ctrl Pts',(0.0835265683620147,-6.14692278878557,
48.5199317919394));
#22490=CARTESIAN_POINT('Ctrl Pts',(0.0835265683690384,-6.12148849588211,
48.5199317919394));
#22491=CARTESIAN_POINT('Ctrl Pts',(0.0835265683750737,-6.10694539169996,
48.521354690718));
#22492=CARTESIAN_POINT('Ctrl Pts',(0.0835265683917245,-6.05386667280684,
48.5195892904706));
#22493=CARTESIAN_POINT('Ctrl Pts',(0.083526568382076,-6.02801550569024,
48.5199465324602));
#22494=CARTESIAN_POINT('Ctrl Pts',(0.0835265683815503,-6.00666333723547,
48.5199460669664));
#22495=CARTESIAN_POINT('Ctrl Pts',(0.0835265683815503,-6.00666333723547,
48.5199460669664));
#22496=CARTESIAN_POINT('Ctrl Pts',(-0.267518736492503,-6.01200137934925,
48.5199461833398));
#22497=CARTESIAN_POINT('Ctrl Pts',(-0.618388065344823,-6.02125184123478,
48.5184889915195));
#22498=CARTESIAN_POINT('Ctrl Pts',(-1.31980082405271,-6.04818290219398,
48.5151613829919));
#22499=CARTESIAN_POINT('Ctrl Pts',(-1.67034425390828,-6.06586350126765,
48.5132909662846));
#22500=CARTESIAN_POINT('Ctrl Pts',(-2.72152477454993,-6.13245845073777,
48.5108119660831));
#22501=CARTESIAN_POINT('Ctrl Pts',(-3.42379712957049,-6.17306838542386,
48.5061181030979));
#22502=CARTESIAN_POINT('Ctrl Pts',(-4.12551257835428,-6.20946968446904,
48.4959174422579));
#22503=CARTESIAN_POINT('Ctrl Pts',(0.083526568382076,-6.02801550569024,
48.5199465324602));
#22504=CARTESIAN_POINT('Ctrl Pts',(-0.189316787260607,-6.03090918789797,
48.5198869612836));
#22505=CARTESIAN_POINT('Ctrl Pts',(-0.484920401653545,-6.03698783585283,
48.5195752075044));
#22506=CARTESIAN_POINT('Ctrl Pts',(-1.12748085797788,-6.05935112779399,
48.51831127849));
#22507=CARTESIAN_POINT('Ctrl Pts',(-1.47443454508558,-6.07568031732946,
48.5173741424643));
#22508=CARTESIAN_POINT('Ctrl Pts',(-2.60108317843058,-6.14582978513443,
48.5172046544322));
#22509=CARTESIAN_POINT('Ctrl Pts',(-3.35185488132463,-6.19184520827618,
48.5141149281108));
#22510=CARTESIAN_POINT('Ctrl Pts',(-4.12419588396466,-6.23345010526292,
48.5059136087023));
#22511=CARTESIAN_POINT('Ctrl Pts',(0.0835265683917245,-6.05386667280684,
48.5195892904706));
#22512=CARTESIAN_POINT('Ctrl Pts',(-0.189103447624509,-6.0538205571228,
48.5195869596226));
#22513=CARTESIAN_POINT('Ctrl Pts',(-0.484557202789109,-6.05830967273256,
48.5196902430863));
#22514=CARTESIAN_POINT('Ctrl Pts',(-1.12692130702108,-6.07865710025598,
48.5193460059677));
#22515=CARTESIAN_POINT('Ctrl Pts',(-1.47382850126476,-6.09455995771879,
48.518913524595));
#22516=CARTESIAN_POINT('Ctrl Pts',(-2.60045731391633,-6.16286923348301,
48.5194534620086));
#22517=CARTESIAN_POINT('Ctrl Pts',(-3.35085408858969,-6.21237399282374,
48.5175683503199));
#22518=CARTESIAN_POINT('Ctrl Pts',(-4.12290068577714,-6.25674581559982,
48.5119171961227));
#22519=CARTESIAN_POINT('Ctrl Pts',(0.0835265683750737,-6.10694539169996,
48.521354690718));
#22520=CARTESIAN_POINT('Ctrl Pts',(-0.227816669563641,-6.1069582237576,
48.521355914551));
#22521=CARTESIAN_POINT('Ctrl Pts',(-0.550623003667509,-6.11145963930881,
48.5214911612936));
#22522=CARTESIAN_POINT('Ctrl Pts',(-1.22201691703506,-6.12977840933438,
48.5214366576209));
#22523=CARTESIAN_POINT('Ctrl Pts',(-1.57060291888689,-6.14361803658331,
48.5212544268105));
#22524=CARTESIAN_POINT('Ctrl Pts',(-2.65931970425501,-6.1996683887915,48.5212339924792));
#22525=CARTESIAN_POINT('Ctrl Pts',(-3.38453260161145,-6.24739159903889,
48.5204767822314));
#22526=CARTESIAN_POINT('Ctrl Pts',(-4.12038695511613,-6.29803503999888,
48.5189262877413));
#22527=CARTESIAN_POINT('Ctrl Pts',(0.0835265683690384,-6.12148849588211,
48.5199317919394));
#22528=CARTESIAN_POINT('Ctrl Pts',(-0.266743231119374,-6.12148849588211,
48.5199317919394));
#22529=CARTESIAN_POINT('Ctrl Pts',(-0.6170520033925,-6.12687873284897,48.5199317919388));
#22530=CARTESIAN_POINT('Ctrl Pts',(-1.31767207799207,-6.14643370208422,
48.5199317919371));
#22531=CARTESIAN_POINT('Ctrl Pts',(-1.66798338031851,-6.1605984343526,48.5199317919361));
#22532=CARTESIAN_POINT('Ctrl Pts',(-2.71880795910365,-6.21324540616174,
48.5199317919341));
#22533=CARTESIAN_POINT('Ctrl Pts',(-3.41921190736816,-6.26188042070648,
48.5199317919341));
#22534=CARTESIAN_POINT('Ctrl Pts',(-4.11916842264263,-6.31602855406106,
48.5199317919394));
#22535=CARTESIAN_POINT('Ctrl Pts',(0.0835265683620147,-6.14692278878554,
48.5199317919394));
#22536=CARTESIAN_POINT('Ctrl Pts',(-0.266821084249497,-6.14692278878554,
48.5199317919394));
#22537=CARTESIAN_POINT('Ctrl Pts',(-0.617168736861009,-6.15072449281721,
48.5199317919388));
#22538=CARTESIAN_POINT('Ctrl Pts',(-1.31778153573106,-6.16593130894387,
48.5199317919372));
#22539=CARTESIAN_POINT('Ctrl Pts',(-1.6680466819896,-6.17733642103887,48.5199317919363));
#22540=CARTESIAN_POINT('Ctrl Pts',(-2.71859460170632,-6.22295686941886,
48.5199317919344));
#22541=CARTESIAN_POINT('Ctrl Pts',(-3.41862985610558,-6.26857731779886,
48.5199317919344));
#22542=CARTESIAN_POINT('Ctrl Pts',(-4.11800505968107,-6.32940458230553,
48.5199317919394));
#22543=CARTESIAN_POINT('',(-4.12551257076669,-6.20946977174738,48.495917231884));
#22544=CARTESIAN_POINT('Ctrl Pts',(-4.11800505968107,-6.32940458230551,
48.5199317919367));
#22545=CARTESIAN_POINT('Ctrl Pts',(-4.11858674116184,-6.32271656818346,
48.5199317638787));
#22546=CARTESIAN_POINT('Ctrl Pts',(-4.11917549964439,-6.31495176722324,
48.5197172285933));
#22547=CARTESIAN_POINT('Ctrl Pts',(-4.11977717145446,-6.30626433210882,
48.5190688039378));
#22548=CARTESIAN_POINT('Ctrl Pts',(-4.12032674885696,-6.29832907912767,
48.5184765216804));
#22549=CARTESIAN_POINT('Ctrl Pts',(-4.12088712278166,-6.28962376481006,
48.517520333247));
#22550=CARTESIAN_POINT('Ctrl Pts',(-4.12145907343358,-6.28030805427432,
48.5160324259247));
#22551=CARTESIAN_POINT('Ctrl Pts',(-4.12200326888234,-6.27144440972983,
48.5146167226812));
#22552=CARTESIAN_POINT('Ctrl Pts',(-4.12255791867854,-6.26202846118951,
48.5127182234746));
#22553=CARTESIAN_POINT('Ctrl Pts',(-4.12312024912556,-6.25223759022031,
48.5102148793545));
#22554=CARTESIAN_POINT('Ctrl Pts',(-4.12365584850649,-6.24291214028643,
48.5078305347612));
#22555=CARTESIAN_POINT('Ctrl Pts',(-4.12419834333242,-6.23324739180506,
48.5048965752648));
#22556=CARTESIAN_POINT('Ctrl Pts',(-4.12474286125808,-6.22342541541294,
48.5013450104422));
#22557=CARTESIAN_POINT('Ctrl Pts',(-4.12499921694512,-6.21880128939725,
48.4996729555891));
#22558=CARTESIAN_POINT('Ctrl Pts',(-4.12525599093568,-6.214142666,48.4978646482433));
#22559=CARTESIAN_POINT('Ctrl Pts',(-4.12551255559153,-6.20946994630408,
48.4959168111364));
#22560=CARTESIAN_POINT('Ctrl Pts',(-4.12551257835429,-6.20946968446903,
48.4959174422579));
#22561=CARTESIAN_POINT('Ctrl Pts',(-3.42379712957049,-6.17306838542386,
48.5061181030979));
#22562=CARTESIAN_POINT('Ctrl Pts',(-2.72152477454993,-6.13245845073777,
48.5108119660831));
#22563=CARTESIAN_POINT('Ctrl Pts',(-1.31995074702773,-6.04366518477761,
48.514117299685));
#22564=CARTESIAN_POINT('Ctrl Pts',(-0.618564041366555,-6.01733942146302,
48.5199462997132));
#22565=CARTESIAN_POINT('Ctrl Pts',(0.0835265683815503,-6.00666333723547,
48.5199460669664));
#22566=CARTESIAN_POINT('Ctrl Pts',(0.0835265683815503,-6.00666333723547,
48.5199460669664));
#22567=CARTESIAN_POINT('Ctrl Pts',(-0.267518736492766,-6.00132529512186,
48.519945950593));
#22568=CARTESIAN_POINT('Ctrl Pts',(-0.61861597912618,-5.99973567328081,
48.5184885224508));
#22569=CARTESIAN_POINT('Ctrl Pts',(-1.32094154226152,-5.99820579736984,
48.5087577021076));
#22570=CARTESIAN_POINT('Ctrl Pts',(-1.67216986276346,-5.99826554329992,
48.5004843099067));
#22571=CARTESIAN_POINT('Ctrl Pts',(-2.7260922445975,-5.99214762358588,48.4595881764337));
#22572=CARTESIAN_POINT('Ctrl Pts',(-3.42734501754431,-5.9947566407883,48.4163876002916));
#22573=CARTESIAN_POINT('Ctrl Pts',(-4.128454810656,-6.007051447105,48.3603316468569));
#22574=CARTESIAN_POINT('Ctrl Pts',(-0.267518736492503,-6.01200137934925,
48.5199461833399));
#22575=CARTESIAN_POINT('Ctrl Pts',(-0.54053515644952,-6.00879525432305,
48.519004334916));
#22576=CARTESIAN_POINT('Ctrl Pts',(-0.831623018753302,-6.00835114797875,
48.5169166777066));
#22577=CARTESIAN_POINT('Ctrl Pts',(-1.44672510888142,-6.00829173506044,
48.5070409830143));
#22578=CARTESIAN_POINT('Ctrl Pts',(-1.77074437164332,-6.00864450579794,
48.4992338112145));
#22579=CARTESIAN_POINT('Ctrl Pts',(-2.7873735152434,-6.00381665756613,48.4591554550849));
#22580=CARTESIAN_POINT('Ctrl Pts',(-3.46432076030098,-6.006970116274,48.4176356671043));
#22581=CARTESIAN_POINT('Ctrl Pts',(-4.12850749787601,-6.01900581052063,
48.3652975204339));
#22582=CARTESIAN_POINT('Ctrl Pts',(-0.618388065344823,-6.02125184123478,
48.5184889915195));
#22583=CARTESIAN_POINT('Ctrl Pts',(-0.831277824717596,-6.01828947675541,
48.5172889554692));
#22584=CARTESIAN_POINT('Ctrl Pts',(-1.07630838450787,-6.01789996842512,
48.5149008816201));
#22585=CARTESIAN_POINT('Ctrl Pts',(-1.62065368277726,-6.01814206511781,
48.5050013605236));
#22586=CARTESIAN_POINT('Ctrl Pts',(-1.91997597366274,-6.01872578610802,
48.4974612118007));
#22587=CARTESIAN_POINT('Ctrl Pts',(-2.88438285982273,-6.015691965127,48.4585450694341));
#22588=CARTESIAN_POINT('Ctrl Pts',(-3.52649817488522,-6.02014444454682,
48.4189800887184));
#22589=CARTESIAN_POINT('Ctrl Pts',(-4.12864057911591,-6.03128117156189,
48.3719827330256));
#22590=CARTESIAN_POINT('Ctrl Pts',(-1.31980082405271,-6.04818290219398,
48.5151613829919));
#22591=CARTESIAN_POINT('Ctrl Pts',(-1.44516286435873,-6.04432658406756,
48.5134046445656));
#22592=CARTESIAN_POINT('Ctrl Pts',(-1.61934713476681,-6.04289085428145,
48.5103147763951));
#22593=CARTESIAN_POINT('Ctrl Pts',(-2.04329097920305,-6.0417352100729,48.4999506928749));
#22594=CARTESIAN_POINT('Ctrl Pts',(-2.29305999373915,-6.0419554406095,48.4926406006807));
#22595=CARTESIAN_POINT('Ctrl Pts',(-3.12263860626336,-6.04033961883415,
48.4565445600434));
#22596=CARTESIAN_POINT('Ctrl Pts',(-3.67166030973921,-6.04594588203862,
48.4216081073828));
#22597=CARTESIAN_POINT('Ctrl Pts',(-4.12920120927185,-6.05467770199134,
48.3864516772669));
#22598=CARTESIAN_POINT('Ctrl Pts',(-1.67034425390828,-6.06586350126765,
48.5132909662846));
#22599=CARTESIAN_POINT('Ctrl Pts',(-1.76830361616495,-6.06089216511445,
48.51123856213));
#22600=CARTESIAN_POINT('Ctrl Pts',(-1.91769808992094,-6.05836696394206,
48.5077487407884));
#22601=CARTESIAN_POINT('Ctrl Pts',(-2.29199666504518,-6.05552058028394,
48.4969449896315));
#22602=CARTESIAN_POINT('Ctrl Pts',(-2.51690957755418,-6.05514353309333,
48.4895975747613));
#22603=CARTESIAN_POINT('Ctrl Pts',(-3.2638833885578,-6.05313466114755,48.4551572853244));
#22604=CARTESIAN_POINT('Ctrl Pts',(-3.75464503000896,-6.0585729912576,48.4228917044332));
#22605=CARTESIAN_POINT('Ctrl Pts',(-4.1296287581879,-6.06579887137954,48.3942354089164));
#22606=CARTESIAN_POINT('Ctrl Pts',(-2.72152477454993,-6.13245845073777,
48.5108119660831));
#22607=CARTESIAN_POINT('Ctrl Pts',(-2.78175048147961,-6.12571278892217,
48.507599134673));
#22608=CARTESIAN_POINT('Ctrl Pts',(-2.87872640152294,-6.1197510150967,48.5025662256946));
#22609=CARTESIAN_POINT('Ctrl Pts',(-3.11802710698666,-6.10935599899705,
48.4895414181605));
#22610=CARTESIAN_POINT('Ctrl Pts',(-3.26035692734462,-6.10489083403437,
48.4815303852878));
#22611=CARTESIAN_POINT('Ctrl Pts',(-3.71314893100167,-6.09364276612037,
48.4510874243765));
#22612=CARTESIAN_POINT('Ctrl Pts',(-3.99041609239207,-6.09193010339169,
48.4262709574899));
#22613=CARTESIAN_POINT('Ctrl Pts',(-4.13155362590487,-6.09473681170807,
48.4157241439942));
#22614=CARTESIAN_POINT('Ctrl Pts',(-3.42379712957049,-6.17306838542386,
48.5061181030979));
#22615=CARTESIAN_POINT('Ctrl Pts',(-3.45976825369342,-6.1636799739977,48.5021196905914));
#22616=CARTESIAN_POINT('Ctrl Pts',(-3.52173694617229,-6.15479195321228,
48.4962278198627));
#22617=CARTESIAN_POINT('Ctrl Pts',(-3.66733280171424,-6.13882811012295,
48.4820050858237));
#22618=CARTESIAN_POINT('Ctrl Pts',(-3.75095996477732,-6.13175228781906,
48.4736742225135));
#22619=CARTESIAN_POINT('Ctrl Pts',(-3.98882416065135,-6.11446024442977,
48.4470450295045));
#22620=CARTESIAN_POINT('Ctrl Pts',(-4.13001933607927,-6.10813589078394,
48.4278950754018));
#22621=CARTESIAN_POINT('Ctrl Pts',(-4.13369316567458,-6.10812801481237,
48.4275666875517));
#22622=CARTESIAN_POINT('Ctrl Pts',(-4.12551257835428,-6.20946968446904,
48.4959174422579));
#22623=CARTESIAN_POINT('Ctrl Pts',(-4.12617092554909,-6.1974794740721,48.4909193590357));
#22624=CARTESIAN_POINT('Ctrl Pts',(-4.12683966151712,-6.18527410478074,
48.484789162884));
#22625=CARTESIAN_POINT('Ctrl Pts',(-4.12827543030072,-6.16205725105381,
48.4713889284507));
#22626=CARTESIAN_POINT('Ctrl Pts',(-4.12904246311627,-6.15104576661825,
48.4641188901692));
#22627=CARTESIAN_POINT('Ctrl Pts',(-4.13160728578581,-6.12223844456225,
48.4422855877235));
#22628=CARTESIAN_POINT('Ctrl Pts',(-4.13366096331981,-6.10843369230011,
48.4278763391901));
#22629=CARTESIAN_POINT('Ctrl Pts',(-4.13722371861489,-6.1084337131847,48.4275653153946));
#22630=CARTESIAN_POINT('Ctrl Pts',(-4.12551257835429,-6.20946968446903,
48.4959174422579));
#22631=CARTESIAN_POINT('Ctrl Pts',(-4.12682927274388,-6.18548926367518,
48.4859212758135));
#22632=CARTESIAN_POINT('Ctrl Pts',(-4.12818752222643,-6.16064820730358,
48.4713966576511));
#22633=CARTESIAN_POINT('Ctrl Pts',(-4.13160728578581,-6.12223844456225,
48.4422855877235));
#22634=CARTESIAN_POINT('Ctrl Pts',(-4.13366096331981,-6.10843369230011,
48.4278763391901));
#22635=CARTESIAN_POINT('Ctrl Pts',(-4.13722371861488,-6.10843371318471,
48.4275653153946));
#22636=CARTESIAN_POINT('',(-4.128454810656,-6.00705144710501,48.3603316468569));
#22637=CARTESIAN_POINT('Ctrl Pts',(-4.128454810656,-6.00705144710501,48.3603316468569));
#22638=CARTESIAN_POINT('Ctrl Pts',(-4.12847724605468,-6.01214188287171,
48.3624462270809));
#22639=CARTESIAN_POINT('Ctrl Pts',(-4.12851349521485,-6.01712839937856,
48.3648008414081));
#22640=CARTESIAN_POINT('Ctrl Pts',(-4.12856659590172,-6.02202475059606,
48.3673129480271));
#22641=CARTESIAN_POINT('Ctrl Pts',(-4.12863240824478,-6.0280932285195,48.3704264223024));
#22642=CARTESIAN_POINT('Ctrl Pts',(-4.12872385551699,-6.03402509336409,
48.3737833452877));
#22643=CARTESIAN_POINT('Ctrl Pts',(-4.12884968366995,-6.03985134815184,
48.3773045718558));
#22644=CARTESIAN_POINT('Ctrl Pts',(-4.12887227551138,-6.04089742425802,
48.3779367911994));
#22645=CARTESIAN_POINT('Ctrl Pts',(-4.12889598882607,-6.04194007207302,
48.3785744384767));
#22646=CARTESIAN_POINT('Ctrl Pts',(-4.12892089419388,-6.04297943677661,
48.3792172051462));
#22647=CARTESIAN_POINT('Ctrl Pts',(-4.12907740642859,-6.04951109266998,
48.3832565290626));
#22648=CARTESIAN_POINT('Ctrl Pts',(-4.12927928721199,-6.05591440502064,
48.3874952504182));
#22649=CARTESIAN_POINT('Ctrl Pts',(-4.12955440546488,-6.06221540874182,
48.3918795150871));
#22650=CARTESIAN_POINT('Ctrl Pts',(-4.129749144932,-6.06667550578774,48.3949828692134));
#22651=CARTESIAN_POINT('Ctrl Pts',(-4.12998024811885,-6.07108307587747,
48.3981593533735));
#22652=CARTESIAN_POINT('Ctrl Pts',(-4.13027038076022,-6.07544485148905,
48.401398320609));
#22653=CARTESIAN_POINT('Ctrl Pts',(-4.13051585714226,-6.07913527698313,
48.4041387566893));
#22654=CARTESIAN_POINT('Ctrl Pts',(-4.13080237637701,-6.08279191115652,
48.406923377578));
#22655=CARTESIAN_POINT('Ctrl Pts',(-4.1311632911292,-6.08641490063092,48.409745887031));
#22656=CARTESIAN_POINT('Ctrl Pts',(-4.13142089737007,-6.08900084286116,
48.4117604792459));
#22657=CARTESIAN_POINT('Ctrl Pts',(-4.13171554465927,-6.09157063046096,
48.4137952446382));
#22658=CARTESIAN_POINT('Ctrl Pts',(-4.13208086203652,-6.09412272337342,
48.4158470897808));
#22659=CARTESIAN_POINT('Ctrl Pts',(-4.13233561746212,-6.09590243481497,
48.4172779515879));
#22660=CARTESIAN_POINT('Ctrl Pts',(-4.1326236272006,-6.09767362900813,48.4187172631575));
#22661=CARTESIAN_POINT('Ctrl Pts',(-4.13297918313311,-6.09943558046489,
48.4201632417151));
#22662=CARTESIAN_POINT('Ctrl Pts',(-4.1332181244978,-6.10061965038779,48.4211349709376));
#22663=CARTESIAN_POINT('Ctrl Pts',(-4.13348648933834,-6.10179994098431,
48.4221101275599));
#22664=CARTESIAN_POINT('Ctrl Pts',(-4.13381763546866,-6.1029736298463,48.4230849222562));
#22665=CARTESIAN_POINT('Ctrl Pts',(-4.13401726738067,-6.10368118983316,
48.4236725786145));
#22666=CARTESIAN_POINT('Ctrl Pts',(-4.13423928223204,-6.10438688630814,
48.4242605993929));
#22667=CARTESIAN_POINT('Ctrl Pts',(-4.13450789108345,-6.10508829918447,
48.4248456081052));
#22668=CARTESIAN_POINT('Ctrl Pts',(-4.13468189352899,-6.10554266826118,
48.4252245715908));
#22669=CARTESIAN_POINT('Ctrl Pts',(-4.13487545529636,-6.10599659049777,
48.4256034524709));
#22670=CARTESIAN_POINT('Ctrl Pts',(-4.1351077826707,-6.10644310670885,48.425975005762));
#22671=CARTESIAN_POINT('Ctrl Pts',(-4.13523410076814,-6.10668588084782,
48.4261770220115));
#22672=CARTESIAN_POINT('Ctrl Pts',(-4.13537284994624,-6.10692799624868,
48.4263781398347));
#22673=CARTESIAN_POINT('Ctrl Pts',(-4.13553088498902,-6.10716341124115,
48.4265725981583));
#22674=CARTESIAN_POINT('Ctrl Pts',(-4.13565915175361,-6.10735448227761,
48.4267304273306));
#22675=CARTESIAN_POINT('Ctrl Pts',(-4.13579977890918,-6.10754133617494,
48.4268840707421));
#22676=CARTESIAN_POINT('Ctrl Pts',(-4.13596274135563,-6.10771844494464,
48.4270278886976));
#22677=CARTESIAN_POINT('Ctrl Pts',(-4.13604422257886,-6.10780699932949,
48.4270997976754));
#22678=CARTESIAN_POINT('Ctrl Pts',(-4.13612859947745,-6.10789132123182,
48.4271678595123));
#22679=CARTESIAN_POINT('Ctrl Pts',(-4.1362343104114,-6.10798127288396,48.4272394029535));
#22680=CARTESIAN_POINT('Ctrl Pts',(-4.13628716587837,-6.10802624871004,
48.4272751746741));
#22681=CARTESIAN_POINT('Ctrl Pts',(-4.13634156485444,-6.10807104932053,
48.4273106966924));
#22682=CARTESIAN_POINT('Ctrl Pts',(-4.13643190669548,-6.10813310869716,
48.4273588375411));
#22683=CARTESIAN_POINT('Ctrl Pts',(-4.13647707759982,-6.10816413837435,
48.4273829079569));
#22684=CARTESIAN_POINT('Ctrl Pts',(-4.13654110267543,-6.10820885152138,
48.4274176883991));
#22685=CARTESIAN_POINT('Ctrl Pts',(-4.13665996059634,-6.10826888896282,
48.427461956441));
#22686=CARTESIAN_POINT('Ctrl Pts',(-4.13674745395857,-6.10831308355725,
48.427494542909));
#22687=CARTESIAN_POINT('Ctrl Pts',(-4.13686461503084,-6.10836602282818,
48.4275326992659));
#22688=CARTESIAN_POINT('Ctrl Pts',(-4.13702847377054,-6.10840319283375,
48.4275531996689));
#22689=CARTESIAN_POINT('Ctrl Pts',(-4.1370872137358,-6.1084165175111,48.4275605486389));
#22690=CARTESIAN_POINT('Ctrl Pts',(-4.13715198788423,-6.10842750223913,
48.4275653432463));
#22691=CARTESIAN_POINT('Ctrl Pts',(-4.13722371803033,-6.10843371313409,
48.4275653153948));
#22692=CARTESIAN_POINT('Ctrl Pts',(-4.128454810656,-6.00705144710501,48.3603316468569));
#22693=CARTESIAN_POINT('Ctrl Pts',(-3.42734501754431,-5.9947566407883,48.4163876002916));
#22694=CARTESIAN_POINT('Ctrl Pts',(-2.7260922445975,-5.99214762358588,48.4595881764337));
#22695=CARTESIAN_POINT('Ctrl Pts',(-1.32086240215211,-6.00030484987126,
48.5141163543976));
#22696=CARTESIAN_POINT('Ctrl Pts',(-0.618564041367084,-5.99598725300824,
48.5199458342196));
#22697=CARTESIAN_POINT('Ctrl Pts',(0.0835265683815503,-6.00666333723547,
48.5199460669664));
#22698=CARTESIAN_POINT('Ctrl Pts',(-48.353987706665,-6.00666333723547,0.0824317919588709));
#22699=CARTESIAN_POINT('Ctrl Pts',(-48.3539881721587,-6.02801550569024,
0.082431791959394));
#22700=CARTESIAN_POINT('Ctrl Pts',(-48.3536309301691,-6.05386667280685,
0.0824317919690549));
#22701=CARTESIAN_POINT('Ctrl Pts',(-48.3553963304166,-6.10694539169998,
0.082431791952385));
#22702=CARTESIAN_POINT('Ctrl Pts',(-48.3539734316379,-6.12148849588211,
0.0824317919463454));
#22703=CARTESIAN_POINT('Ctrl Pts',(-48.3539734316379,-6.14692278878554,
0.0824317919393188));
#22704=CARTESIAN_POINT('Ctrl Pts',(-48.3539878230387,-6.01200137934915,
0.433477096833169));
#22705=CARTESIAN_POINT('Ctrl Pts',(-48.3539286009829,-6.0309091878989,0.355275147603605));
#22706=CARTESIAN_POINT('Ctrl Pts',(-48.3536285993218,-6.05382055712376,
0.355061807985282));
#22707=CARTESIAN_POINT('Ctrl Pts',(-48.3553975542498,-6.10695822375809,
0.393775029891096));
#22708=CARTESIAN_POINT('Ctrl Pts',(-48.3539734316379,-6.12148849588211,
0.432701591434755));
#22709=CARTESIAN_POINT('Ctrl Pts',(-48.3539734316379,-6.14692278878554,
0.432779444550827));
#22710=CARTESIAN_POINT('Ctrl Pts',(-48.3525306312191,-6.02125184123593,
0.784346425692766));
#22711=CARTESIAN_POINT('Ctrl Pts',(-48.353616847204,-6.03698783585502,0.650878762005552));
#22712=CARTESIAN_POINT('Ctrl Pts',(-48.3537318827856,-6.05830967273448,
0.650515563154517));
#22713=CARTESIAN_POINT('Ctrl Pts',(-48.3555328009924,-6.11145963930963,
0.716581363996309));
#22714=CARTESIAN_POINT('Ctrl Pts',(-48.3539734316373,-6.12687873284897,
0.783010363707002));
#22715=CARTESIAN_POINT('Ctrl Pts',(-48.3539734316373,-6.15072449281721,
0.783127097162336));
#22716=CARTESIAN_POINT('Ctrl Pts',(-48.3492030226928,-6.04818290219923,
1.48575918442931));
#22717=CARTESIAN_POINT('Ctrl Pts',(-48.3523529181898,-6.05935112779917,
1.29343921835598));
#22718=CARTESIAN_POINT('Ctrl Pts',(-48.353387645667,-6.07865710025985,1.29287966739942));
#22719=CARTESIAN_POINT('Ctrl Pts',(-48.3554782973195,-6.12977840933566,
1.38797527736651));
#22720=CARTESIAN_POINT('Ctrl Pts',(-48.3539734316356,-6.14643370208422,
1.48363043830394));
#22721=CARTESIAN_POINT('Ctrl Pts',(-48.3539734316357,-6.16593130894386,
1.48373989603238));
#22722=CARTESIAN_POINT('Ctrl Pts',(-48.3473326059861,-6.06586350127576,
1.83630261430625));
#22723=CARTESIAN_POINT('Ctrl Pts',(-48.3514157821642,-6.0756803173363,1.64039290548077));
#22724=CARTESIAN_POINT('Ctrl Pts',(-48.3529551642942,-6.09455995772361,
1.6397868616514));
#22725=CARTESIAN_POINT('Ctrl Pts',(-48.3552960665089,-6.14361803658471,
1.73656127921966));
#22726=CARTESIAN_POINT('Ctrl Pts',(-48.3539734316346,-6.1605984343526,1.83394174062863));
#22727=CARTESIAN_POINT('Ctrl Pts',(-48.3539734316348,-6.17733642103886,
1.83400504229092));
#22728=CARTESIAN_POINT('Ctrl Pts',(-48.3448536057857,-6.13245845075532,
2.88748313503321));
#22729=CARTESIAN_POINT('Ctrl Pts',(-48.3512462941318,-6.14582978514638,
2.76704153887883));
#22730=CARTESIAN_POINT('Ctrl Pts',(-48.3534951017072,-6.16286923349057,
2.76641567432489));
#22731=CARTESIAN_POINT('Ctrl Pts',(-48.3552756321772,-6.19966838879309,
2.82527806458757));
#22732=CARTESIAN_POINT('Ctrl Pts',(-48.3539734316326,-6.21324540616174,
2.8847663194085));
#22733=CARTESIAN_POINT('Ctrl Pts',(-48.3539734316329,-6.22295686941885,
2.88455296200763));
#22734=CARTESIAN_POINT('Ctrl Pts',(-48.3401597427993,-6.17306838545285,
3.5897554902018));
#22735=CARTESIAN_POINT('Ctrl Pts',(-48.3481565678091,-6.19184520829409,
3.51781324186406));
#22736=CARTESIAN_POINT('Ctrl Pts',(-48.3516099900174,-6.21237399283442,
3.51681244904663));
#22737=CARTESIAN_POINT('Ctrl Pts',(-48.3545184219291,-6.24739159904061,
3.55049096194934));
#22738=CARTESIAN_POINT('Ctrl Pts',(-48.3539734316326,-6.26188042070648,
3.58517026766949));
#22739=CARTESIAN_POINT('Ctrl Pts',(-48.3539734316329,-6.26857731779884,
3.58458821640688));
#22740=CARTESIAN_POINT('Ctrl Pts',(-48.3299590819564,-6.20946968450872,
4.29147093911199));
#22741=CARTESIAN_POINT('Ctrl Pts',(-48.3399552484009,-6.23345010528184,
4.29015424448251));
#22742=CARTESIAN_POINT('Ctrl Pts',(-48.3459588358212,-6.25674581560882,
4.28885904618088));
#22743=CARTESIAN_POINT('Ctrl Pts',(-48.3529679274398,-6.29803503999844,
4.28634531541159));
#22744=CARTESIAN_POINT('Ctrl Pts',(-48.3539734316379,-6.31602855406108,
4.28512678294393));
#22745=CARTESIAN_POINT('Ctrl Pts',(-48.3539734316379,-6.32940458230551,
4.28396341998237));
#22746=CARTESIAN_POINT('',(-48.3299588608603,-6.20946977623549,4.29147093113758));
#22747=CARTESIAN_POINT('',(-48.353987706665,-6.00666333723547,0.0824317919588709));
#22748=CARTESIAN_POINT('Ctrl Pts',(-48.3299590819564,-6.2094696845087,4.291470939112));
#22749=CARTESIAN_POINT('Ctrl Pts',(-48.3401597427993,-6.17306838545285,
3.5897554902018));
#22750=CARTESIAN_POINT('Ctrl Pts',(-48.3448536057857,-6.13245845075532,
2.88748313503321));
#22751=CARTESIAN_POINT('Ctrl Pts',(-48.3481589393863,-6.04366518478258,
1.48590910739726));
#22752=CARTESIAN_POINT('Ctrl Pts',(-48.3539879394125,-6.01733942146283,
0.784522401707471));
#22753=CARTESIAN_POINT('Ctrl Pts',(-48.353987706665,-6.00666333723547,0.0824317919588709));
#22754=CARTESIAN_POINT('Ctrl Pts',(-48.3299584186682,-6.20946995968904,
4.29147091518876));
#22755=CARTESIAN_POINT('Ctrl Pts',(-48.3340747811502,-6.2193448070199,4.29092871768642));
#22756=CARTESIAN_POINT('Ctrl Pts',(-48.3375647029145,-6.22915570483183,
4.29038566954877));
#22757=CARTESIAN_POINT('Ctrl Pts',(-48.3404726016179,-6.23871408127374,
4.28984735821603));
#22758=CARTESIAN_POINT('Ctrl Pts',(-48.3435579448646,-6.24885572484959,
4.28927619828079));
#22759=CARTESIAN_POINT('Ctrl Pts',(-48.3459887705052,-6.25871184341282,
4.28871047939837));
#22760=CARTESIAN_POINT('Ctrl Pts',(-48.3478713812869,-6.26808527594661,
4.28815447282215));
#22761=CARTESIAN_POINT('Ctrl Pts',(-48.3498400177411,-6.27788702634906,
4.28757305959252));
#22762=CARTESIAN_POINT('Ctrl Pts',(-48.3512107408118,-6.28716030960557,
4.28700232501256));
#22763=CARTESIAN_POINT('Ctrl Pts',(-48.3521434975818,-6.2957252017122,4.2864432263021));
#22764=CARTESIAN_POINT('Ctrl Pts',(-48.353157498511,-6.30503610551134,4.28583542946793));
#22765=CARTESIAN_POINT('Ctrl Pts',(-48.3536561387394,-6.31350977078185,
4.28524139166978));
#22766=CARTESIAN_POINT('Ctrl Pts',(-48.3538589105089,-6.32097498479566,
4.28465714448851));
#22767=CARTESIAN_POINT('Ctrl Pts',(-48.3539396358021,-6.32394695466908,
4.28442455035012));
#22768=CARTESIAN_POINT('Ctrl Pts',(-48.3539734197696,-6.32675971428296,
4.28419345399841));
#22769=CARTESIAN_POINT('Ctrl Pts',(-48.3539734316348,-6.32940458230554,
4.28396341998237));
#22770=CARTESIAN_POINT('Ctrl Pts',(-48.3539734316379,-6.14692278878557,
0.0824317919393188));
#22771=CARTESIAN_POINT('Ctrl Pts',(-48.3539734316379,-6.12148849588211,
0.0824317919463454));
#22772=CARTESIAN_POINT('Ctrl Pts',(-48.3553963304166,-6.10694539169998,
0.082431791952385));
#22773=CARTESIAN_POINT('Ctrl Pts',(-48.3536309301691,-6.05386667280685,
0.0824317919690549));
#22774=CARTESIAN_POINT('Ctrl Pts',(-48.3539881721587,-6.02801550569024,
0.082431791959394));
#22775=CARTESIAN_POINT('Ctrl Pts',(-48.353987706665,-6.00666333723547,0.0824317919588709));
#22776=CARTESIAN_POINT('Ctrl Pts',(-48.353987706665,-6.00666333723547,0.0824317919588709));
#22777=CARTESIAN_POINT('Ctrl Pts',(-48.3539878230381,-6.01200137934917,
-0.268613512915165));
#22778=CARTESIAN_POINT('Ctrl Pts',(-48.3525306312174,-6.02125184123468,
-0.619482841767479));
#22779=CARTESIAN_POINT('Ctrl Pts',(-48.3492030226894,-6.04818290219387,
-1.32089560047537));
#22780=CARTESIAN_POINT('Ctrl Pts',(-48.3473326059821,-6.06586350126756,
-1.67143903033095));
#22781=CARTESIAN_POINT('Ctrl Pts',(-48.3448536057816,-6.13245845073776,
-2.72261955097263));
#22782=CARTESIAN_POINT('Ctrl Pts',(-48.3401597427964,-6.17306838542386,
-3.42489190599315));
#22783=CARTESIAN_POINT('Ctrl Pts',(-48.3299590819564,-6.20946968446904,
-4.12660735477694));
#22784=CARTESIAN_POINT('Ctrl Pts',(-48.3539881721587,-6.02801550569024,
0.082431791959394));
#22785=CARTESIAN_POINT('Ctrl Pts',(-48.3539286009819,-6.03090918789793,
-0.190411563683277));
#22786=CARTESIAN_POINT('Ctrl Pts',(-48.3536168472025,-6.03698783585276,
-0.486015178076197));
#22787=CARTESIAN_POINT('Ctrl Pts',(-48.3523529181877,-6.05935112779389,
-1.1285756344005));
#22788=CARTESIAN_POINT('Ctrl Pts',(-48.351415782162,-6.07568031732935,-1.47552932150819));
#22789=CARTESIAN_POINT('Ctrl Pts',(-48.3512462941307,-6.14582978513439,
-2.60217795485319));
#22790=CARTESIAN_POINT('Ctrl Pts',(-48.3481565678094,-6.19184520827618,
-3.35294965774719));
#22791=CARTESIAN_POINT('Ctrl Pts',(-48.3399552484008,-6.23345010526292,
-4.12529066038733));
#22792=CARTESIAN_POINT('Ctrl Pts',(-48.3536309301691,-6.05386667280685,
0.0824317919690549));
#22793=CARTESIAN_POINT('Ctrl Pts',(-48.353628599321,-6.05382055712278,-0.190198224047172));
#22794=CARTESIAN_POINT('Ctrl Pts',(-48.3537318827846,-6.05830967273253,
-0.485651979211756));
#22795=CARTESIAN_POINT('Ctrl Pts',(-48.3533876456657,-6.07865710025591,
-1.1280160834437));
#22796=CARTESIAN_POINT('Ctrl Pts',(-48.352955164293,-6.0945599577187,-1.47492327768737));
#22797=CARTESIAN_POINT('Ctrl Pts',(-48.3534951017072,-6.16286923348297,
-2.60155209033893));
#22798=CARTESIAN_POINT('Ctrl Pts',(-48.3516099900184,-6.21237399282373,
-3.35194886501225));
#22799=CARTESIAN_POINT('Ctrl Pts',(-48.3459588358212,-6.25674581559982,
-4.12399546219981));
#22800=CARTESIAN_POINT('Ctrl Pts',(-48.3553963304166,-6.10694539169998,
0.082431791952385));
#22801=CARTESIAN_POINT('Ctrl Pts',(-48.3553975542495,-6.1069582237576,-0.228911445986326));
#22802=CARTESIAN_POINT('Ctrl Pts',(-48.3555328009921,-6.11145963930882,
-0.551717780090184));
#22803=CARTESIAN_POINT('Ctrl Pts',(-48.3554782973193,-6.12977840933436,
-1.22311169345771));
#22804=CARTESIAN_POINT('Ctrl Pts',(-48.3552960665088,-6.14361803658328,
-1.57169769530953));
#22805=CARTESIAN_POINT('Ctrl Pts',(-48.3552756321777,-6.19966838879149,
-2.66041448067764));
#22806=CARTESIAN_POINT('Ctrl Pts',(-48.35451842193,-6.24739159903889,-3.38562737803406));
#22807=CARTESIAN_POINT('Ctrl Pts',(-48.3529679274398,-6.29803503999889,
-4.12148173153879));
#22808=CARTESIAN_POINT('Ctrl Pts',(-48.3539734316379,-6.12148849588211,
0.0824317919463454));
#22809=CARTESIAN_POINT('Ctrl Pts',(-48.3539734316379,-6.12148849588211,
-0.267838007542064));
#22810=CARTESIAN_POINT('Ctrl Pts',(-48.3539734316373,-6.12687873284897,
-0.618146779815187));
#22811=CARTESIAN_POINT('Ctrl Pts',(-48.3539734316356,-6.14643370208422,
-1.31876685441475));
#22812=CARTESIAN_POINT('Ctrl Pts',(-48.3539734316346,-6.1605984343526,-1.66907815674119));
#22813=CARTESIAN_POINT('Ctrl Pts',(-48.3539734316326,-6.21324540616174,
-2.71990273552632));
#22814=CARTESIAN_POINT('Ctrl Pts',(-48.3539734316326,-6.26188042070648,
-3.42030668379082));
#22815=CARTESIAN_POINT('Ctrl Pts',(-48.3539734316379,-6.31602855406106,
-4.12026319906529));
#22816=CARTESIAN_POINT('Ctrl Pts',(-48.3539734316379,-6.14692278878554,
0.0824317919393188));
#22817=CARTESIAN_POINT('Ctrl Pts',(-48.3539734316379,-6.14692278878554,
-0.26791586067219));
#22818=CARTESIAN_POINT('Ctrl Pts',(-48.3539734316373,-6.15072449281721,
-0.618263513283698));
#22819=CARTESIAN_POINT('Ctrl Pts',(-48.3539734316357,-6.16593130894387,
-1.31887631215375));
#22820=CARTESIAN_POINT('Ctrl Pts',(-48.3539734316348,-6.17733642103887,
-1.66914145841228));
#22821=CARTESIAN_POINT('Ctrl Pts',(-48.3539734316329,-6.22295686941886,
-2.71968937812899));
#22822=CARTESIAN_POINT('Ctrl Pts',(-48.3539734316329,-6.26857731779886,
-3.41972463252824));
#22823=CARTESIAN_POINT('Ctrl Pts',(-48.3539734316379,-6.32940458230553,
-4.11909983610373));
#22824=CARTESIAN_POINT('',(-48.3299588715825,-6.2094697717474,-4.12660734718935));
#22825=CARTESIAN_POINT('Ctrl Pts',(-48.3539734316352,-6.32940458230556,
-4.11909983610374));
#22826=CARTESIAN_POINT('Ctrl Pts',(-48.3539734035773,-6.32271656818349,
-4.1196815175845));
#22827=CARTESIAN_POINT('Ctrl Pts',(-48.3537588682918,-6.31495176722325,
-4.12027027606706));
#22828=CARTESIAN_POINT('Ctrl Pts',(-48.3531104436363,-6.30626433210883,
-4.12087194787713));
#22829=CARTESIAN_POINT('Ctrl Pts',(-48.3525181613788,-6.29832907912765,
-4.12142152527963));
#22830=CARTESIAN_POINT('Ctrl Pts',(-48.3515619729455,-6.28962376480999,
-4.12198189920433));
#22831=CARTESIAN_POINT('Ctrl Pts',(-48.3500740656231,-6.28030805427421,
-4.12255384985624));
#22832=CARTESIAN_POINT('Ctrl Pts',(-48.3486583623796,-6.27144440972966,
-4.12309804530501));
#22833=CARTESIAN_POINT('Ctrl Pts',(-48.346759863173,-6.26202846118927,-4.12365269510123));
#22834=CARTESIAN_POINT('Ctrl Pts',(-48.3442565190529,-6.25223759022,-4.12421502554824));
#22835=CARTESIAN_POINT('Ctrl Pts',(-48.3418721744595,-6.24291214028606,
-4.12475062492918));
#22836=CARTESIAN_POINT('Ctrl Pts',(-48.3389382149631,-6.23324739180464,
-4.1252931197551));
#22837=CARTESIAN_POINT('Ctrl Pts',(-48.3353866501404,-6.22342541541245,
-4.12583763768076));
#22838=CARTESIAN_POINT('Ctrl Pts',(-48.3337145952874,-6.21880128939694,
-4.12609399336779));
#22839=CARTESIAN_POINT('Ctrl Pts',(-48.3319062879416,-6.21414266599987,
-4.12635076735834));
#22840=CARTESIAN_POINT('Ctrl Pts',(-48.3299584508348,-6.20946994630412,
-4.12660733201417));
#22841=CARTESIAN_POINT('Ctrl Pts',(-48.3299590819564,-6.20946968446903,
-4.12660735477694));
#22842=CARTESIAN_POINT('Ctrl Pts',(-48.3401597427964,-6.17306838542386,
-3.42489190599315));
#22843=CARTESIAN_POINT('Ctrl Pts',(-48.3448536057816,-6.13245845073776,
-2.72261955097264));
#22844=CARTESIAN_POINT('Ctrl Pts',(-48.3481589393823,-6.04366518477749,
-1.32104552345038));
#22845=CARTESIAN_POINT('Ctrl Pts',(-48.3539879394112,-6.01733942146287,
-0.619658817789202));
#22846=CARTESIAN_POINT('Ctrl Pts',(-48.353987706665,-6.00666333723547,0.0824317919588709));
#22847=CARTESIAN_POINT('Ctrl Pts',(-48.353987706665,-6.00666333723547,0.0824317919588709));
#22848=CARTESIAN_POINT('Ctrl Pts',(-48.3539875902912,-6.00132529512179,
-0.268613512915427));
#22849=CARTESIAN_POINT('Ctrl Pts',(-48.3525301621487,-5.99973567328071,
-0.61971075554883));
#22850=CARTESIAN_POINT('Ctrl Pts',(-48.3427993418052,-5.99820579736973,
-1.32203631868417));
#22851=CARTESIAN_POINT('Ctrl Pts',(-48.3345259496042,-5.99826554329983,
-1.67326463918611));
#22852=CARTESIAN_POINT('Ctrl Pts',(-48.2936298161322,-5.99214762358588,
-2.72718702102022));
#22853=CARTESIAN_POINT('Ctrl Pts',(-48.2504292399901,-5.99475664078831,
-3.42843979396698));
#22854=CARTESIAN_POINT('Ctrl Pts',(-48.1943732865555,-6.00705144710501,
-4.12954958707863));
#22855=CARTESIAN_POINT('Ctrl Pts',(-48.3539878230381,-6.01200137934917,
-0.268613512915165));
#22856=CARTESIAN_POINT('Ctrl Pts',(-48.353045974614,-6.00879525432293,-0.541629932872173));
#22857=CARTESIAN_POINT('Ctrl Pts',(-48.3509583174043,-6.00835114797862,
-0.832717795175944));
#22858=CARTESIAN_POINT('Ctrl Pts',(-48.3410826227118,-6.00829173506032,
-1.44781988530405));
#22859=CARTESIAN_POINT('Ctrl Pts',(-48.3332754509119,-6.00864450579782,
-1.77183914806596));
#22860=CARTESIAN_POINT('Ctrl Pts',(-48.2931970947834,-6.00381665756611,
-2.78846829166608));
#22861=CARTESIAN_POINT('Ctrl Pts',(-48.2516773068029,-6.00697011627401,
-3.46541553672362));
#22862=CARTESIAN_POINT('Ctrl Pts',(-48.1993391601324,-6.01900581052064,
-4.12960227429863));
#22863=CARTESIAN_POINT('Ctrl Pts',(-48.3525306312174,-6.02125184123468,
-0.619482841767479));
#22864=CARTESIAN_POINT('Ctrl Pts',(-48.3513305951669,-6.01828947675528,
-0.832372601140253));
#22865=CARTESIAN_POINT('Ctrl Pts',(-48.3489425213176,-6.01789996842498,
-1.07740316093052));
#22866=CARTESIAN_POINT('Ctrl Pts',(-48.3390430002211,-6.01814206511767,
-1.6217484591999));
#22867=CARTESIAN_POINT('Ctrl Pts',(-48.3315028514982,-6.0187257861079,-1.92107075008537));
#22868=CARTESIAN_POINT('Ctrl Pts',(-48.2925867091325,-6.01569196512697,
-2.8854776362454));
#22869=CARTESIAN_POINT('Ctrl Pts',(-48.2530217284169,-6.02014444454683,
-3.52759295130783));
#22870=CARTESIAN_POINT('Ctrl Pts',(-48.2060243727241,-6.0312811715619,-4.12973535553853));
#22871=CARTESIAN_POINT('Ctrl Pts',(-48.3492030226894,-6.04818290219387,
-1.32089560047537));
#22872=CARTESIAN_POINT('Ctrl Pts',(-48.3474462842631,-6.04432658406742,
-1.44625764078141));
#22873=CARTESIAN_POINT('Ctrl Pts',(-48.3443564160926,-6.04289085428131,
-1.62044191118949));
#22874=CARTESIAN_POINT('Ctrl Pts',(-48.3339923325724,-6.04173521007275,
-2.04438575562572));
#22875=CARTESIAN_POINT('Ctrl Pts',(-48.3266822403782,-6.04195544060936,
-2.2941547701618));
#22876=CARTESIAN_POINT('Ctrl Pts',(-48.2905861997417,-6.04033961883411,
-3.12373338268601));
#22877=CARTESIAN_POINT('Ctrl Pts',(-48.2556497470813,-6.04594588203863,
-3.6727550861618));
#22878=CARTESIAN_POINT('Ctrl Pts',(-48.2204933169654,-6.05467770199135,
-4.13029598569448));
#22879=CARTESIAN_POINT('Ctrl Pts',(-48.3473326059821,-6.06586350126756,
-1.67143903033095));
#22880=CARTESIAN_POINT('Ctrl Pts',(-48.3452802018275,-6.06089216511434,
-1.76939839258765));
#22881=CARTESIAN_POINT('Ctrl Pts',(-48.3417903804858,-6.05836696394193,
-1.91879286634364));
#22882=CARTESIAN_POINT('Ctrl Pts',(-48.330986629329,-6.0555205802838,-2.29309144146787));
#22883=CARTESIAN_POINT('Ctrl Pts',(-48.3236392144589,-6.05514353309318,
-2.51800435397685));
#22884=CARTESIAN_POINT('Ctrl Pts',(-48.2891989250228,-6.0531346611475,-3.26497816498047));
#22885=CARTESIAN_POINT('Ctrl Pts',(-48.2569333441317,-6.05857299125762,
-3.75573980643155));
#22886=CARTESIAN_POINT('Ctrl Pts',(-48.2282770486149,-6.06579887137955,
-4.13072353461054));
#22887=CARTESIAN_POINT('Ctrl Pts',(-48.3448536057816,-6.13245845073776,
-2.72261955097264));
#22888=CARTESIAN_POINT('Ctrl Pts',(-48.3416407743715,-6.12571278892215,
-2.78284525790236));
#22889=CARTESIAN_POINT('Ctrl Pts',(-48.336607865393,-6.11975101509667,-2.87982117794571));
#22890=CARTESIAN_POINT('Ctrl Pts',(-48.3235830578589,-6.109355998997,-3.11912188340943));
#22891=CARTESIAN_POINT('Ctrl Pts',(-48.3155720249862,-6.10489083403431,
-3.26145170376736));
#22892=CARTESIAN_POINT('Ctrl Pts',(-48.285129064075,-6.09364276612035,-3.71424370742436));
#22893=CARTESIAN_POINT('Ctrl Pts',(-48.2603125971885,-6.09193010339171,
-3.99151086881468));
#22894=CARTESIAN_POINT('Ctrl Pts',(-48.2497657836928,-6.09473681170808,
-4.1326484023275));
#22895=CARTESIAN_POINT('Ctrl Pts',(-48.3401597427964,-6.17306838542386,
-3.42489190599315));
#22896=CARTESIAN_POINT('Ctrl Pts',(-48.3361613302899,-6.16367997399771,
-3.46086303011612));
#22897=CARTESIAN_POINT('Ctrl Pts',(-48.3302694595612,-6.15479195321228,
-3.52283172259502));
#22898=CARTESIAN_POINT('Ctrl Pts',(-48.3160467255223,-6.13882811012296,
-3.66842757813698));
#22899=CARTESIAN_POINT('Ctrl Pts',(-48.307715862212,-6.13175228781906,-3.75205474120005));
#22900=CARTESIAN_POINT('Ctrl Pts',(-48.2810866692031,-6.11446024442978,
-3.98991893707404));
#22901=CARTESIAN_POINT('Ctrl Pts',(-48.2619367151003,-6.10813589078396,
-4.13111411250191));
#22902=CARTESIAN_POINT('Ctrl Pts',(-48.2616083272502,-6.10812801481237,
-4.13478794209722));
#22903=CARTESIAN_POINT('Ctrl Pts',(-48.3299590819564,-6.20946968446904,
-4.12660735477694));
#22904=CARTESIAN_POINT('Ctrl Pts',(-48.3249609987342,-6.1974794740721,-4.12726570197174));
#22905=CARTESIAN_POINT('Ctrl Pts',(-48.3188308025825,-6.18527410478074,
-4.12793443793977));
#22906=CARTESIAN_POINT('Ctrl Pts',(-48.3054305681492,-6.16205725105381,
-4.12937020672336));
#22907=CARTESIAN_POINT('Ctrl Pts',(-48.2981605298677,-6.15104576661825,
-4.13013723953891));
#22908=CARTESIAN_POINT('Ctrl Pts',(-48.2763272274221,-6.12223844456225,
-4.13270206220845));
#22909=CARTESIAN_POINT('Ctrl Pts',(-48.2619179788887,-6.10843369230012,
-4.13475573974244));
#22910=CARTESIAN_POINT('Ctrl Pts',(-48.2616069550931,-6.10843371318471,
-4.13831849503753));
#22911=CARTESIAN_POINT('Ctrl Pts',(-48.3299590819564,-6.20946968446903,
-4.12660735477694));
#22912=CARTESIAN_POINT('Ctrl Pts',(-48.319962915512,-6.18548926367518,-4.12792404916654));
#22913=CARTESIAN_POINT('Ctrl Pts',(-48.3054382973496,-6.16064820730356,
-4.12928229864908));
#22914=CARTESIAN_POINT('Ctrl Pts',(-48.2763272274221,-6.12223844456225,
-4.13270206220845));
#22915=CARTESIAN_POINT('Ctrl Pts',(-48.2619179788887,-6.10843369230012,
-4.13475573974244));
#22916=CARTESIAN_POINT('Ctrl Pts',(-48.2616069550931,-6.10843371318472,
-4.13831849503754));
#22917=CARTESIAN_POINT('',(-48.1943732865555,-6.00705144710502,-4.12954958707863));
#22918=CARTESIAN_POINT('Ctrl Pts',(-48.2616069550931,-6.10843371318472,
-4.13831849503754));
#22919=CARTESIAN_POINT('Ctrl Pts',(-48.2616096994074,-6.10782231644003,
-4.1312573891569));
#22920=CARTESIAN_POINT('Ctrl Pts',(-48.2142367808633,-6.05486890076757,
-4.12976033595866));
#22921=CARTESIAN_POINT('Ctrl Pts',(-48.1943732865555,-6.00705144710502,
-4.12954958707863));
#22922=CARTESIAN_POINT('Ctrl Pts',(-48.1943732865555,-6.00705144710502,
-4.12954958707863));
#22923=CARTESIAN_POINT('Ctrl Pts',(-48.2504292399901,-5.99475664078831,
-3.42843979396698));
#22924=CARTESIAN_POINT('Ctrl Pts',(-48.2936298161323,-5.99214762358588,
-2.72718702102021));
#22925=CARTESIAN_POINT('Ctrl Pts',(-48.3481579940948,-6.00030484987115,
-1.32195717857475));
#22926=CARTESIAN_POINT('Ctrl Pts',(-48.3539874739176,-5.99598725300811,
-0.619658817789722));
#22927=CARTESIAN_POINT('Ctrl Pts',(-48.353987706665,-6.00666333723547,0.0824317919588709));
#22928=CARTESIAN_POINT('Ctrl Pts',(-48.353987706665,-6.00666333723547,0.0824317919588709));
#22929=CARTESIAN_POINT('Ctrl Pts',(-48.3539872411712,-5.9853111687807,0.0824317919583475));
#22930=CARTESIAN_POINT('Ctrl Pts',(-48.353628932479,-5.96223275463528,0.0824317919477567));
#22931=CARTESIAN_POINT('Ctrl Pts',(-48.3495242804801,-5.92795641804994,
0.0824317919456884));
#22932=CARTESIAN_POINT('Ctrl Pts',(-48.3539734316379,-5.90583775506839,
0.0824317919453202));
#22933=CARTESIAN_POINT('Ctrl Pts',(-48.3539734316379,-5.88746284406389,
0.0824317919393457));
#22934=CARTESIAN_POINT('Ctrl Pts',(-48.3539875902912,-6.00132529512179,
-0.268613512915427));
#22935=CARTESIAN_POINT('Ctrl Pts',(-48.3539275501301,-5.98270666392102,
-0.190757692317236));
#22936=CARTESIAN_POINT('Ctrl Pts',(-48.3536632315908,-5.96240686080377,
-0.173571652624935));
#22937=CARTESIAN_POINT('Ctrl Pts',(-48.3495016480342,-5.92787973562318,
-0.195374050181301));
#22938=CARTESIAN_POINT('Ctrl Pts',(-48.353973431638,-5.90583775506839,-0.234362487437545));
#22939=CARTESIAN_POINT('Ctrl Pts',(-48.3539734316379,-5.88746284406389,
-0.26885562075853));
#22940=CARTESIAN_POINT('Ctrl Pts',(-48.3525301621487,-5.99973567328071,
-0.61971075554883));
#22941=CARTESIAN_POINT('Ctrl Pts',(-48.352733527773,-5.98152768121118,-0.48634291779545));
#22942=CARTESIAN_POINT('Ctrl Pts',(-48.3522992264081,-5.96239709811723,
-0.46057610468301));
#22943=CARTESIAN_POINT('Ctrl Pts',(-48.3473885441251,-5.92723732580308,
-0.501601281232533));
#22944=CARTESIAN_POINT('Ctrl Pts',(-48.3508557705022,-5.90562906540036,
-0.568393270900862));
#22945=CARTESIAN_POINT('Ctrl Pts',(-48.3501520759131,-5.88746284406389,
-0.620143038727584));
#22946=CARTESIAN_POINT('Ctrl Pts',(-48.3427993418052,-5.99820579736973,
-1.32203631868417));
#22947=CARTESIAN_POINT('Ctrl Pts',(-48.3443675175985,-5.97907559060215,
-1.12899680959845));
#22948=CARTESIAN_POINT('Ctrl Pts',(-48.3432090309159,-5.96099214798805,
-1.09680529223567));
#22949=CARTESIAN_POINT('Ctrl Pts',(-48.3361366892894,-5.9251130175414,-1.16128319669793));
#22950=CARTESIAN_POINT('Ctrl Pts',(-48.3366948692374,-5.9049506781467,-1.25795261852717));
#22951=CARTESIAN_POINT('Ctrl Pts',(-48.3348648315385,-5.8874628440639,-1.32263498783777));
#22952=CARTESIAN_POINT('Ctrl Pts',(-48.3345259496042,-5.99826554329983,
-1.67326463918611));
#22953=CARTESIAN_POINT('Ctrl Pts',(-48.3370692580606,-5.9777471823027,-1.47607399037158));
#22954=CARTESIAN_POINT('Ctrl Pts',(-48.3353565172368,-5.95954166014514,
-1.44603650619017));
#22955=CARTESIAN_POINT('Ctrl Pts',(-48.3269346991117,-5.9236034688997,-1.51473806899513));
#22956=CARTESIAN_POINT('Ctrl Pts',(-48.3256515256245,-5.90448098056108,
-1.61347711598476));
#22957=CARTESIAN_POINT('Ctrl Pts',(-48.3233989425165,-5.8874628440639,-1.67383952952183));
#22958=CARTESIAN_POINT('Ctrl Pts',(-48.3072618606229,-5.99418693015719,
-2.37587956040885));
#22959=CARTESIAN_POINT('Ctrl Pts',(-48.3087333779557,-5.97194742955361,
-2.2284105390898));
#22960=CARTESIAN_POINT('Ctrl Pts',(-48.3062335055684,-5.95413393118536,
-2.2069034605042));
#22961=CARTESIAN_POINT('Ctrl Pts',(-48.2977571519412,-5.91998502842413,
-2.25918163584876));
#22962=CARTESIAN_POINT('Ctrl Pts',(-48.295070923821,-5.90343694889075,-2.33296688978062));
#22963=CARTESIAN_POINT('Ctrl Pts',(-48.2928171719614,-5.8874628440639,-2.37608253350143));
#22964=CARTESIAN_POINT('Ctrl Pts',(-48.289645694342,-5.99381953117215,-2.72684648395123));
#22965=CARTESIAN_POINT('Ctrl Pts',(-48.2899913250448,-5.9708180255258,-2.60397205002056));
#22966=CARTESIAN_POINT('Ctrl Pts',(-48.2869150459205,-5.95257589046839,
-2.58894422957247));
#22967=CARTESIAN_POINT('Ctrl Pts',(-48.2785859525854,-5.91860436677926,
-2.63542225668577));
#22968=CARTESIAN_POINT('Ctrl Pts',(-48.2755338718776,-5.90286261480602,
-2.69692810424823));
#22969=CARTESIAN_POINT('Ctrl Pts',(-48.2737012896825,-5.8874628440639,-2.72712100634181));
#22970=CARTESIAN_POINT('Ctrl Pts',(-48.247215395667,-5.99717808806688,-3.4284040490082));
#22971=CARTESIAN_POINT('Ctrl Pts',(-48.2437182975085,-5.97321241327166,
-3.36074991074874));
#22972=CARTESIAN_POINT('Ctrl Pts',(-48.2392225168896,-5.95314193699471,
-3.35655320341621));
#22973=CARTESIAN_POINT('Ctrl Pts',(-48.2313449268639,-5.91737158402251,
-3.38631956483236));
#22974=CARTESIAN_POINT('Ctrl Pts',(-48.2285187244,-5.90176568155596,-3.42028263358126));
#22975=CARTESIAN_POINT('Ctrl Pts',(-48.2278104516838,-5.8874628440639,-3.42894804748533));
#22976=CARTESIAN_POINT('Ctrl Pts',(-48.2224012632728,-6.00090404394666,
-3.77899469052281));
#22977=CARTESIAN_POINT('Ctrl Pts',(-48.2161873228831,-5.97673620504532,
-3.74196626054616));
#22978=CARTESIAN_POINT('Ctrl Pts',(-48.2108487060109,-5.95526602423799,
-3.74211938381146));
#22979=CARTESIAN_POINT('Ctrl Pts',(-48.2032756172259,-5.91751946291063,
-3.76097220601848));
#22980=CARTESIAN_POINT('Ctrl Pts',(-48.2010411453131,-5.90124308239061,
-3.77967190496021));
#22981=CARTESIAN_POINT('Ctrl Pts',(-48.2010354948423,-5.8874628440639,-3.77973662633642));
#22982=CARTESIAN_POINT('Ctrl Pts',(-48.1943732865555,-6.00705144710501,
-4.12954958707863));
#22983=CARTESIAN_POINT('Ctrl Pts',(-48.1844415394016,-5.98314272027373,
-4.12944421263861));
#22984=CARTESIAN_POINT('Ctrl Pts',(-48.178454383799,-5.9599264156786,-4.12964628233308));
#22985=CARTESIAN_POINT('Ctrl Pts',(-48.1714459461707,-5.91876732373883,
-4.13010310894204));
#22986=CARTESIAN_POINT('Ctrl Pts',(-48.170424664145,-5.90082453639419,-4.13035786585651));
#22987=CARTESIAN_POINT('Ctrl Pts',(-48.170424664145,-5.8874628440639,-4.13035786585651));
#22988=CARTESIAN_POINT('Ctrl Pts',(-48.1943732865555,-6.00705144710502,
-4.12954958707862));
#22989=CARTESIAN_POINT('Ctrl Pts',(-48.1899403654158,-5.99638006180393,
-4.129502554409));
#22990=CARTESIAN_POINT('Ctrl Pts',(-48.1862445826294,-5.9858106003976,-4.1295124996258));
#22991=CARTESIAN_POINT('Ctrl Pts',(-48.1832154572887,-5.97555360442599,
-4.12955963932632));
#22992=CARTESIAN_POINT('Ctrl Pts',(-48.1799757201013,-5.96458345048952,
-4.12961005659982));
#22993=CARTESIAN_POINT('Ctrl Pts',(-48.1774980373401,-5.95397176603297,
-4.12970297530113));
#22994=CARTESIAN_POINT('Ctrl Pts',(-48.1756402817456,-5.94395259925277,
-4.12980930460529));
#22995=CARTESIAN_POINT('Ctrl Pts',(-48.1736701824512,-5.93332754531064,
-4.1299220639412));
#22996=CARTESIAN_POINT('Ctrl Pts',(-48.1723957131875,-5.92336957191581,
-4.13004977115199));
#22997=CARTESIAN_POINT('Ctrl Pts',(-48.1716028722098,-5.91431731008252,
-4.13015382200399));
#22998=CARTESIAN_POINT('Ctrl Pts',(-48.1707100966236,-5.90412404486024,
-4.1302709880726));
#22999=CARTESIAN_POINT('Ctrl Pts',(-48.170424664145,-5.89507967138156,-4.13035786585652));
#23000=CARTESIAN_POINT('Ctrl Pts',(-48.170424664145,-5.8874628440639,-4.13035786585652));
#23001=CARTESIAN_POINT('Ctrl Pts',(-48.3539734316379,-5.88746284406389,
0.0824317919393457));
#23002=CARTESIAN_POINT('Ctrl Pts',(-48.3539734316379,-5.90583775506839,
0.0824317919453202));
#23003=CARTESIAN_POINT('Ctrl Pts',(-48.3495242804801,-5.92795641804994,
0.0824317919456884));
#23004=CARTESIAN_POINT('Ctrl Pts',(-48.353628932479,-5.96223275463528,0.0824317919477567));
#23005=CARTESIAN_POINT('Ctrl Pts',(-48.3539872411712,-5.9853111687807,0.0824317919583475));
#23006=CARTESIAN_POINT('Ctrl Pts',(-48.353987706665,-6.00666333723547,0.0824317919588709));
#23007=CARTESIAN_POINT('Ctrl Pts',(-48.353987706665,-6.00666333723547,0.0824317919588709));
#23008=CARTESIAN_POINT('Ctrl Pts',(-48.3539875902919,-6.00132529512177,
0.433477096832907));
#23009=CARTESIAN_POINT('Ctrl Pts',(-48.3525301621497,-5.99973567328063,
0.784574339470114));
#23010=CARTESIAN_POINT('Ctrl Pts',(-48.3427993418055,-5.9982057973697,1.48689990262106));
#23011=CARTESIAN_POINT('Ctrl Pts',(-48.3345259496034,-5.9982655432999,1.8381282231348));
#23012=CARTESIAN_POINT('Ctrl Pts',(-48.3072618606178,-5.99418693015788,
2.540743144389));
#23013=CARTESIAN_POINT('Ctrl Pts',(-48.2896456943372,-5.99381953117289,
2.89171006791637));
#23014=CARTESIAN_POINT('Ctrl Pts',(-48.2472153956642,-5.99717808806743,
3.59326763292906));
#23015=CARTESIAN_POINT('Ctrl Pts',(-48.2224012632718,-6.00090404394695,
3.94385827441437));
#23016=CARTESIAN_POINT('Ctrl Pts',(-48.1943732865555,-6.00705144710499,
4.29441317095732));
#23017=CARTESIAN_POINT('Ctrl Pts',(-48.3539872411712,-5.9853111687807,0.0824317919583475));
#23018=CARTESIAN_POINT('Ctrl Pts',(-48.3539275501302,-5.98270666392057,
0.355621276231302));
#23019=CARTESIAN_POINT('Ctrl Pts',(-48.3527335277731,-5.98152768121041,
0.651206501710543));
#23020=CARTESIAN_POINT('Ctrl Pts',(-48.3443675175979,-5.97907559060113,
1.2938603935253));
#23021=CARTESIAN_POINT('Ctrl Pts',(-48.3370692580592,-5.97774718230175,
1.64093757430917));
#23022=CARTESIAN_POINT('Ctrl Pts',(-48.3087333779502,-5.97194742955337,
2.39327412306098));
#23023=CARTESIAN_POINT('Ctrl Pts',(-48.2899913250396,-5.97081802552575,
2.76883563397861));
#23024=CARTESIAN_POINT('Ctrl Pts',(-48.2437182975056,-5.97321241327176,
3.52561349466635));
#23025=CARTESIAN_POINT('Ctrl Pts',(-48.216187322882,-5.9767362050454,3.90682984443646));
#23026=CARTESIAN_POINT('Ctrl Pts',(-48.1844415394016,-5.98314272027372,
4.29430779651733));
#23027=CARTESIAN_POINT('Ctrl Pts',(-48.353628932479,-5.96223275463528,0.0824317919477567));
#23028=CARTESIAN_POINT('Ctrl Pts',(-48.3536632315906,-5.96240686080333,
0.338435236520447));
#23029=CARTESIAN_POINT('Ctrl Pts',(-48.3522992264079,-5.96239709811649,
0.625439688580834));
#23030=CARTESIAN_POINT('Ctrl Pts',(-48.3432090309151,-5.96099214798705,
1.26166887614506));
#23031=CARTESIAN_POINT('Ctrl Pts',(-48.3353565172354,-5.95954166014419,
1.61090009010881));
#23032=CARTESIAN_POINT('Ctrl Pts',(-48.306233505564,-5.95413393118495,2.37176704445063));
#23033=CARTESIAN_POINT('Ctrl Pts',(-48.2869150459164,-5.95257589046815,
2.75380781351011));
#23034=CARTESIAN_POINT('Ctrl Pts',(-48.2392225168873,-5.95314193699467,
3.52141678732466));
#23035=CARTESIAN_POINT('Ctrl Pts',(-48.21084870601,-5.95526602423798,3.90698296769951));
#23036=CARTESIAN_POINT('Ctrl Pts',(-48.178454383799,-5.95992641567858,4.29450986621179));
#23037=CARTESIAN_POINT('Ctrl Pts',(-48.3495242804801,-5.92795641804994,
0.0824317919456884));
#23038=CARTESIAN_POINT('Ctrl Pts',(-48.349501648034,-5.92787973562296,0.360237634072677));
#23039=CARTESIAN_POINT('Ctrl Pts',(-48.3473885441248,-5.92723732580272,
0.666464865124364));
#23040=CARTESIAN_POINT('Ctrl Pts',(-48.3361366892888,-5.92511301754091,
1.32614678059277));
#23041=CARTESIAN_POINT('Ctrl Pts',(-48.3269346991108,-5.92360346889921,
1.67960165289253));
#23042=CARTESIAN_POINT('Ctrl Pts',(-48.2977571519393,-5.91998502842383,
2.42404521975457));
#23043=CARTESIAN_POINT('Ctrl Pts',(-48.2785859525836,-5.91860436677904,
2.80028584058811));
#23044=CARTESIAN_POINT('Ctrl Pts',(-48.2313449268628,-5.91737158402241,
3.55118314872339));
#23045=CARTESIAN_POINT('Ctrl Pts',(-48.2032756172255,-5.91751946291058,
3.92583578990169));
#23046=CARTESIAN_POINT('Ctrl Pts',(-48.1714459461707,-5.91876732373881,
4.29496669282072));
#23047=CARTESIAN_POINT('Ctrl Pts',(-48.3539734316379,-5.90583775506839,
0.0824317919453202));
#23048=CARTESIAN_POINT('Ctrl Pts',(-48.3539734316379,-5.90583775506839,
0.399226071328185));
#23049=CARTESIAN_POINT('Ctrl Pts',(-48.350855770502,-5.90562906540036,0.733256854791239));
#23050=CARTESIAN_POINT('Ctrl Pts',(-48.3366948692371,-5.90495067814671,
1.42281620241652));
#23051=CARTESIAN_POINT('Ctrl Pts',(-48.3256515256241,-5.90448098056108,
1.77834069987334));
#23052=CARTESIAN_POINT('Ctrl Pts',(-48.2950709238206,-5.90343694889074,
2.49783047366717));
#23053=CARTESIAN_POINT('Ctrl Pts',(-48.2755338718772,-5.90286261480601,
2.86179168813353));
#23054=CARTESIAN_POINT('Ctrl Pts',(-48.2285187243997,-5.90176568155594,
3.58514621746359));
#23055=CARTESIAN_POINT('Ctrl Pts',(-48.201041145313,-5.90124308239059,3.94453548884082));
#23056=CARTESIAN_POINT('Ctrl Pts',(-48.170424664145,-5.90082453639417,4.29522144973519));
#23057=CARTESIAN_POINT('Ctrl Pts',(-48.3539734316379,-5.88746284406389,
0.0824317919393457));
#23058=CARTESIAN_POINT('Ctrl Pts',(-48.3539734316379,-5.88746284406389,
0.433719204637221));
#23059=CARTESIAN_POINT('Ctrl Pts',(-48.3501520759131,-5.88746284406389,
0.785006622606274));
#23060=CARTESIAN_POINT('Ctrl Pts',(-48.3348648315386,-5.88746284406389,
1.48749857171645));
#23061=CARTESIAN_POINT('Ctrl Pts',(-48.3233989425165,-5.88746284406389,
1.83870311340052));
#23062=CARTESIAN_POINT('Ctrl Pts',(-48.2928171719614,-5.88746284406389,
2.5409461173801));
#23063=CARTESIAN_POINT('Ctrl Pts',(-48.2737012896826,-5.88746284406389,
2.89198459022049));
#23064=CARTESIAN_POINT('Ctrl Pts',(-48.2278104516838,-5.88746284406388,
3.593811631364));
#23065=CARTESIAN_POINT('Ctrl Pts',(-48.2010354948423,-5.88746284406388,
3.94460021021509));
#23066=CARTESIAN_POINT('Ctrl Pts',(-48.170424664145,-5.88746284406388,4.29522144973519));
#23067=CARTESIAN_POINT('',(-48.1943732865555,-6.007051447105,4.29441317095728));
#23068=CARTESIAN_POINT('Origin',(-48.4830242383024,-5.88723161925863,4.32103607292913));
#23069=CARTESIAN_POINT('Ctrl Pts',(-48.1943732865555,-6.007051447105,4.29441317095728));
#23070=CARTESIAN_POINT('Ctrl Pts',(-48.2504292399881,-5.99475664078891,
3.59330337787145));
#23071=CARTESIAN_POINT('Ctrl Pts',(-48.293629816125,-5.99214762358688,2.89205060501605));
#23072=CARTESIAN_POINT('Ctrl Pts',(-48.3481579940962,-6.00030484987091,
1.48682076250771));
#23073=CARTESIAN_POINT('Ctrl Pts',(-48.3539874739188,-5.99598725300808,
0.784522401706929));
#23074=CARTESIAN_POINT('Ctrl Pts',(-48.353987706665,-6.00666333723547,0.0824317919588709));
#23075=CARTESIAN_POINT('Ctrl Pts',(48.5210408433891,-6.00666333723546,0.0824317919201338));
#23076=CARTESIAN_POINT('Ctrl Pts',(48.5210407270157,-6.00132529512171,-0.268613512953911));
#23077=CARTESIAN_POINT('Ctrl Pts',(48.5195832988733,-5.99973567328055,-0.61971075559112));
#23078=CARTESIAN_POINT('Ctrl Pts',(48.5098524785288,-5.99820579736961,-1.32203631874206));
#23079=CARTESIAN_POINT('Ctrl Pts',(48.5015790863268,-5.99826554329984,-1.67326463925579));
#23080=CARTESIAN_POINT('Ctrl Pts',(48.4743149973416,-5.99418693015786,-2.37587956050997));
#23081=CARTESIAN_POINT('Ctrl Pts',(48.4566988310611,-5.99381953117288,-2.72684648403734));
#23082=CARTESIAN_POINT('Ctrl Pts',(48.4142685323882,-5.99717808806743,-3.42840404905));
#23083=CARTESIAN_POINT('Ctrl Pts',(48.3894543999959,-6.00090404394696,-3.77899469053528));
#23084=CARTESIAN_POINT('Ctrl Pts',(48.3614264232796,-6.00705144710499,-4.12954958707821));
#23085=CARTESIAN_POINT('Ctrl Pts',(48.5210403778953,-5.9853111687807,0.0824317919206602));
#23086=CARTESIAN_POINT('Ctrl Pts',(48.5209806868542,-5.98270666392053,-0.190757692352299));
#23087=CARTESIAN_POINT('Ctrl Pts',(48.5197866644968,-5.98152768121036,-0.48634291783155));
#23088=CARTESIAN_POINT('Ctrl Pts',(48.5114206543214,-5.97907559060105,-1.12899680964633));
#23089=CARTESIAN_POINT('Ctrl Pts',(48.5041223947826,-5.97774718230167,-1.4760739904302));
#23090=CARTESIAN_POINT('Ctrl Pts',(48.475786514674,-5.97194742955333,-2.22841053918201));
#23091=CARTESIAN_POINT('Ctrl Pts',(48.4570444617636,-5.97081802552572,-2.60397205009964));
#23092=CARTESIAN_POINT('Ctrl Pts',(48.4107714342297,-5.97321241327177,-3.36074991078733));
#23093=CARTESIAN_POINT('Ctrl Pts',(48.3832404596062,-5.97673620504541,-3.7419662605574));
#23094=CARTESIAN_POINT('Ctrl Pts',(48.3514946761257,-5.98314272027372,-4.12944421263819));
#23095=CARTESIAN_POINT('Ctrl Pts',(48.5206820692032,-5.96223275463527,0.0824317919312382));
#23096=CARTESIAN_POINT('Ctrl Pts',(48.5207163683146,-5.96240686080331,-0.173571652641453));
#23097=CARTESIAN_POINT('Ctrl Pts',(48.5193523631318,-5.96239709811646,-0.46057610470184));
#23098=CARTESIAN_POINT('Ctrl Pts',(48.5102621676387,-5.96099214798699,-1.09680529226608));
#23099=CARTESIAN_POINT('Ctrl Pts',(48.5024096539591,-5.95954166014412,-1.44603650622985));
#23100=CARTESIAN_POINT('Ctrl Pts',(48.473286642288,-5.95413393118491,-2.20690346057166));
#23101=CARTESIAN_POINT('Ctrl Pts',(48.4539681826404,-5.95257589046813,-2.58894422963113));
#23102=CARTESIAN_POINT('Ctrl Pts',(48.4062756536114,-5.95314193699467,-3.35655320344563));
#23103=CARTESIAN_POINT('Ctrl Pts',(48.3779018427341,-5.95526602423799,-3.74211938382045));
#23104=CARTESIAN_POINT('Ctrl Pts',(48.3455075205231,-5.95992641567859,-4.12964628233266));
#23105=CARTESIAN_POINT('Ctrl Pts',(48.5165774172042,-5.92795641804992,0.0824317919333195));
#23106=CARTESIAN_POINT('Ctrl Pts',(48.516554784758,-5.92787973562295,-0.195374050193665));
#23107=CARTESIAN_POINT('Ctrl Pts',(48.5144416808488,-5.9272373258027,-0.501601281245333));
#23108=CARTESIAN_POINT('Ctrl Pts',(48.5031898260128,-5.92511301754087,-1.16128319671373));
#23109=CARTESIAN_POINT('Ctrl Pts',(48.4939878358348,-5.92360346889917,-1.51473806901351));
#23110=CARTESIAN_POINT('Ctrl Pts',(48.4648102886634,-5.9199850284238,-2.25918163587555));
#23111=CARTESIAN_POINT('Ctrl Pts',(48.4456390893077,-5.91860436677902,-2.63542225670908));
#23112=CARTESIAN_POINT('Ctrl Pts',(48.3983980635869,-5.91737158402241,-3.38631956484433));
#23113=CARTESIAN_POINT('Ctrl Pts',(48.3703287539496,-5.91751946291058,-3.76097220602262));
#23114=CARTESIAN_POINT('Ctrl Pts',(48.3384990828948,-5.91876732373882,-4.13010310894162));
#23115=CARTESIAN_POINT('Ctrl Pts',(48.521026568362,-5.90583775506839,0.0824317919337002));
#23116=CARTESIAN_POINT('Ctrl Pts',(48.521026568362,-5.90583775506839,-0.23436248744916));
#23117=CARTESIAN_POINT('Ctrl Pts',(48.5179089072261,-5.90562906540036,-0.568393270912183));
#23118=CARTESIAN_POINT('Ctrl Pts',(48.5037480059612,-5.90495067814671,-1.25795261853744));
#23119=CARTESIAN_POINT('Ctrl Pts',(48.4927046623482,-5.90448098056109,-1.61347711599428));
#23120=CARTESIAN_POINT('Ctrl Pts',(48.4621240605447,-5.90343694889074,-2.3329668897881));
#23121=CARTESIAN_POINT('Ctrl Pts',(48.4425870086013,-5.90286261480601,-2.69692810425446));
#23122=CARTESIAN_POINT('Ctrl Pts',(48.3955718611238,-5.90176568155594,-3.4202826335845));
#23123=CARTESIAN_POINT('Ctrl Pts',(48.3680942820371,-5.90124308239059,-3.77967190496174));
#23124=CARTESIAN_POINT('Ctrl Pts',(48.3374778008691,-5.90082453639417,-4.1303578658561));
#23125=CARTESIAN_POINT('Ctrl Pts',(48.521026568362,-5.88746284406389,0.082431791939678));
#23126=CARTESIAN_POINT('Ctrl Pts',(48.521026568362,-5.88746284406389,-0.268855620758191));
#23127=CARTESIAN_POINT('Ctrl Pts',(48.5172052126372,-5.88746284406389,-0.620143038727212));
#23128=CARTESIAN_POINT('Ctrl Pts',(48.5019179682627,-5.88746284406389,-1.32263498783737));
#23129=CARTESIAN_POINT('Ctrl Pts',(48.4904520792406,-5.88746284406389,-1.67383952952145));
#23130=CARTESIAN_POINT('Ctrl Pts',(48.4598703086855,-5.88746284406389,-2.37608253350103));
#23131=CARTESIAN_POINT('Ctrl Pts',(48.4407544264067,-5.88746284406388,-2.7271210063414));
#23132=CARTESIAN_POINT('Ctrl Pts',(48.3948635884079,-5.88746284406388,-3.42894804748491));
#23133=CARTESIAN_POINT('Ctrl Pts',(48.3680886315664,-5.88746284406389,-3.77973662633601));
#23134=CARTESIAN_POINT('Ctrl Pts',(48.3374778008691,-5.88746284406389,-4.1303578658561));
#23135=CARTESIAN_POINT('',(48.5210408433891,-6.00666333723546,0.0824317919201338));
#23136=CARTESIAN_POINT('Ctrl Pts',(48.5210265683621,-5.88746284406389,0.082431791939678));
#23137=CARTESIAN_POINT('Ctrl Pts',(48.521026568362,-5.90583775506839,0.0824317919337002));
#23138=CARTESIAN_POINT('Ctrl Pts',(48.5165774172042,-5.92795641804992,0.0824317919333195));
#23139=CARTESIAN_POINT('Ctrl Pts',(48.5206820692032,-5.96223275463527,0.0824317919312382));
#23140=CARTESIAN_POINT('Ctrl Pts',(48.5210403778953,-5.9853111687807,0.0824317919206602));
#23141=CARTESIAN_POINT('Ctrl Pts',(48.5210408433891,-6.00666333723546,0.0824317919201338));
#23142=CARTESIAN_POINT('',(48.3614264232796,-6.00705144710501,-4.12954958707822));
#23143=CARTESIAN_POINT('Ctrl Pts',(48.3374778008691,-5.88746284406389,-4.1303578658561));
#23144=CARTESIAN_POINT('Ctrl Pts',(48.3374778008691,-5.89466520940775,-4.13035786585611));
#23145=CARTESIAN_POINT('Ctrl Pts',(48.3377330767287,-5.90314351486559,-4.13028019061201));
#23146=CARTESIAN_POINT('Ctrl Pts',(48.3385156183452,-5.91266355145352,-4.13017267066886));
#23147=CARTESIAN_POINT('Ctrl Pts',(48.3392385198517,-5.92145803425844,-4.13007334517968));
#23148=CARTESIAN_POINT('Ctrl Pts',(48.3404137627567,-5.93114147445238,-4.12994875887528));
#23149=CARTESIAN_POINT('Ctrl Pts',(48.342246929742,-5.94148964487018,-4.12983582017077));
#23150=CARTESIAN_POINT('Ctrl Pts',(48.344019574647,-5.95149617003371,-4.12972661014203));
#23151=CARTESIAN_POINT('Ctrl Pts',(48.3464089871042,-5.96212379582484,-4.12962842768266));
#23152=CARTESIAN_POINT('Ctrl Pts',(48.3495648080625,-5.97313476325663,-4.12957145846139));
#23153=CARTESIAN_POINT('Ctrl Pts',(48.3524876731452,-5.98333292489419,-4.12951869458479));
#23154=CARTESIAN_POINT('Ctrl Pts',(48.3560684105317,-5.99385899411776,-4.12950132106585));
#23155=CARTESIAN_POINT('Ctrl Pts',(48.3603813000572,-6.00450404015464,-4.12953941874855));
#23156=CARTESIAN_POINT('Ctrl Pts',(48.3607250425592,-6.005352463175,-4.12954245517985));
#23157=CARTESIAN_POINT('Ctrl Pts',(48.3610734091784,-6.00620163512511,-4.12954584164827));
#23158=CARTESIAN_POINT('Ctrl Pts',(48.3614264232796,-6.00705144710501,-4.12954958707822));
#23159=CARTESIAN_POINT('Ctrl Pts',(48.3614264232796,-6.00705144710501,-4.12954958707822));
#23160=CARTESIAN_POINT('Ctrl Pts',(48.4174823767122,-5.99475664078892,-3.42843979399236));
#23161=CARTESIAN_POINT('Ctrl Pts',(48.460682952849,-5.99214762358688,-2.72718702113706));
#23162=CARTESIAN_POINT('Ctrl Pts',(48.5152111308193,-6.00030484987083,-1.3219571786287));
#23163=CARTESIAN_POINT('Ctrl Pts',(48.5210406106424,-5.99598725300796,-0.619658817827956));
#23164=CARTESIAN_POINT('Ctrl Pts',(48.5210408433891,-6.00666333723546,0.0824317919201338));
#23165=CARTESIAN_POINT('Ctrl Pts',(48.5210408433891,-6.00666333723546,0.0824317919201338));
#23166=CARTESIAN_POINT('Ctrl Pts',(48.5210409597626,-6.01200137934909,-0.268613512954174));
#23167=CARTESIAN_POINT('Ctrl Pts',(48.5195837679427,-6.02125184123585,-0.619482841813776));
#23168=CARTESIAN_POINT('Ctrl Pts',(48.5162561594161,-6.04818290219915,-1.32089560055031));
#23169=CARTESIAN_POINT('Ctrl Pts',(48.5143857427094,-6.06586350127569,-1.67143903042725));
#23170=CARTESIAN_POINT('Ctrl Pts',(48.5119067425097,-6.1324584507553,-2.72261955115417));
#23171=CARTESIAN_POINT('Ctrl Pts',(48.5072128795234,-6.17306838545284,-3.42489190632274));
#23172=CARTESIAN_POINT('Ctrl Pts',(48.4970122186805,-6.20946968450871,-4.12660735523292));
#23173=CARTESIAN_POINT('Ctrl Pts',(48.5210407270157,-6.00132529512171,-0.268613512953911));
#23174=CARTESIAN_POINT('Ctrl Pts',(48.5200991113388,-6.00879525432309,-0.541629932914882));
#23175=CARTESIAN_POINT('Ctrl Pts',(48.5183837318925,-6.01828947675668,-0.832372601189314));
#23176=CARTESIAN_POINT('Ctrl Pts',(48.5144994209904,-6.04432658407318,-1.44625764085795));
#23177=CARTESIAN_POINT('Ctrl Pts',(48.5123333385556,-6.06089216512316,-1.76939839268532));
#23178=CARTESIAN_POINT('Ctrl Pts',(48.508693911101,-6.12571278894254,-2.78284525810139));
#23179=CARTESIAN_POINT('Ctrl Pts',(48.5032144670184,-6.16367997403221,-3.46086303049164));
#23180=CARTESIAN_POINT('Ctrl Pts',(48.4920141354583,-6.19747947412215,-4.12726570254766));
#23181=CARTESIAN_POINT('Ctrl Pts',(48.5195832988733,-5.99973567328055,-0.61971075559112));
#23182=CARTESIAN_POINT('Ctrl Pts',(48.5180114541292,-6.00835114797888,-0.832717795223906));
#23183=CARTESIAN_POINT('Ctrl Pts',(48.5159956580433,-6.01789996842705,-1.077403160991));
#23184=CARTESIAN_POINT('Ctrl Pts',(48.5114095528202,-6.04289085428948,-1.62044191129696));
#23185=CARTESIAN_POINT('Ctrl Pts',(48.5088435172146,-6.05836696395436,-1.91879286648555));
#23186=CARTESIAN_POINT('Ctrl Pts',(48.5036610021237,-6.11975101512501,-2.8798211782362));
#23187=CARTESIAN_POINT('Ctrl Pts',(48.497322596291,-6.15479195325803,-3.52283172309684));
#23188=CARTESIAN_POINT('Ctrl Pts',(48.4858839393065,-6.18527410484421,-4.12793443867102));
#23189=CARTESIAN_POINT('Ctrl Pts',(48.5098524785288,-5.99820579736961,-1.32203631874206));
#23190=CARTESIAN_POINT('Ctrl Pts',(48.5081357594357,-6.0082917350608,-1.44781988536826));
#23191=CARTESIAN_POINT('Ctrl Pts',(48.5060961369459,-6.0181420651212,-1.62174845929102));
#23192=CARTESIAN_POINT('Ctrl Pts',(48.5010454692996,-6.04173521008612,-2.04438575580717));
#23193=CARTESIAN_POINT('Ctrl Pts',(48.4980397660576,-6.05552058030391,-2.29309144171275));
#23194=CARTESIAN_POINT('Ctrl Pts',(48.4906361945903,-6.10935599904101,-3.11912188389239));
#23195=CARTESIAN_POINT('Ctrl Pts',(48.4830998622531,-6.13882811018934,-3.66842757888082));
#23196=CARTESIAN_POINT('Ctrl Pts',(48.4724837048732,-6.1620572511385,-4.12937020770049));
#23197=CARTESIAN_POINT('Ctrl Pts',(48.5015790863268,-5.99826554329984,-1.67326463925579));
#23198=CARTESIAN_POINT('Ctrl Pts',(48.5003285876348,-6.00864450579842,-1.77183914814116));
#23199=CARTESIAN_POINT('Ctrl Pts',(48.498555988222,-6.01872578611223,-1.92107075019569));
#23200=CARTESIAN_POINT('Ctrl Pts',(48.4937353771045,-6.0419554406255,-2.29415477038631));
#23201=CARTESIAN_POINT('Ctrl Pts',(48.4906923511867,-6.05514353311736,-2.51800435428045));
#23202=CARTESIAN_POINT('Ctrl Pts',(48.4826251617171,-6.10489083408601,-3.26145170435135));
#23203=CARTESIAN_POINT('Ctrl Pts',(48.4747689989427,-6.13175228789483,-3.75205474205961));
#23204=CARTESIAN_POINT('Ctrl Pts',(48.4652136665916,-6.15104576671075,-4.13013724060659));
#23205=CARTESIAN_POINT('Ctrl Pts',(48.460682952849,-5.99214762358688,-2.72718702113706));
#23206=CARTESIAN_POINT('Ctrl Pts',(48.4602502315003,-6.00381665756758,-2.78846829178684));
#23207=CARTESIAN_POINT('Ctrl Pts',(48.4596398458504,-6.01569196513298,-2.88547763641065));
#23208=CARTESIAN_POINT('Ctrl Pts',(48.457639336462,-6.04033961885395,-3.12373338298816));
#23209=CARTESIAN_POINT('Ctrl Pts',(48.4562520617447,-6.05313466117661,-3.26497816537503));
#23210=CARTESIAN_POINT('Ctrl Pts',(48.4521822008009,-6.09364276617912,-3.7142437081182));
#23211=CARTESIAN_POINT('Ctrl Pts',(48.4481398059304,-6.11446024451103,-3.98991893800781));
#23212=CARTESIAN_POINT('Ctrl Pts',(48.4433803641459,-6.12223844465216,-4.13270206324732));
#23213=CARTESIAN_POINT('Ctrl Pts',(48.4174823767122,-5.99475664078892,-3.42843979399236));
#23214=CARTESIAN_POINT('Ctrl Pts',(48.418730443525,-6.00697011627484,-3.46541553675024));
#23215=CARTESIAN_POINT('Ctrl Pts',(48.4200748651391,-6.02014444454773,-3.52759295133352));
#23216=CARTESIAN_POINT('Ctrl Pts',(48.422702883804,-6.0459458820395,-3.67275508618324));
#23217=CARTESIAN_POINT('Ctrl Pts',(48.4239864808546,-6.05857299125839,-3.75573980644969));
#23218=CARTESIAN_POINT('Ctrl Pts',(48.4273657339121,-6.09193010339208,-3.99151086882235));
#23219=CARTESIAN_POINT('Ctrl Pts',(48.4289898518245,-6.10813589078396,-4.13111411250188));
#23220=CARTESIAN_POINT('Ctrl Pts',(48.4289711156128,-6.10843369230009,-4.13475573974202));
#23221=CARTESIAN_POINT('Ctrl Pts',(48.3614264232796,-6.00705144710499,-4.12954958707821));
#23222=CARTESIAN_POINT('Ctrl Pts',(48.3663922968565,-6.01900581052063,-4.12960227429821));
#23223=CARTESIAN_POINT('Ctrl Pts',(48.3730775094482,-6.03128117156189,-4.12973535553811));
#23224=CARTESIAN_POINT('Ctrl Pts',(48.3875464536895,-6.05467770199134,-4.13029598569406));
#23225=CARTESIAN_POINT('Ctrl Pts',(48.395330185339,-6.06579887137953,-4.13072353461011));
#23226=CARTESIAN_POINT('Ctrl Pts',(48.4168189204169,-6.09473681170807,-4.13264840232708));
#23227=CARTESIAN_POINT('Ctrl Pts',(48.4286614639744,-6.10812801481235,-4.1347879420968));
#23228=CARTESIAN_POINT('Ctrl Pts',(48.4286600918172,-6.10843371318468,-4.13831849503711));
#23229=CARTESIAN_POINT('Ctrl Pts',(48.3614264232796,-6.00705144710501,-4.12954958707822));
#23230=CARTESIAN_POINT('Ctrl Pts',(48.3812898236076,-6.05486867452979,-4.1297603349611));
#23231=CARTESIAN_POINT('Ctrl Pts',(48.4286623878632,-6.1078218153655,-4.13125737499063));
#23232=CARTESIAN_POINT('Ctrl Pts',(48.428660091853,-6.1084337045031,-4.1383183948133));
#23233=CARTESIAN_POINT('',(48.4970119975844,-6.2094697762355,-4.1266073472585));
#23234=CARTESIAN_POINT('Ctrl Pts',(48.4286601057169,-6.10843371319293,-4.13831833592522));
#23235=CARTESIAN_POINT('Ctrl Pts',(48.4289715446248,-6.1084341033154,-4.13475567859721));
#23236=CARTESIAN_POINT('Ctrl Pts',(48.4433805808296,-6.12223873054926,-4.13270203779284));
#23237=CARTESIAN_POINT('Ctrl Pts',(48.4724914340735,-6.16064820739694,-4.12928229972635));
#23238=CARTESIAN_POINT('Ctrl Pts',(48.4870160522361,-6.18548926373558,-4.12792404986242));
#23239=CARTESIAN_POINT('Ctrl Pts',(48.4970122186805,-6.2094696845087,-4.12660735523292));
#23240=CARTESIAN_POINT('Ctrl Pts',(48.4970122186805,-6.2094696845087,-4.12660735523292));
#23241=CARTESIAN_POINT('Ctrl Pts',(48.5072128795234,-6.17306838545284,-3.42489190632274));
#23242=CARTESIAN_POINT('Ctrl Pts',(48.5119067425097,-6.1324584507553,-2.72261955115417));
#23243=CARTESIAN_POINT('Ctrl Pts',(48.5152120761093,-6.04366518478249,-1.32104552351828));
#23244=CARTESIAN_POINT('Ctrl Pts',(48.5210410761362,-6.01733942146272,-0.619658817828478));
#23245=CARTESIAN_POINT('Ctrl Pts',(48.5210408433891,-6.00666333723546,0.0824317919201338));
#23246=CARTESIAN_POINT('Ctrl Pts',(48.5210408433891,-6.00666333723546,0.0824317919201338));
#23247=CARTESIAN_POINT('Ctrl Pts',(48.5210413088828,-6.02801550569023,0.0824317919196075));
#23248=CARTESIAN_POINT('Ctrl Pts',(48.5206840668932,-6.05386667280683,0.0824317919099577));
#23249=CARTESIAN_POINT('Ctrl Pts',(48.5224494671407,-6.10694539169997,0.0824317919266097));
#23250=CARTESIAN_POINT('Ctrl Pts',(48.521026568362,-6.1214884958821,0.0824317919326452));
#23251=CARTESIAN_POINT('Ctrl Pts',(48.521026568362,-6.14692278878552,0.0824317919396692));
#23252=CARTESIAN_POINT('Ctrl Pts',(48.5210409597626,-6.01200137934909,-0.268613512954174));
#23253=CARTESIAN_POINT('Ctrl Pts',(48.5209817377068,-6.03090918789886,-0.190411563724606));
#23254=CARTESIAN_POINT('Ctrl Pts',(48.5206817360457,-6.05382055712372,-0.190198224106269));
#23255=CARTESIAN_POINT('Ctrl Pts',(48.5224506909739,-6.10695822375808,-0.228911446012096));
#23256=CARTESIAN_POINT('Ctrl Pts',(48.521026568362,-6.12148849588209,-0.267838007555758));
#23257=CARTESIAN_POINT('Ctrl Pts',(48.521026568362,-6.14692278878552,-0.267915860671833));
#23258=CARTESIAN_POINT('Ctrl Pts',(48.5195837679427,-6.02125184123585,-0.619482841813776));
#23259=CARTESIAN_POINT('Ctrl Pts',(48.5206699839277,-6.03698783585497,-0.48601517812655));
#23260=CARTESIAN_POINT('Ctrl Pts',(48.5207850195095,-6.05830967273443,-0.4856519792755));
#23261=CARTESIAN_POINT('Ctrl Pts',(48.5225859377164,-6.11145963930962,-0.551717780117302));
#23262=CARTESIAN_POINT('Ctrl Pts',(48.5210265683614,-6.12687873284895,-0.618146779828));
#23263=CARTESIAN_POINT('Ctrl Pts',(48.5210265683614,-6.15072449281718,-0.618263513283336));
#23264=CARTESIAN_POINT('Ctrl Pts',(48.5162561594161,-6.04818290219915,-1.32089560055031));
#23265=CARTESIAN_POINT('Ctrl Pts',(48.5194060549133,-6.05935112779908,-1.12857563447696));
#23266=CARTESIAN_POINT('Ctrl Pts',(48.5204407823906,-6.07865710025979,-1.12801608352039));
#23267=CARTESIAN_POINT('Ctrl Pts',(48.5225314340435,-6.12977840933563,-1.22311169348749));
#23268=CARTESIAN_POINT('Ctrl Pts',(48.5210265683597,-6.1464337020842,-1.31876685442492));
#23269=CARTESIAN_POINT('Ctrl Pts',(48.5210265683599,-6.16593130894384,-1.31887631215337));
#23270=CARTESIAN_POINT('Ctrl Pts',(48.5143857427094,-6.06586350127569,-1.67143903042725));
#23271=CARTESIAN_POINT('Ctrl Pts',(48.5184689188876,-6.07568031733621,-1.47552932160173));
#23272=CARTESIAN_POINT('Ctrl Pts',(48.5200083010177,-6.09455995772354,-1.47492327777235));
#23273=CARTESIAN_POINT('Ctrl Pts',(48.5223492032329,-6.14361803658467,-1.57169769534062));
#23274=CARTESIAN_POINT('Ctrl Pts',(48.5210265683587,-6.16059843435258,-1.6690781567496));
#23275=CARTESIAN_POINT('Ctrl Pts',(48.5210265683589,-6.17733642103885,-1.6691414584119));
#23276=CARTESIAN_POINT('Ctrl Pts',(48.5119067425097,-6.1324584507553,-2.72261955115417));
#23277=CARTESIAN_POINT('Ctrl Pts',(48.5182994308559,-6.14582978514634,-2.60217795499973));
#23278=CARTESIAN_POINT('Ctrl Pts',(48.5205482384313,-6.16286923349053,-2.60155209044579));
#23279=CARTESIAN_POINT('Ctrl Pts',(48.5223287689013,-6.19966838879307,-2.6604144807085));
#23280=CARTESIAN_POINT('Ctrl Pts',(48.5210265683567,-6.21324540616173,-2.71990273552945));
#23281=CARTESIAN_POINT('Ctrl Pts',(48.521026568357,-6.22295686941884,-2.71968937812859));
#23282=CARTESIAN_POINT('Ctrl Pts',(48.5072128795234,-6.17306838545284,-3.42489190632274));
#23283=CARTESIAN_POINT('Ctrl Pts',(48.5152097045332,-6.19184520829409,-3.35294965798495));
#23284=CARTESIAN_POINT('Ctrl Pts',(48.5186631267415,-6.21237399283441,-3.35194886516752));
#23285=CARTESIAN_POINT('Ctrl Pts',(48.5215715586532,-6.2473915990406,-3.38562737807026));
#23286=CARTESIAN_POINT('Ctrl Pts',(48.5210265683567,-6.26188042070647,-3.42030668379043));
#23287=CARTESIAN_POINT('Ctrl Pts',(48.521026568357,-6.26857731779883,-3.41972463252783));
#23288=CARTESIAN_POINT('Ctrl Pts',(48.4970122186805,-6.20946968450871,-4.12660735523292));
#23289=CARTESIAN_POINT('Ctrl Pts',(48.507008385125,-6.23345010528183,-4.12529066060343));
#23290=CARTESIAN_POINT('Ctrl Pts',(48.5130119725454,-6.25674581560881,-4.1239954623018));
#23291=CARTESIAN_POINT('Ctrl Pts',(48.5200210641639,-6.29803503999843,-4.12148173153252));
#23292=CARTESIAN_POINT('Ctrl Pts',(48.5210265683621,-6.31602855406107,-4.12026319906486));
#23293=CARTESIAN_POINT('Ctrl Pts',(48.5210265683621,-6.3294045823055,-4.1190998361033));
#23294=CARTESIAN_POINT('Ctrl Pts',(48.4970115553921,-6.20946995968909,-4.12660733130967));
#23295=CARTESIAN_POINT('Ctrl Pts',(48.5011279178742,-6.21934480701995,-4.12606513380734));
#23296=CARTESIAN_POINT('Ctrl Pts',(48.5046178396385,-6.22915570483188,-4.12552208566969));
#23297=CARTESIAN_POINT('Ctrl Pts',(48.5075257383419,-6.2387140812738,-4.12498377433694));
#23298=CARTESIAN_POINT('Ctrl Pts',(48.5106110815886,-6.24885572484965,-4.1244126144017));
#23299=CARTESIAN_POINT('Ctrl Pts',(48.5130419072292,-6.25871184341287,-4.12384689551928));
#23300=CARTESIAN_POINT('Ctrl Pts',(48.5149245180109,-6.26808527594666,-4.12329088894307));
#23301=CARTESIAN_POINT('Ctrl Pts',(48.5168931544651,-6.2778870263491,-4.12270947571344));
#23302=CARTESIAN_POINT('Ctrl Pts',(48.5182638775358,-6.2871603096056,-4.12213874113348));
#23303=CARTESIAN_POINT('Ctrl Pts',(48.5191966343059,-6.29572520171223,-4.12157964242301));
#23304=CARTESIAN_POINT('Ctrl Pts',(48.520210635235,-6.30503610551135,-4.12097184558885));
#23305=CARTESIAN_POINT('Ctrl Pts',(48.5207092754634,-6.31350977078186,-4.1203778077907));
#23306=CARTESIAN_POINT('Ctrl Pts',(48.520912047233,-6.32097498479566,-4.11979356060943));
#23307=CARTESIAN_POINT('Ctrl Pts',(48.5209927725262,-6.32394695466906,-4.11956096647104));
#23308=CARTESIAN_POINT('Ctrl Pts',(48.5210265564937,-6.32675971428292,-4.11932987011934));
#23309=CARTESIAN_POINT('Ctrl Pts',(48.5210265683589,-6.32940458230548,-4.1190998361033));
#23310=CARTESIAN_POINT('Ctrl Pts',(48.5210265683621,-6.14692278878556,0.0824317919396692));
#23311=CARTESIAN_POINT('Ctrl Pts',(48.521026568362,-6.1214884958821,0.0824317919326452));
#23312=CARTESIAN_POINT('Ctrl Pts',(48.5224494671407,-6.10694539169997,0.0824317919266097));
#23313=CARTESIAN_POINT('Ctrl Pts',(48.5206840668932,-6.05386667280683,0.0824317919099577));
#23314=CARTESIAN_POINT('Ctrl Pts',(48.5210413088828,-6.02801550569023,0.0824317919196075));
#23315=CARTESIAN_POINT('Ctrl Pts',(48.5210408433891,-6.00666333723546,0.0824317919201338));
#23316=CARTESIAN_POINT('Ctrl Pts',(48.5210408433891,-6.00666333723546,0.0824317919201338));
#23317=CARTESIAN_POINT('Ctrl Pts',(48.5210409597624,-6.01200137934921,0.433477096794178));
#23318=CARTESIAN_POINT('Ctrl Pts',(48.519583767942,-6.02125184123474,0.784346425646489));
#23319=CARTESIAN_POINT('Ctrl Pts',(48.5162561594143,-6.04818290219394,1.48575918435436));
#23320=CARTESIAN_POINT('Ctrl Pts',(48.514385742707,-6.06586350126761,1.83630261420992));
#23321=CARTESIAN_POINT('Ctrl Pts',(48.5119067425057,-6.13245845073776,2.88748313485153));
#23322=CARTESIAN_POINT('Ctrl Pts',(48.5072128795205,-6.17306838542385,3.58975548987207));
#23323=CARTESIAN_POINT('Ctrl Pts',(48.4970122186805,-6.20946968446903,4.29147093865584));
#23324=CARTESIAN_POINT('Ctrl Pts',(48.5210413088828,-6.02801550569023,0.0824317919196075));
#23325=CARTESIAN_POINT('Ctrl Pts',(48.5209817377062,-6.03090918789795,0.355275147562284));
#23326=CARTESIAN_POINT('Ctrl Pts',(48.520669983927,-6.03698783585279,0.650878761955212));
#23327=CARTESIAN_POINT('Ctrl Pts',(48.5194060549125,-6.05935112779395,1.29343921827952));
#23328=CARTESIAN_POINT('Ctrl Pts',(48.5184689188868,-6.07568031732942,1.64039290538721));
#23329=CARTESIAN_POINT('Ctrl Pts',(48.5182994308548,-6.14582978513442,2.76704153873217));
#23330=CARTESIAN_POINT('Ctrl Pts',(48.5152097045334,-6.19184520827617,3.51781324162618));
#23331=CARTESIAN_POINT('Ctrl Pts',(48.5070083851249,-6.23345010526291,4.29015424426622));
#23332=CARTESIAN_POINT('Ctrl Pts',(48.5206840668932,-6.05386667280683,0.0824317919099577));
#23333=CARTESIAN_POINT('Ctrl Pts',(48.5206817360452,-6.05382055712278,0.355061807926185));
#23334=CARTESIAN_POINT('Ctrl Pts',(48.5207850195089,-6.05830967273254,0.650515563090774));
#23335=CARTESIAN_POINT('Ctrl Pts',(48.5204407823903,-6.07865710025595,1.29287966732272));
#23336=CARTESIAN_POINT('Ctrl Pts',(48.5200083010175,-6.09455995771876,1.63978686156639));
#23337=CARTESIAN_POINT('Ctrl Pts',(48.5205482384312,-6.162869233483,2.76641567421791));
#23338=CARTESIAN_POINT('Ctrl Pts',(48.5186631267424,-6.21237399282373,3.51681244889125));
#23339=CARTESIAN_POINT('Ctrl Pts',(48.5130119725453,-6.25674581559981,4.2888590460787));
#23340=CARTESIAN_POINT('Ctrl Pts',(48.5224494671407,-6.10694539169997,0.0824317919266097));
#23341=CARTESIAN_POINT('Ctrl Pts',(48.5224506909736,-6.1069582237576,0.393775029865316));
#23342=CARTESIAN_POINT('Ctrl Pts',(48.5225859377162,-6.11145963930881,0.716581363969174));
#23343=CARTESIAN_POINT('Ctrl Pts',(48.5225314340435,-6.12977840933438,1.3879752773367));
#23344=CARTESIAN_POINT('Ctrl Pts',(48.522349203233,-6.14361803658331,1.73656127918852));
#23345=CARTESIAN_POINT('Ctrl Pts',(48.5223287689018,-6.1996683887915,2.82527806455661));
#23346=CARTESIAN_POINT('Ctrl Pts',(48.5215715586541,-6.24739159903889,3.55049096191302));
#23347=CARTESIAN_POINT('Ctrl Pts',(48.5200210641639,-6.29803503999888,4.28634531541769));
#23348=CARTESIAN_POINT('Ctrl Pts',(48.521026568362,-6.1214884958821,0.0824317919326452));
#23349=CARTESIAN_POINT('Ctrl Pts',(48.521026568362,-6.1214884958821,0.432701591421048));
#23350=CARTESIAN_POINT('Ctrl Pts',(48.5210265683614,-6.12687873284896,0.783010363694165));
#23351=CARTESIAN_POINT('Ctrl Pts',(48.5210265683597,-6.14643370208421,1.48363043829371));
#23352=CARTESIAN_POINT('Ctrl Pts',(48.5210265683587,-6.1605984343526,1.83394174062015));
#23353=CARTESIAN_POINT('Ctrl Pts',(48.5210265683567,-6.21324540616174,2.88476631940526));
#23354=CARTESIAN_POINT('Ctrl Pts',(48.5210265683567,-6.26188042070648,3.58517026766974));
#23355=CARTESIAN_POINT('Ctrl Pts',(48.521026568362,-6.31602855406106,4.2851267829442));
#23356=CARTESIAN_POINT('Ctrl Pts',(48.521026568362,-6.14692278878552,0.0824317919396692));
#23357=CARTESIAN_POINT('Ctrl Pts',(48.521026568362,-6.14692278878553,0.432779444551172));
#23358=CARTESIAN_POINT('Ctrl Pts',(48.5210265683614,-6.15072449281719,0.783127097162674));
#23359=CARTESIAN_POINT('Ctrl Pts',(48.5210265683598,-6.16593130894386,1.48373989603271));
#23360=CARTESIAN_POINT('Ctrl Pts',(48.5210265683589,-6.17733642103886,1.83400504229124));
#23361=CARTESIAN_POINT('Ctrl Pts',(48.521026568357,-6.22295686941886,2.88455296200792));
#23362=CARTESIAN_POINT('Ctrl Pts',(48.521026568357,-6.26857731779886,3.58458821640716));
#23363=CARTESIAN_POINT('Ctrl Pts',(48.521026568362,-6.32940458230552,4.28396341998264));
#23364=CARTESIAN_POINT('',(48.4970120083066,-6.20946977174738,4.29147093106825));
#23365=CARTESIAN_POINT('Ctrl Pts',(48.5210265683593,-6.32940458230551,4.28396341998264));
#23366=CARTESIAN_POINT('Ctrl Pts',(48.5210265403013,-6.32271656818346,4.2845451014634));
#23367=CARTESIAN_POINT('Ctrl Pts',(48.5208120050159,-6.31495176722323,4.28513385994596));
#23368=CARTESIAN_POINT('Ctrl Pts',(48.5201635803604,-6.30626433210881,4.28573553175603));
#23369=CARTESIAN_POINT('Ctrl Pts',(48.5195712981029,-6.29832907912766,4.28628510915853));
#23370=CARTESIAN_POINT('Ctrl Pts',(48.5186151096696,-6.28962376481004,4.28684548308324));
#23371=CARTESIAN_POINT('Ctrl Pts',(48.5171272023472,-6.28030805427429,4.28741743373515));
#23372=CARTESIAN_POINT('Ctrl Pts',(48.5157114991037,-6.27144440972979,4.28796162918391));
#23373=CARTESIAN_POINT('Ctrl Pts',(48.5138129998971,-6.26202846118944,4.2885162789801));
#23374=CARTESIAN_POINT('Ctrl Pts',(48.511309655777,-6.25223759022023,4.28907860942712));
#23375=CARTESIAN_POINT('Ctrl Pts',(48.5089253111837,-6.24291214028634,4.28961420880806));
#23376=CARTESIAN_POINT('Ctrl Pts',(48.5059913516873,-6.23324739180496,4.29015670363398));
#23377=CARTESIAN_POINT('Ctrl Pts',(48.5024397868646,-6.22342541541284,4.29070122155964));
#23378=CARTESIAN_POINT('Ctrl Pts',(48.5007677320116,-6.21880128939719,4.29095757724668));
#23379=CARTESIAN_POINT('Ctrl Pts',(48.4989594246657,-6.21414266599999,4.29121435123722));
#23380=CARTESIAN_POINT('Ctrl Pts',(48.4970115875589,-6.20946994630411,4.29147091589307));
#23381=CARTESIAN_POINT('Ctrl Pts',(48.4970122186805,-6.20946968446902,4.29147093865584));
#23382=CARTESIAN_POINT('Ctrl Pts',(48.5072128795205,-6.17306838542385,3.58975548987207));
#23383=CARTESIAN_POINT('Ctrl Pts',(48.5119067425057,-6.13245845073776,2.88748313485153));
#23384=CARTESIAN_POINT('Ctrl Pts',(48.5152120761074,-6.04366518477756,1.48590910732938));
#23385=CARTESIAN_POINT('Ctrl Pts',(48.5210410761359,-6.01733942146297,0.784522401668223));
#23386=CARTESIAN_POINT('Ctrl Pts',(48.5210408433891,-6.00666333723546,0.0824317919201338));
#23387=CARTESIAN_POINT('Ctrl Pts',(48.5210408433891,-6.00666333723546,0.0824317919201338));
#23388=CARTESIAN_POINT('Ctrl Pts',(48.5210407270156,-6.00132529512183,0.433477096794441));
#23389=CARTESIAN_POINT('Ctrl Pts',(48.5195832988733,-5.99973567328077,0.784574339427845));
#23390=CARTESIAN_POINT('Ctrl Pts',(48.5098524785301,-5.9982057973698,1.48689990256317));
#23391=CARTESIAN_POINT('Ctrl Pts',(48.5015790863291,-5.99826554329988,1.83812822306509));
#23392=CARTESIAN_POINT('Ctrl Pts',(48.4606829528563,-5.99214762358588,2.8920506048991));
#23393=CARTESIAN_POINT('Ctrl Pts',(48.4174823767142,-5.99475664078831,3.59330337784589));
#23394=CARTESIAN_POINT('Ctrl Pts',(48.3614264232796,-6.007051447105,4.29441317095755));
#23395=CARTESIAN_POINT('Ctrl Pts',(48.5210409597624,-6.01200137934921,0.433477096794178));
#23396=CARTESIAN_POINT('Ctrl Pts',(48.5200991113386,-6.008795254323,0.706493516751188));
#23397=CARTESIAN_POINT('Ctrl Pts',(48.5180114541291,-6.0083511479787,0.997581379054961));
#23398=CARTESIAN_POINT('Ctrl Pts',(48.5081357594368,-6.0082917350604,1.61268346918306));
#23399=CARTESIAN_POINT('Ctrl Pts',(48.5003285876369,-6.00864450579789,1.93670273194495));
#23400=CARTESIAN_POINT('Ctrl Pts',(48.4602502315076,-6.00381665756613,2.95333187554498));
#23401=CARTESIAN_POINT('Ctrl Pts',(48.418730443527,-6.00697011627401,3.63027912060255));
#23402=CARTESIAN_POINT('Ctrl Pts',(48.3663922968565,-6.01900581052064,4.29446585817755));
#23403=CARTESIAN_POINT('Ctrl Pts',(48.519583767942,-6.02125184123474,0.784346425646489));
#23404=CARTESIAN_POINT('Ctrl Pts',(48.5183837318917,-6.01828947675535,0.997236185019257));
#23405=CARTESIAN_POINT('Ctrl Pts',(48.5159956580425,-6.01789996842507,1.24226674480952));
#23406=CARTESIAN_POINT('Ctrl Pts',(48.5060961369461,-6.01814206511776,1.7866120430789));
#23407=CARTESIAN_POINT('Ctrl Pts',(48.4985559882231,-6.01872578610798,2.08593433396436));
#23408=CARTESIAN_POINT('Ctrl Pts',(48.4596398458567,-6.015691965127,3.05034122012432));
#23409=CARTESIAN_POINT('Ctrl Pts',(48.420074865141,-6.02014444454683,3.69245653518678));
#23410=CARTESIAN_POINT('Ctrl Pts',(48.3730775094482,-6.0312811715619,4.29459893941745));
#23411=CARTESIAN_POINT('Ctrl Pts',(48.5162561594143,-6.04818290219394,1.48575918435436));
#23412=CARTESIAN_POINT('Ctrl Pts',(48.5144994209881,-6.0443265840675,1.61112122466037));
#23413=CARTESIAN_POINT('Ctrl Pts',(48.5114095528176,-6.0428908542814,1.78530549506845));
#23414=CARTESIAN_POINT('Ctrl Pts',(48.5010454692974,-6.04173521007285,2.20924933950468));
#23415=CARTESIAN_POINT('Ctrl Pts',(48.4937353771031,-6.04195544060946,2.45901835404076));
#23416=CARTESIAN_POINT('Ctrl Pts',(48.4576393364659,-6.04033961883415,3.28859696656493));
#23417=CARTESIAN_POINT('Ctrl Pts',(48.4227028838054,-6.04594588203863,3.83761867004076));
#23418=CARTESIAN_POINT('Ctrl Pts',(48.3875464536895,-6.05467770199135,4.29515956957339));
#23419=CARTESIAN_POINT('Ctrl Pts',(48.514385742707,-6.06586350126761,1.83630261420992));
#23420=CARTESIAN_POINT('Ctrl Pts',(48.5123333385524,-6.06089216511441,1.93426197646659));
#23421=CARTESIAN_POINT('Ctrl Pts',(48.5088435172107,-6.05836696394202,2.08365645022257));
#23422=CARTESIAN_POINT('Ctrl Pts',(48.4980397660539,-6.0555205802839,2.4579550253468));
#23423=CARTESIAN_POINT('Ctrl Pts',(48.4906923511837,-6.05514353309329,2.68286793785579));
#23424=CARTESIAN_POINT('Ctrl Pts',(48.456252061747,-6.05313466114754,3.42984174885938));
#23425=CARTESIAN_POINT('Ctrl Pts',(48.4239864808558,-6.05857299125761,3.92060339031051));
#23426=CARTESIAN_POINT('Ctrl Pts',(48.395330185339,-6.06579887137954,4.29558711848945));
#23427=CARTESIAN_POINT('Ctrl Pts',(48.5119067425057,-6.13245845073776,2.88748313485153));
#23428=CARTESIAN_POINT('Ctrl Pts',(48.5086939110956,-6.12571278892215,2.94770884178122));
#23429=CARTESIAN_POINT('Ctrl Pts',(48.5036610021172,-6.11975101509668,3.04468476182455));
#23430=CARTESIAN_POINT('Ctrl Pts',(48.4906361945831,-6.10935599899704,3.28398546728826));
#23431=CARTESIAN_POINT('Ctrl Pts',(48.4826251617104,-6.10489083403436,3.42631528764621));
#23432=CARTESIAN_POINT('Ctrl Pts',(48.4521822007991,-6.09364276612037,3.87910729130324));
#23433=CARTESIAN_POINT('Ctrl Pts',(48.4273657339126,-6.0919301033917,4.15637445269361));
#23434=CARTESIAN_POINT('Ctrl Pts',(48.4168189204168,-6.09473681170808,4.29751198620641));
#23435=CARTESIAN_POINT('Ctrl Pts',(48.5072128795205,-6.17306838542385,3.58975548987207));
#23436=CARTESIAN_POINT('Ctrl Pts',(48.503214467014,-6.16367997399769,3.62572661399501));
#23437=CARTESIAN_POINT('Ctrl Pts',(48.4973225962853,-6.15479195321227,3.68769530647388));
#23438=CARTESIAN_POINT('Ctrl Pts',(48.4830998622463,-6.13882811012295,3.83329116201583));
#23439=CARTESIAN_POINT('Ctrl Pts',(48.4747689989361,-6.13175228781906,3.9169183250789));
#23440=CARTESIAN_POINT('Ctrl Pts',(48.4481398059271,-6.11446024442977,4.15478252095291));
#23441=CARTESIAN_POINT('Ctrl Pts',(48.4289898518244,-6.10813589078395,4.29597769638082));
#23442=CARTESIAN_POINT('Ctrl Pts',(48.4286614639743,-6.10812801481236,4.29965152597613));
#23443=CARTESIAN_POINT('Ctrl Pts',(48.4970122186805,-6.20946968446903,4.29147093865584));
#23444=CARTESIAN_POINT('Ctrl Pts',(48.4920141354583,-6.19747947407209,4.29212928585064));
#23445=CARTESIAN_POINT('Ctrl Pts',(48.4858839393066,-6.18527410478073,4.29279802181868));
#23446=CARTESIAN_POINT('Ctrl Pts',(48.4724837048733,-6.16205725105381,4.29423379060227));
#23447=CARTESIAN_POINT('Ctrl Pts',(48.4652136665918,-6.15104576661825,4.29500082341782));
#23448=CARTESIAN_POINT('Ctrl Pts',(48.4433803641462,-6.12223844456224,4.29756564608736));
#23449=CARTESIAN_POINT('Ctrl Pts',(48.4289711156128,-6.10843369230011,4.29961932362136));
#23450=CARTESIAN_POINT('Ctrl Pts',(48.4286600918172,-6.1084337131847,4.30318207891644));
#23451=CARTESIAN_POINT('Ctrl Pts',(48.4970122186805,-6.20946968446902,4.29147093865584));
#23452=CARTESIAN_POINT('Ctrl Pts',(48.4870160522361,-6.18548926367516,4.29278763304545));
#23453=CARTESIAN_POINT('Ctrl Pts',(48.4724914340736,-6.16064820730357,4.29414588252798));
#23454=CARTESIAN_POINT('Ctrl Pts',(48.4433803641462,-6.12223844456224,4.29756564608736));
#23455=CARTESIAN_POINT('Ctrl Pts',(48.4289711156128,-6.10843369230011,4.29961932362136));
#23456=CARTESIAN_POINT('Ctrl Pts',(48.4286600918172,-6.10843371318471,4.30318207891645));
#23457=CARTESIAN_POINT('',(48.3614264232796,-6.00705144710501,4.29441317095755));
#23458=CARTESIAN_POINT('Ctrl Pts',(48.3614264232796,-6.00705144710501,4.29441317095755));
#23459=CARTESIAN_POINT('Ctrl Pts',(48.3635409992397,-6.01214187260733,4.29443560631099));
#23460=CARTESIAN_POINT('Ctrl Pts',(48.3658956083523,-6.01712837927263,4.29447185537051));
#23461=CARTESIAN_POINT('Ctrl Pts',(48.3684077092534,-6.02202472097697,4.29452495588205));
#23462=CARTESIAN_POINT('Ctrl Pts',(48.371521187098,-6.02809320787936,4.29459076823304));
#23463=CARTESIAN_POINT('Ctrl Pts',(48.3748781145008,-6.03402508126499,4.29468221557362));
#23464=CARTESIAN_POINT('Ctrl Pts',(48.3783993459457,-6.03985134429203,4.29480804388813));
#23465=CARTESIAN_POINT('Ctrl Pts',(48.3790315660535,-6.04089742169324,4.29483063575458));
#23466=CARTESIAN_POINT('Ctrl Pts',(48.3796692141087,-6.04194007079459,4.29485434909697));
#23467=CARTESIAN_POINT('Ctrl Pts',(48.3803119815688,-6.04297943677662,4.29487925449542));
#23468=CARTESIAN_POINT('Ctrl Pts',(48.3843513079875,-6.04951109671614,4.29503576682709));
#23469=CARTESIAN_POINT('Ctrl Pts',(48.3885900320879,-6.05591441295341,4.29523764776086));
#23470=CARTESIAN_POINT('Ctrl Pts',(48.3929742996562,-6.06221542044989,4.29551276627763));
#23471=CARTESIAN_POINT('Ctrl Pts',(48.3960776511973,-6.06667551350295,4.29570750564051));
#23472=CARTESIAN_POINT('Ctrl Pts',(48.3992541326303,-6.07108307969412,4.29593860867427));
#23473=CARTESIAN_POINT('Ctrl Pts',(48.4024930970316,-6.07544485148906,4.29622874106177));
#23474=CARTESIAN_POINT('Ctrl Pts',(48.4052050793963,-6.07909695960793,4.29647166868333));
#23475=CARTESIAN_POINT('Ctrl Pts',(48.4079603485602,-6.08271598873198,4.29675485663422));
#23476=CARTESIAN_POINT('Ctrl Pts',(48.4107527583317,-6.08630203841479,4.29711043443884));
#23477=CARTESIAN_POINT('Ctrl Pts',(48.4127529501023,-6.08887071122852,4.29736513337519));
#23478=CARTESIAN_POINT('Ctrl Pts',(48.4147730680574,-6.09142345508024,4.2976561771177));
#23479=CARTESIAN_POINT('Ctrl Pts',(48.4168100839244,-6.09395875854621,4.29801585661109));
#23480=CARTESIAN_POINT('Ctrl Pts',(48.418234877991,-6.09573208068565,4.29826743501868));
#23481=CARTESIAN_POINT('Ctrl Pts',(48.4196681079838,-6.09749699613462,4.29855158068182));
#23482=CARTESIAN_POINT('Ctrl Pts',(48.4211080201929,-6.09925274341038,4.2989009079552));
#23483=CARTESIAN_POINT('Ctrl Pts',(48.4220746454017,-6.10043139136287,4.29913541429971));
#23484=CARTESIAN_POINT('Ctrl Pts',(48.4230445410963,-6.10160612835187,4.29939833468633));
#23485=CARTESIAN_POINT('Ctrl Pts',(48.4240147544947,-6.10277497406914,4.29972059174042));
#23486=CARTESIAN_POINT('Ctrl Pts',(48.4246007385427,-6.10348092695132,4.29991522674895));
#23487=CARTESIAN_POINT('Ctrl Pts',(48.4251874240369,-6.10418538595768,4.30013130395329));
#23488=CARTESIAN_POINT('Ctrl Pts',(48.4257707705672,-6.10488492040487,4.30038975841948));
#23489=CARTESIAN_POINT('Ctrl Pts',(48.4261752550347,-6.10536996797714,4.3005689671945));
#23490=CARTESIAN_POINT('Ctrl Pts',(48.4265807298491,-6.10585567764595,4.30076899482023));
#23491=CARTESIAN_POINT('Ctrl Pts',(48.4269781707174,-6.10633304315556,4.30100976460741));
#23492=CARTESIAN_POINT('Ctrl Pts',(48.4272533213187,-6.10666352604623,4.30117645091727));
#23493=CARTESIAN_POINT('Ctrl Pts',(48.4275278798357,-6.1069938323219,4.30136389578696));
#23494=CARTESIAN_POINT('Ctrl Pts',(48.4277875302301,-6.10730907399672,4.30159035252877));
#23495=CARTESIAN_POINT('Ctrl Pts',(48.4279029314537,-6.10744918268042,4.30169100088381));
#23496=CARTESIAN_POINT('Ctrl Pts',(48.4280156595997,-6.10758666990988,4.30179985197504));
#23497=CARTESIAN_POINT('Ctrl Pts',(48.4281226651196,-6.10771844494382,4.30192110165643));
#23498=CARTESIAN_POINT('Ctrl Pts',(48.4281945740975,-6.10780699932883,4.30200258287975));
#23499=CARTESIAN_POINT('Ctrl Pts',(48.4282626359345,-6.10789132123128,4.30208695977842));
#23500=CARTESIAN_POINT('Ctrl Pts',(48.4283341793758,-6.10798127288354,4.30219267071245));
#23501=CARTESIAN_POINT('Ctrl Pts',(48.4283699510964,-6.10802624870967,4.30224552617946));
#23502=CARTESIAN_POINT('Ctrl Pts',(48.4284054731147,-6.1080710493202,4.30229992515555));
#23503=CARTESIAN_POINT('Ctrl Pts',(48.4284536139635,-6.10813310869685,4.30239026699659));
#23504=CARTESIAN_POINT('Ctrl Pts',(48.4284776843793,-6.10816413837406,4.30243543790092));
#23505=CARTESIAN_POINT('Ctrl Pts',(48.4285124648215,-6.10820885152106,4.30249946297644));
#23506=CARTESIAN_POINT('Ctrl Pts',(48.4285567328635,-6.10826888896255,4.30261832089737));
#23507=CARTESIAN_POINT('Ctrl Pts',(48.4285893193314,-6.10831308355696,4.30270581425947));
#23508=CARTESIAN_POINT('Ctrl Pts',(48.4286274756883,-6.10836602282788,4.30282297533157));
#23509=CARTESIAN_POINT('Ctrl Pts',(48.4286479760914,-6.10840319283353,4.30298683407108));
#23510=CARTESIAN_POINT('Ctrl Pts',(48.4286553250614,-6.10841651751098,4.30304557403661));
#23511=CARTESIAN_POINT('Ctrl Pts',(48.428660119669,-6.1084275022391,4.30311034818538));
#23512=CARTESIAN_POINT('Ctrl Pts',(48.4286600918174,-6.1084337131341,4.3031820783319));
#23513=CARTESIAN_POINT('Ctrl Pts',(48.3614264232796,-6.00705144710501,4.29441317095755));
#23514=CARTESIAN_POINT('Ctrl Pts',(48.4174823767142,-5.99475664078831,3.59330337784589));
#23515=CARTESIAN_POINT('Ctrl Pts',(48.4606829528563,-5.99214762358588,2.8920506048991));
#23516=CARTESIAN_POINT('Ctrl Pts',(48.51521113082,-6.00030484987122,1.48682076245375));
#23517=CARTESIAN_POINT('Ctrl Pts',(48.521040610642,-5.99598725300821,0.78452240166875));
#23518=CARTESIAN_POINT('Ctrl Pts',(48.5210408433891,-6.00666333723546,0.0824317919201338));
#23519=CARTESIAN_POINT('Ctrl Pts',(0.0835265683425695,-6.00666333723547,
-48.3550824830876));
#23520=CARTESIAN_POINT('Ctrl Pts',(0.083526568342042,-6.02801550569023,
-48.3550829485813));
#23521=CARTESIAN_POINT('Ctrl Pts',(0.0835265683323826,-6.05386667280684,
-48.3547257065917));
#23522=CARTESIAN_POINT('Ctrl Pts',(0.0835265683490379,-6.10694539169998,
-48.3564911068392));
#23523=CARTESIAN_POINT('Ctrl Pts',(0.083526568355074,-6.12148849588211,
-48.3550682080606));
#23524=CARTESIAN_POINT('Ctrl Pts',(0.0835265683620966,-6.14692278878554,
-48.3550682080606));
#23525=CARTESIAN_POINT('Ctrl Pts',(-0.26751873653172,-6.01200137934907,
-48.3550825994612));
#23526=CARTESIAN_POINT('Ctrl Pts',(-0.189316787302164,-6.03090918789885,
-48.3550233774054));
#23527=CARTESIAN_POINT('Ctrl Pts',(-0.189103447683842,-6.05382055712372,
-48.3547233757443));
#23528=CARTESIAN_POINT('Ctrl Pts',(-0.227816669589675,-6.1069582237581,
-48.3564923306724));
#23529=CARTESIAN_POINT('Ctrl Pts',(-0.266743231133337,-6.12148849588211,
-48.3550682080606));
#23530=CARTESIAN_POINT('Ctrl Pts',(-0.266821084249414,-6.14692278878554,
-48.3550682080606));
#23531=CARTESIAN_POINT('Ctrl Pts',(-0.618388065391316,-6.02125184123581,
-48.3536254076414));
#23532=CARTESIAN_POINT('Ctrl Pts',(-0.484920401704102,-6.03698783585495,
-48.3547116236264));
#23533=CARTESIAN_POINT('Ctrl Pts',(-0.48455720285307,-6.05830967273443,
-48.3548266592081));
#23534=CARTESIAN_POINT('Ctrl Pts',(-0.550623003694885,-6.11145963930963,
-48.356627577415));
#23535=CARTESIAN_POINT('Ctrl Pts',(-0.617052003405587,-6.12687873284897,
-48.3550682080599));
#23536=CARTESIAN_POINT('Ctrl Pts',(-0.617168736860925,-6.15072449281721,
-48.35506820806));
#23537=CARTESIAN_POINT('Ctrl Pts',(-1.31980082412786,-6.04818290219911,
-48.350297799115));
#23538=CARTESIAN_POINT('Ctrl Pts',(-1.12748085805452,-6.05935112779907,
-48.3534476946121));
#23539=CARTESIAN_POINT('Ctrl Pts',(-1.12692130709796,-6.07865710025978,
-48.3544824220894));
#23540=CARTESIAN_POINT('Ctrl Pts',(-1.22201691706508,-6.12977840933565,
-48.3565730737421));
#23541=CARTESIAN_POINT('Ctrl Pts',(-1.31767207800253,-6.14643370208422,
-48.3550682080582));
#23542=CARTESIAN_POINT('Ctrl Pts',(-1.31778153573098,-6.16593130894387,
-48.3550682080584));
#23543=CARTESIAN_POINT('Ctrl Pts',(-1.67034425400482,-6.06586350127566,
-48.3484273824083));
#23544=CARTESIAN_POINT('Ctrl Pts',(-1.47443454517931,-6.0756803173362,-48.3525105585865));
#23545=CARTESIAN_POINT('Ctrl Pts',(-1.47382850134994,-6.09455995772354,
-48.3540499407165));
#23546=CARTESIAN_POINT('Ctrl Pts',(-1.57060291891823,-6.14361803658469,
-48.3563908429315));
#23547=CARTESIAN_POINT('Ctrl Pts',(-1.66798338032722,-6.16059843435261,
-48.3550682080572));
#23548=CARTESIAN_POINT('Ctrl Pts',(-1.66804668198952,-6.17733642103887,
-48.3550682080574));
#23549=CARTESIAN_POINT('Ctrl Pts',(-2.72152477473183,-6.1324584507553,-48.3459483822083));
#23550=CARTESIAN_POINT('Ctrl Pts',(-2.60108317857739,-6.14582978514635,
-48.3523410705545));
#23551=CARTESIAN_POINT('Ctrl Pts',(-2.60045731402345,-6.16286923349055,
-48.3545898781298));
#23552=CARTESIAN_POINT('Ctrl Pts',(-2.65931970428615,-6.19966838879309,
-48.3563704085999));
#23553=CARTESIAN_POINT('Ctrl Pts',(-2.71880795910709,-6.21324540616175,
-48.3550682080552));
#23554=CARTESIAN_POINT('Ctrl Pts',(-2.71859460170623,-6.22295686941886,
-48.3550682080555));
#23555=CARTESIAN_POINT('Ctrl Pts',(-3.4237971299004,-6.17306838545285,-48.3412545192219));
#23556=CARTESIAN_POINT('Ctrl Pts',(-3.3518548815626,-6.1918452082941,-48.3492513442317));
#23557=CARTESIAN_POINT('Ctrl Pts',(-3.35085408874517,-6.21237399283442,
-48.35270476644));
#23558=CARTESIAN_POINT('Ctrl Pts',(-3.38453260164791,-6.24739159904062,
-48.3556131983518));
#23559=CARTESIAN_POINT('Ctrl Pts',(-3.41921190736808,-6.26188042070649,
-48.3550682080552));
#23560=CARTESIAN_POINT('Ctrl Pts',(-3.41862985610548,-6.26857731779886,
-48.3550682080555));
#23561=CARTESIAN_POINT('Ctrl Pts',(-4.1255125788106,-6.20946968450873,-48.331053858379));
#23562=CARTESIAN_POINT('Ctrl Pts',(-4.12419588418111,-6.23345010528185,
-48.3410500248235));
#23563=CARTESIAN_POINT('Ctrl Pts',(-4.12290068587948,-6.25674581560883,
-48.3470536122439));
#23564=CARTESIAN_POINT('Ctrl Pts',(-4.1203869551102,-6.29803503999845,-48.3540627038624));
#23565=CARTESIAN_POINT('Ctrl Pts',(-4.11916842264253,-6.31602855406109,
-48.3550682080606));
#23566=CARTESIAN_POINT('Ctrl Pts',(-4.11800505968097,-6.32940458230552,
-48.3550682080606));
#23567=CARTESIAN_POINT('',(-4.12551257083619,-6.20946977623546,-48.331053637283));
#23568=CARTESIAN_POINT('',(0.0835265683425695,-6.00666333723547,-48.3550824830876));
#23569=CARTESIAN_POINT('Ctrl Pts',(-4.1255125788106,-6.20946968450871,-48.331053858379));
#23570=CARTESIAN_POINT('Ctrl Pts',(-3.4237971299004,-6.17306838545285,-48.3412545192219));
#23571=CARTESIAN_POINT('Ctrl Pts',(-2.72152477473183,-6.1324584507553,-48.3459483822083));
#23572=CARTESIAN_POINT('Ctrl Pts',(-1.31995074709581,-6.04366518478245,
-48.3492537158084));
#23573=CARTESIAN_POINT('Ctrl Pts',(-0.618564041406008,-6.01733942146266,
-48.355082715835));
#23574=CARTESIAN_POINT('Ctrl Pts',(0.0835265683425695,-6.00666333723547,
-48.3550824830876));
#23575=CARTESIAN_POINT('Ctrl Pts',(-4.12551255488737,-6.20946995968897,
-48.331053195091));
#23576=CARTESIAN_POINT('Ctrl Pts',(-4.12497035738504,-6.21934480701976,
-48.335169557573));
#23577=CARTESIAN_POINT('Ctrl Pts',(-4.12442730924739,-6.22915570483163,
-48.3386594793373));
#23578=CARTESIAN_POINT('Ctrl Pts',(-4.12388899791465,-6.23871408127349,
-48.3415673780406));
#23579=CARTESIAN_POINT('Ctrl Pts',(-4.12331783797941,-6.24885572484929,
-48.3446527212873));
#23580=CARTESIAN_POINT('Ctrl Pts',(-4.12275211909699,-6.25871184341249,
-48.3470835469279));
#23581=CARTESIAN_POINT('Ctrl Pts',(-4.12219611252078,-6.26808527594625,
-48.3489661577096));
#23582=CARTESIAN_POINT('Ctrl Pts',(-4.12161469929116,-6.27788702634866,
-48.3509347941638));
#23583=CARTESIAN_POINT('Ctrl Pts',(-4.12104396471119,-6.28716030960515,
-48.3523055172344));
#23584=CARTESIAN_POINT('Ctrl Pts',(-4.12048486600072,-6.29572520171176,
-48.3532382740045));
#23585=CARTESIAN_POINT('Ctrl Pts',(-4.11987706916655,-6.3050361055109,-48.3542522749337));
#23586=CARTESIAN_POINT('Ctrl Pts',(-4.11928303136841,-6.31350977078143,
-48.3547509151621));
#23587=CARTESIAN_POINT('Ctrl Pts',(-4.11869878418713,-6.32097498479525,
-48.3549536869316));
#23588=CARTESIAN_POINT('Ctrl Pts',(-4.11846619004874,-6.32394695466881,
-48.3550344122248));
#23589=CARTESIAN_POINT('Ctrl Pts',(-4.11823509369702,-6.32675971428282,
-48.3550681961923));
#23590=CARTESIAN_POINT('Ctrl Pts',(-4.11800505968097,-6.32940458230551,
-48.3550682080575));
#23591=CARTESIAN_POINT('Ctrl Pts',(0.0835265683620966,-6.14692278878557,
-48.3550682080606));
#23592=CARTESIAN_POINT('Ctrl Pts',(0.083526568355074,-6.12148849588211,
-48.3550682080606));
#23593=CARTESIAN_POINT('Ctrl Pts',(0.0835265683490379,-6.10694539169998,
-48.3564911068392));
#23594=CARTESIAN_POINT('Ctrl Pts',(0.0835265683323826,-6.05386667280684,
-48.3547257065917));
#23595=CARTESIAN_POINT('Ctrl Pts',(0.083526568342042,-6.02801550569023,
-48.3550829485813));
#23596=CARTESIAN_POINT('Ctrl Pts',(0.0835265683425695,-6.00666333723547,
-48.3550824830876));
#23597=CARTESIAN_POINT('Ctrl Pts',(0.0835265683425695,-6.00666333723547,
-48.3550824830876));
#23598=CARTESIAN_POINT('Ctrl Pts',(0.434571873216595,-6.01200137934925,
-48.3550825994608));
#23599=CARTESIAN_POINT('Ctrl Pts',(0.785441202068902,-6.02125184123479,
-48.3536254076403));
#23600=CARTESIAN_POINT('Ctrl Pts',(1.48685396077679,-6.04818290219399,-48.3502977991125));
#23601=CARTESIAN_POINT('Ctrl Pts',(1.83739739063237,-6.06586350126766,-48.3484273824051));
#23602=CARTESIAN_POINT('Ctrl Pts',(2.88857791127407,-6.13245845073778,-48.3459483822043));
#23603=CARTESIAN_POINT('Ctrl Pts',(3.59085026629458,-6.17306838542386,-48.341254519219));
#23604=CARTESIAN_POINT('Ctrl Pts',(4.29256571507838,-6.20946968446905,-48.331053858379));
#23605=CARTESIAN_POINT('Ctrl Pts',(0.083526568342042,-6.02801550569023,
-48.3550829485813));
#23606=CARTESIAN_POINT('Ctrl Pts',(0.356369923984709,-6.03090918789797,
-48.3550233774046));
#23607=CARTESIAN_POINT('Ctrl Pts',(0.651973538377631,-6.03698783585282,
-48.3547116236253));
#23608=CARTESIAN_POINT('Ctrl Pts',(1.29453399470195,-6.05935112779398,-48.3534476946107));
#23609=CARTESIAN_POINT('Ctrl Pts',(1.64148768180965,-6.07568031732944,-48.352510558585));
#23610=CARTESIAN_POINT('Ctrl Pts',(2.76813631515469,-6.14582978513442,-48.3523410705534));
#23611=CARTESIAN_POINT('Ctrl Pts',(3.51890801804868,-6.19184520827618,-48.349251344232));
#23612=CARTESIAN_POINT('Ctrl Pts',(4.29124902068876,-6.23345010526292,-48.3410500248235));
#23613=CARTESIAN_POINT('Ctrl Pts',(0.0835265683323826,-6.05386667280684,
-48.3547257065917));
#23614=CARTESIAN_POINT('Ctrl Pts',(0.356156584348608,-6.0538205571228,-48.3547233757437));
#23615=CARTESIAN_POINT('Ctrl Pts',(0.651610339513195,-6.05830967273256,
-48.3548266592073));
#23616=CARTESIAN_POINT('Ctrl Pts',(1.29397444374515,-6.07865710025598,-48.3544824220886));
#23617=CARTESIAN_POINT('Ctrl Pts',(1.64088163798883,-6.09455995771877,-48.3540499407158));
#23618=CARTESIAN_POINT('Ctrl Pts',(2.76751045064042,-6.16286923348299,-48.3545898781298));
#23619=CARTESIAN_POINT('Ctrl Pts',(3.51790722531375,-6.21237399282374,-48.352704766441));
#23620=CARTESIAN_POINT('Ctrl Pts',(4.28995382250124,-6.25674581559981,-48.3470536122438));
#23621=CARTESIAN_POINT('Ctrl Pts',(0.0835265683490379,-6.10694539169998,
-48.3564911068392));
#23622=CARTESIAN_POINT('Ctrl Pts',(0.39486980628775,-6.10695822375761,-48.3564923306722));
#23623=CARTESIAN_POINT('Ctrl Pts',(0.717676140391613,-6.11145963930883,
-48.3566275774147));
#23624=CARTESIAN_POINT('Ctrl Pts',(1.38907005375915,-6.12977840933439,-48.356573073742));
#23625=CARTESIAN_POINT('Ctrl Pts',(1.73765605561098,-6.14361803658331,-48.3563908429315));
#23626=CARTESIAN_POINT('Ctrl Pts',(2.8263728409791,-6.1996683887915,-48.3563704086003));
#23627=CARTESIAN_POINT('Ctrl Pts',(3.55158573833553,-6.24739159903889,-48.3556131983526));
#23628=CARTESIAN_POINT('Ctrl Pts',(4.28744009184022,-6.29803503999889,-48.3540627038624));
#23629=CARTESIAN_POINT('Ctrl Pts',(0.083526568355074,-6.12148849588211,
-48.3550682080606));
#23630=CARTESIAN_POINT('Ctrl Pts',(0.433796367843485,-6.12148849588211,
-48.3550682080606));
#23631=CARTESIAN_POINT('Ctrl Pts',(0.784105140116609,-6.12687873284897,
-48.3550682080599));
#23632=CARTESIAN_POINT('Ctrl Pts',(1.48472521471617,-6.14643370208422,-48.3550682080582));
#23633=CARTESIAN_POINT('Ctrl Pts',(1.83503651704262,-6.1605984343526,-48.3550682080572));
#23634=CARTESIAN_POINT('Ctrl Pts',(2.88586109582775,-6.21324540616174,-48.3550682080552));
#23635=CARTESIAN_POINT('Ctrl Pts',(3.58626504409225,-6.26188042070648,-48.3550682080552));
#23636=CARTESIAN_POINT('Ctrl Pts',(4.28622155936672,-6.31602855406106,-48.3550682080606));
#23637=CARTESIAN_POINT('Ctrl Pts',(0.0835265683620966,-6.14692278878554,
-48.3550682080606));
#23638=CARTESIAN_POINT('Ctrl Pts',(0.433874220973607,-6.14692278878554,
-48.3550682080606));
#23639=CARTESIAN_POINT('Ctrl Pts',(0.784221873585118,-6.15072449281721,
-48.35506820806));
#23640=CARTESIAN_POINT('Ctrl Pts',(1.48483467245517,-6.16593130894387,-48.3550682080584));
#23641=CARTESIAN_POINT('Ctrl Pts',(1.83509981871371,-6.17733642103887,-48.3550682080574));
#23642=CARTESIAN_POINT('Ctrl Pts',(2.88564773843042,-6.22295686941886,-48.3550682080555));
#23643=CARTESIAN_POINT('Ctrl Pts',(3.58568299282967,-6.26857731779886,-48.3550682080555));
#23644=CARTESIAN_POINT('Ctrl Pts',(4.28505819640516,-6.32940458230553,-48.3550682080606));
#23645=CARTESIAN_POINT('',(4.29256570749077,-6.20946977174739,-48.3310536480052));
#23646=CARTESIAN_POINT('Ctrl Pts',(4.28505819640516,-6.32940458230551,-48.3550682080579));
#23647=CARTESIAN_POINT('Ctrl Pts',(4.28563987788593,-6.32271656818346,-48.3550681799999));
#23648=CARTESIAN_POINT('Ctrl Pts',(4.28622863636849,-6.31495176722324,-48.3548536447145));
#23649=CARTESIAN_POINT('Ctrl Pts',(4.28683030817856,-6.30626433210882,-48.3542052200589));
#23650=CARTESIAN_POINT('Ctrl Pts',(4.28737988558105,-6.29832907912768,-48.3536129378015));
#23651=CARTESIAN_POINT('Ctrl Pts',(4.28794025950575,-6.28962376481006,-48.3526567493682));
#23652=CARTESIAN_POINT('Ctrl Pts',(4.28851221015767,-6.28030805427432,-48.3511688420458));
#23653=CARTESIAN_POINT('Ctrl Pts',(4.28905640560643,-6.27144440972983,-48.3497531388023));
#23654=CARTESIAN_POINT('Ctrl Pts',(4.28961105540263,-6.2620284611895,-48.3478546395958));
#23655=CARTESIAN_POINT('Ctrl Pts',(4.29017338584965,-6.2522375902203,-48.3453512954757));
#23656=CARTESIAN_POINT('Ctrl Pts',(4.29070898523059,-6.24291214028641,-48.3429669508824));
#23657=CARTESIAN_POINT('Ctrl Pts',(4.29125148005651,-6.23324739180503,-48.3400329913859));
#23658=CARTESIAN_POINT('Ctrl Pts',(4.29179599798217,-6.2234254154129,-48.3364814265633));
#23659=CARTESIAN_POINT('Ctrl Pts',(4.29205235366921,-6.21880128939723,-48.3348093717102));
#23660=CARTESIAN_POINT('Ctrl Pts',(4.29230912765975,-6.214142666,-48.3330010643644));
#23661=CARTESIAN_POINT('Ctrl Pts',(4.2925656923156,-6.20946994630409,-48.3310532272575));
#23662=CARTESIAN_POINT('Ctrl Pts',(4.29256571507836,-6.20946968446903,-48.331053858379));
#23663=CARTESIAN_POINT('Ctrl Pts',(3.59085026629458,-6.17306838542386,-48.341254519219));
#23664=CARTESIAN_POINT('Ctrl Pts',(2.88857791127407,-6.13245845073778,-48.3459483822043));
#23665=CARTESIAN_POINT('Ctrl Pts',(1.4870038837518,-6.04366518477762,-48.3492537158055));
#23666=CARTESIAN_POINT('Ctrl Pts',(0.785617178090622,-6.01733942146302,
-48.3550827158341));
#23667=CARTESIAN_POINT('Ctrl Pts',(0.0835265683425695,-6.00666333723547,
-48.3550824830876));
#23668=CARTESIAN_POINT('Ctrl Pts',(0.0835265683425695,-6.00666333723547,
-48.3550824830876));
#23669=CARTESIAN_POINT('Ctrl Pts',(0.434571873216859,-6.00132529512187,
-48.3550823667139));
#23670=CARTESIAN_POINT('Ctrl Pts',(0.785669115850259,-5.99973567328082,
-48.3536249385716));
#23671=CARTESIAN_POINT('Ctrl Pts',(1.4879946789856,-5.99820579736985,-48.3438941182282));
#23672=CARTESIAN_POINT('Ctrl Pts',(1.83922299948754,-5.99826554329993,-48.3356207260272));
#23673=CARTESIAN_POINT('Ctrl Pts',(2.89314538132166,-5.99214762358589,-48.2947245925549));
#23674=CARTESIAN_POINT('Ctrl Pts',(3.59439815426843,-5.99475664078831,-48.2515240164127));
#23675=CARTESIAN_POINT('Ctrl Pts',(4.29550794738009,-6.007051447105,-48.1954680629781));
#23676=CARTESIAN_POINT('Ctrl Pts',(0.434571873216595,-6.01200137934925,
-48.3550825994608));
#23677=CARTESIAN_POINT('Ctrl Pts',(0.707588293173598,-6.00879525432306,
-48.3541407510368));
#23678=CARTESIAN_POINT('Ctrl Pts',(0.998676155477369,-6.00835114797876,
-48.3520530938273));
#23679=CARTESIAN_POINT('Ctrl Pts',(1.61377824560549,-6.00829173506045,-48.3421773991349));
#23680=CARTESIAN_POINT('Ctrl Pts',(1.9377975083674,-6.00864450579793,-48.334370227335));
#23681=CARTESIAN_POINT('Ctrl Pts',(2.95442665196754,-6.00381665756613,-48.294291871206));
#23682=CARTESIAN_POINT('Ctrl Pts',(3.63137389702508,-6.00697011627401,-48.2527720832255));
#23683=CARTESIAN_POINT('Ctrl Pts',(4.2955606346001,-6.01900581052064,-48.200433936555));
#23684=CARTESIAN_POINT('Ctrl Pts',(0.785441202068902,-6.02125184123479,
-48.3536254076403));
#23685=CARTESIAN_POINT('Ctrl Pts',(0.998330961441668,-6.01828947675541,
-48.3524253715899));
#23686=CARTESIAN_POINT('Ctrl Pts',(1.24336152123193,-6.01789996842513,-48.3500372977406));
#23687=CARTESIAN_POINT('Ctrl Pts',(1.78770681950133,-6.01814206511781,-48.3401377766442));
#23688=CARTESIAN_POINT('Ctrl Pts',(2.08702911038681,-6.01872578610802,-48.3325976279212));
#23689=CARTESIAN_POINT('Ctrl Pts',(3.05143599654687,-6.01569196512699,-48.2936814855552));
#23690=CARTESIAN_POINT('Ctrl Pts',(3.6935513116093,-6.02014444454682,-48.2541165048395));
#23691=CARTESIAN_POINT('Ctrl Pts',(4.29569371583999,-6.0312811715619,-48.2071191491467));
#23692=CARTESIAN_POINT('Ctrl Pts',(1.48685396077679,-6.04818290219399,-48.3502977991125));
#23693=CARTESIAN_POINT('Ctrl Pts',(1.61221600108281,-6.04432658406756,-48.3485410606862));
#23694=CARTESIAN_POINT('Ctrl Pts',(1.78640027149089,-6.04289085428145,-48.3454511925156));
#23695=CARTESIAN_POINT('Ctrl Pts',(2.21034411592712,-6.04173521007289,-48.3350871089954));
#23696=CARTESIAN_POINT('Ctrl Pts',(2.46011313046322,-6.04195544060948,-48.3277770168012));
#23697=CARTESIAN_POINT('Ctrl Pts',(3.28969174298747,-6.04033961883414,-48.2916809761644));
#23698=CARTESIAN_POINT('Ctrl Pts',(3.83871344646328,-6.04594588203862,-48.2567445235039));
#23699=CARTESIAN_POINT('Ctrl Pts',(4.29625434599593,-6.05467770199135,-48.221588093388));
#23700=CARTESIAN_POINT('Ctrl Pts',(1.83739739063237,-6.06586350126766,-48.3484273824051));
#23701=CARTESIAN_POINT('Ctrl Pts',(1.93535675288904,-6.06089216511445,-48.3463749782505));
#23702=CARTESIAN_POINT('Ctrl Pts',(2.08475122664503,-6.05836696394206,-48.3428851569089));
#23703=CARTESIAN_POINT('Ctrl Pts',(2.45904980176926,-6.05552058028392,-48.332081405752));
#23704=CARTESIAN_POINT('Ctrl Pts',(2.68396271427826,-6.0551435330933,-48.3247339908818));
#23705=CARTESIAN_POINT('Ctrl Pts',(3.43093652528192,-6.05313466114753,-48.2902937014455));
#23706=CARTESIAN_POINT('Ctrl Pts',(3.92169816673303,-6.0585729912576,-48.2580281205544));
#23707=CARTESIAN_POINT('Ctrl Pts',(4.29668189491198,-6.06579887137954,-48.2293718250375));
#23708=CARTESIAN_POINT('Ctrl Pts',(2.88857791127407,-6.13245845073778,-48.3459483822043));
#23709=CARTESIAN_POINT('Ctrl Pts',(2.94880361820377,-6.12571278892217,-48.3427355507941));
#23710=CARTESIAN_POINT('Ctrl Pts',(3.0457795382471,-6.11975101509669,-48.3377026418157));
#23711=CARTESIAN_POINT('Ctrl Pts',(3.28508024371081,-6.10935599899704,-48.3246778342816));
#23712=CARTESIAN_POINT('Ctrl Pts',(3.42741006406875,-6.10489083403435,-48.3166668014089));
#23713=CARTESIAN_POINT('Ctrl Pts',(3.88020206772579,-6.09364276612036,-48.2862238404977));
#23714=CARTESIAN_POINT('Ctrl Pts',(4.15746922911613,-6.0919301033917,-48.2614073736111));
#23715=CARTESIAN_POINT('Ctrl Pts',(4.29860676262894,-6.09473681170807,-48.2508605601154));
#23716=CARTESIAN_POINT('Ctrl Pts',(3.59085026629458,-6.17306838542386,-48.341254519219));
#23717=CARTESIAN_POINT('Ctrl Pts',(3.62682139041753,-6.16367997399771,-48.3372561067125));
#23718=CARTESIAN_POINT('Ctrl Pts',(3.6887900828964,-6.15479195321228,-48.3313642359839));
#23719=CARTESIAN_POINT('Ctrl Pts',(3.83438593843836,-6.13882811012295,-48.3171415019449));
#23720=CARTESIAN_POINT('Ctrl Pts',(3.91801310150143,-6.13175228781906,-48.3088106386346));
#23721=CARTESIAN_POINT('Ctrl Pts',(4.15587729737545,-6.11446024442977,-48.2821814456257));
#23722=CARTESIAN_POINT('Ctrl Pts',(4.29707247280335,-6.10813589078395,-48.263031491523));
#23723=CARTESIAN_POINT('Ctrl Pts',(4.30074630239866,-6.10812801481237,-48.2627031036729));
#23724=CARTESIAN_POINT('Ctrl Pts',(4.29256571507838,-6.20946968446905,-48.331053858379));
#23725=CARTESIAN_POINT('Ctrl Pts',(4.29322406227318,-6.1974794740721,-48.3260557751568));
#23726=CARTESIAN_POINT('Ctrl Pts',(4.29389279824122,-6.18527410478074,-48.3199255790051));
#23727=CARTESIAN_POINT('Ctrl Pts',(4.29532856702481,-6.16205725105381,-48.3065253445719));
#23728=CARTESIAN_POINT('Ctrl Pts',(4.29609559984036,-6.15104576661825,-48.2992553062903));
#23729=CARTESIAN_POINT('Ctrl Pts',(4.2986604225099,-6.12223844456225,-48.2774220038447));
#23730=CARTESIAN_POINT('Ctrl Pts',(4.30071410004389,-6.10843369230011,-48.2630127553113));
#23731=CARTESIAN_POINT('Ctrl Pts',(4.30427685533897,-6.1084337131847,-48.2627017315157));
#23732=CARTESIAN_POINT('Ctrl Pts',(4.29256571507836,-6.20946968446903,-48.331053858379));
#23733=CARTESIAN_POINT('Ctrl Pts',(4.29388240946801,-6.18548926367518,-48.3210576919346));
#23734=CARTESIAN_POINT('Ctrl Pts',(4.29524065895049,-6.16064820730358,-48.3065330737723));
#23735=CARTESIAN_POINT('Ctrl Pts',(4.2986604225099,-6.12223844456225,-48.2774220038447));
#23736=CARTESIAN_POINT('Ctrl Pts',(4.30071410004389,-6.10843369230011,-48.2630127553113));
#23737=CARTESIAN_POINT('Ctrl Pts',(4.30427685533897,-6.10843371318471,-48.2627017315157));
#23738=CARTESIAN_POINT('',(4.29550794738007,-6.00705144710501,-48.1954680629781));
#23739=CARTESIAN_POINT('Ctrl Pts',(4.30427685533897,-6.10843371318471,-48.2627017315157));
#23740=CARTESIAN_POINT('Ctrl Pts',(4.29721574945835,-6.10782231644002,-48.26270447583));
#23741=CARTESIAN_POINT('Ctrl Pts',(4.29571869626011,-6.05486890076755,-48.2153315572858));
#23742=CARTESIAN_POINT('Ctrl Pts',(4.29550794738007,-6.00705144710501,-48.1954680629781));
#23743=CARTESIAN_POINT('Ctrl Pts',(4.29550794738007,-6.00705144710501,-48.1954680629781));
#23744=CARTESIAN_POINT('Ctrl Pts',(3.59439815426845,-5.9947566407883,-48.2515240164127));
#23745=CARTESIAN_POINT('Ctrl Pts',(2.89314538132164,-5.99214762358589,-48.2947245925549));
#23746=CARTESIAN_POINT('Ctrl Pts',(1.48791553887618,-6.00030484987127,-48.349252770518));
#23747=CARTESIAN_POINT('Ctrl Pts',(0.785617178091139,-5.99598725300827,
-48.3550822503403));
#23748=CARTESIAN_POINT('Ctrl Pts',(0.0835265683425695,-6.00666333723547,
-48.3550824830876));
#23749=CARTESIAN_POINT('Ctrl Pts',(0.0835265683425695,-6.00666333723547,
-48.3550824830876));
#23750=CARTESIAN_POINT('Ctrl Pts',(0.0835265683430974,-5.9853111687807,
-48.3550820175939));
#23751=CARTESIAN_POINT('Ctrl Pts',(0.0835265683536855,-5.96223275463528,
-48.3547237089017));
#23752=CARTESIAN_POINT('Ctrl Pts',(0.0835265683557651,-5.92795641804993,
-48.3506190569028));
#23753=CARTESIAN_POINT('Ctrl Pts',(0.0835265683561427,-5.90583775506839,
-48.3550682080606));
#23754=CARTESIAN_POINT('Ctrl Pts',(0.0835265683621219,-5.88746284406389,
-48.3550682080606));
#23755=CARTESIAN_POINT('Ctrl Pts',(0.434571873216859,-6.00132529512187,
-48.3550823667139));
#23756=CARTESIAN_POINT('Ctrl Pts',(0.356716052618675,-5.98270666392106,
-48.3550223265529));
#23757=CARTESIAN_POINT('Ctrl Pts',(0.339530012926373,-5.96240686080379,
-48.3547580080134));
#23758=CARTESIAN_POINT('Ctrl Pts',(0.361332410482752,-5.92787973562318,
-48.3505964244568));
#23759=CARTESIAN_POINT('Ctrl Pts',(0.400320847739005,-5.90583775506839,
-48.3550682080606));
#23760=CARTESIAN_POINT('Ctrl Pts',(0.434813981059995,-5.88746284406389,
-48.3550682080606));
#23761=CARTESIAN_POINT('Ctrl Pts',(0.785669115850259,-5.99973567328082,
-48.3536249385716));
#23762=CARTESIAN_POINT('Ctrl Pts',(0.652301278096881,-5.98152768121126,
-48.3538283041958));
#23763=CARTESIAN_POINT('Ctrl Pts',(0.626534464984441,-5.96239709811728,
-48.3533940028309));
#23764=CARTESIAN_POINT('Ctrl Pts',(0.667559641533983,-5.92723732580308,
-48.3484833205478));
#23765=CARTESIAN_POINT('Ctrl Pts',(0.734351631202325,-5.90562906540035,
-48.3519505469248));
#23766=CARTESIAN_POINT('Ctrl Pts',(0.786101399029053,-5.88746284406389,
-48.3512468523357));
#23767=CARTESIAN_POINT('Ctrl Pts',(1.4879946789856,-5.99820579736985,-48.3438941182282));
#23768=CARTESIAN_POINT('Ctrl Pts',(1.29495516989986,-5.97907559060224,-48.3454622940215));
#23769=CARTESIAN_POINT('Ctrl Pts',(1.26276365253708,-5.96099214798812,-48.3443038073388));
#23770=CARTESIAN_POINT('Ctrl Pts',(1.32724155699937,-5.92511301754141,-48.3372314657121));
#23771=CARTESIAN_POINT('Ctrl Pts',(1.42391097882863,-5.9049506781467,-48.33778964566));
#23772=CARTESIAN_POINT('Ctrl Pts',(1.48859334813923,-5.88746284406389,-48.3359596079612));
#23773=CARTESIAN_POINT('Ctrl Pts',(1.83922299948754,-5.99826554329993,-48.3356207260272));
#23774=CARTESIAN_POINT('Ctrl Pts',(1.64203235067299,-5.9777471823028,-48.3381640344836));
#23775=CARTESIAN_POINT('Ctrl Pts',(1.61199486649158,-5.95954166014522,-48.3364512936597));
#23776=CARTESIAN_POINT('Ctrl Pts',(1.68069642929659,-5.92360346889971,-48.3280294755344));
#23777=CARTESIAN_POINT('Ctrl Pts',(1.77943547628625,-5.90448098056108,-48.3267463020471));
#23778=CARTESIAN_POINT('Ctrl Pts',(1.83979788982333,-5.88746284406389,-48.3244937189391));
#23779=CARTESIAN_POINT('Ctrl Pts',(2.54183792071029,-5.99418693015723,-48.3083566370457));
#23780=CARTESIAN_POINT('Ctrl Pts',(2.3943688993912,-5.97194742955366,-48.3098281543785));
#23781=CARTESIAN_POINT('Ctrl Pts',(2.37286182080562,-5.9541339311854,-48.3073282819912));
#23782=CARTESIAN_POINT('Ctrl Pts',(2.42513999615023,-5.91998502842413,-48.2988519283639));
#23783=CARTESIAN_POINT('Ctrl Pts',(2.49892525008213,-5.90343694889074,-48.2961657002436));
#23784=CARTESIAN_POINT('Ctrl Pts',(2.54204089380294,-5.88746284406389,-48.293911948384));
#23785=CARTESIAN_POINT('Ctrl Pts',(2.89280484425267,-5.99381953117216,-48.2907404707647));
#23786=CARTESIAN_POINT('Ctrl Pts',(2.76993041032196,-5.97081802552583,-48.2910861014675));
#23787=CARTESIAN_POINT('Ctrl Pts',(2.75490258987387,-5.95257589046841,-48.2880098223432));
#23788=CARTESIAN_POINT('Ctrl Pts',(2.8013806169872,-5.91860436677926,-48.279680729008));
#23789=CARTESIAN_POINT('Ctrl Pts',(2.86288646454969,-5.90286261480602,-48.2766286483002));
#23790=CARTESIAN_POINT('Ctrl Pts',(2.89307936664327,-5.88746284406389,-48.2747960661052));
#23791=CARTESIAN_POINT('Ctrl Pts',(3.59436240930965,-5.99717808806687,-48.2483101720896));
#23792=CARTESIAN_POINT('Ctrl Pts',(3.52670827105016,-5.97321241327166,-48.2448130739311));
#23793=CARTESIAN_POINT('Ctrl Pts',(3.52251156371763,-5.95314193699471,-48.2403172933123));
#23794=CARTESIAN_POINT('Ctrl Pts',(3.55227792513379,-5.91737158402251,-48.2324397032865));
#23795=CARTESIAN_POINT('Ctrl Pts',(3.58624099388271,-5.90176568155595,-48.2296135008226));
#23796=CARTESIAN_POINT('Ctrl Pts',(3.59490640778678,-5.8874628440639,-48.2289052281065));
#23797=CARTESIAN_POINT('Ctrl Pts',(3.94495305082426,-6.00090404394666,-48.2234960396954));
#23798=CARTESIAN_POINT('Ctrl Pts',(3.9079246208476,-5.97673620504532,-48.2172820993057));
#23799=CARTESIAN_POINT('Ctrl Pts',(3.9080777441129,-5.95526602423799,-48.2119434824335));
#23800=CARTESIAN_POINT('Ctrl Pts',(3.92693056631993,-5.91751946291063,-48.2043703936485));
#23801=CARTESIAN_POINT('Ctrl Pts',(3.94563026526167,-5.9012430823906,-48.2021359217358));
#23802=CARTESIAN_POINT('Ctrl Pts',(3.94569498663788,-5.8874628440639,-48.2021302712649));
#23803=CARTESIAN_POINT('Ctrl Pts',(4.29550794738009,-6.007051447105,-48.1954680629781));
#23804=CARTESIAN_POINT('Ctrl Pts',(4.29540257294009,-5.98314272027373,-48.1855363158242));
#23805=CARTESIAN_POINT('Ctrl Pts',(4.29560464263456,-5.9599264156786,-48.1795491602216));
#23806=CARTESIAN_POINT('Ctrl Pts',(4.2960614692435,-5.91876732373882,-48.1725407225933));
#23807=CARTESIAN_POINT('Ctrl Pts',(4.29631622615797,-5.90082453639418,-48.1715194405676));
#23808=CARTESIAN_POINT('Ctrl Pts',(4.29631622615797,-5.88746284406389,-48.1715194405676));
#23809=CARTESIAN_POINT('Ctrl Pts',(4.29550794738007,-6.00705144710502,-48.1954680629781));
#23810=CARTESIAN_POINT('Ctrl Pts',(4.29546091471046,-5.99638006180393,-48.1910351418385));
#23811=CARTESIAN_POINT('Ctrl Pts',(4.2954708599273,-5.9858106003976,-48.187339359052));
#23812=CARTESIAN_POINT('Ctrl Pts',(4.29551799962782,-5.975553604426,-48.1843102337114));
#23813=CARTESIAN_POINT('Ctrl Pts',(4.29556841690132,-5.96458345048953,-48.1810704965239));
#23814=CARTESIAN_POINT('Ctrl Pts',(4.29566133560256,-5.95397176603299,-48.1785928137628));
#23815=CARTESIAN_POINT('Ctrl Pts',(4.29576766490672,-5.94395259925279,-48.1767350581682));
#23816=CARTESIAN_POINT('Ctrl Pts',(4.29588042424262,-5.93332754531067,-48.1747649588739));
#23817=CARTESIAN_POINT('Ctrl Pts',(4.29600813145345,-5.92336957191585,-48.1734904896102));
#23818=CARTESIAN_POINT('Ctrl Pts',(4.29611218230544,-5.91431731008256,-48.1726976486325));
#23819=CARTESIAN_POINT('Ctrl Pts',(4.29622934837405,-5.90412404486025,-48.1718048730462));
#23820=CARTESIAN_POINT('Ctrl Pts',(4.29631622615796,-5.89507967138156,-48.1715194405676));
#23821=CARTESIAN_POINT('Ctrl Pts',(4.29631622615797,-5.88746284406389,-48.1715194405676));
#23822=CARTESIAN_POINT('Ctrl Pts',(0.0835265683620358,-5.88746284406389,
-48.3550682080606));
#23823=CARTESIAN_POINT('Ctrl Pts',(0.0835265683561427,-5.90583775506839,
-48.3550682080606));
#23824=CARTESIAN_POINT('Ctrl Pts',(0.0835265683557651,-5.92795641804993,
-48.3506190569028));
#23825=CARTESIAN_POINT('Ctrl Pts',(0.0835265683536855,-5.96223275463528,
-48.3547237089017));
#23826=CARTESIAN_POINT('Ctrl Pts',(0.0835265683430974,-5.9853111687807,
-48.3550820175939));
#23827=CARTESIAN_POINT('Ctrl Pts',(0.0835265683425695,-6.00666333723547,
-48.3550824830876));
#23828=CARTESIAN_POINT('Ctrl Pts',(0.0835265683425695,-6.00666333723547,
-48.3550824830876));
#23829=CARTESIAN_POINT('Ctrl Pts',(-0.267518736531456,-6.00132529512168,
-48.3550823667144));
#23830=CARTESIAN_POINT('Ctrl Pts',(-0.618615979168657,-5.99973567328051,
-48.3536249385721));
#23831=CARTESIAN_POINT('Ctrl Pts',(-1.3209415423196,-5.99820579736957,-48.3438941182277));
#23832=CARTESIAN_POINT('Ctrl Pts',(-1.67216986283335,-5.9982655432998,-48.3356207260257));
#23833=CARTESIAN_POINT('Ctrl Pts',(-2.37478478408758,-5.99418693015785,
-48.3083566370402));
#23834=CARTESIAN_POINT('Ctrl Pts',(-2.72575170761495,-5.99381953117288,
-48.2907404707597));
#23835=CARTESIAN_POINT('Ctrl Pts',(-3.42730927262762,-5.99717808806743,
-48.2483101720868));
#23836=CARTESIAN_POINT('Ctrl Pts',(-3.77789991411291,-6.00090404394696,
-48.2234960396944));
#23837=CARTESIAN_POINT('Ctrl Pts',(-4.12845481065586,-6.007051447105,-48.1954680629781));
#23838=CARTESIAN_POINT('Ctrl Pts',(0.0835265683430974,-5.9853111687807,
-48.3550820175939));
#23839=CARTESIAN_POINT('Ctrl Pts',(-0.189662915929852,-5.98270666392052,
-48.3550223265528));
#23840=CARTESIAN_POINT('Ctrl Pts',(-0.485248141409092,-5.98152768121033,
-48.3538283041956));
#23841=CARTESIAN_POINT('Ctrl Pts',(-1.12790203322386,-5.97907559060103,
-48.3454622940202));
#23842=CARTESIAN_POINT('Ctrl Pts',(-1.47497921400774,-5.97774718230166,
-48.3381640344815));
#23843=CARTESIAN_POINT('Ctrl Pts',(-2.22731576275959,-5.97194742955333,
-48.3098281543727));
#23844=CARTESIAN_POINT('Ctrl Pts',(-2.60287727367722,-5.97081802552573,
-48.2910861014622));
#23845=CARTESIAN_POINT('Ctrl Pts',(-3.35965513436493,-5.97321241327177,
-48.2448130739282));
#23846=CARTESIAN_POINT('Ctrl Pts',(-3.74087148413501,-5.97673620504541,
-48.2172820993047));
#23847=CARTESIAN_POINT('Ctrl Pts',(-4.12834943621584,-5.98314272027373,
-48.1855363158243));
#23848=CARTESIAN_POINT('Ctrl Pts',(0.0835265683536855,-5.96223275463528,
-48.3547237089017));
#23849=CARTESIAN_POINT('Ctrl Pts',(-0.172476876219001,-5.9624068608033,
-48.3547580080132));
#23850=CARTESIAN_POINT('Ctrl Pts',(-0.459481328279409,-5.96239709811644,
-48.3533940028304));
#23851=CARTESIAN_POINT('Ctrl Pts',(-1.09571051584365,-5.96099214798698,
-48.3443038073375));
#23852=CARTESIAN_POINT('Ctrl Pts',(-1.44494172980739,-5.95954166014412,
-48.3364512936579));
#23853=CARTESIAN_POINT('Ctrl Pts',(-2.20580868414923,-5.95413393118492,
-48.3073282819866));
#23854=CARTESIAN_POINT('Ctrl Pts',(-2.58784945320871,-5.95257589046814,
-48.288009822339));
#23855=CARTESIAN_POINT('Ctrl Pts',(-3.35545842702323,-5.95314193699468,
-48.2403172933099));
#23856=CARTESIAN_POINT('Ctrl Pts',(-3.74102460739806,-5.955266024238,-48.2119434824327));
#23857=CARTESIAN_POINT('Ctrl Pts',(-4.12855150591032,-5.95992641567859,
-48.1795491602216));
#23858=CARTESIAN_POINT('Ctrl Pts',(0.0835265683557651,-5.92795641804993,
-48.3506190569028));
#23859=CARTESIAN_POINT('Ctrl Pts',(-0.194279273771221,-5.92787973562296,
-48.3505964244566));
#23860=CARTESIAN_POINT('Ctrl Pts',(-0.500506504822973,-5.92723732580271,
-48.3484833205473));
#23861=CARTESIAN_POINT('Ctrl Pts',(-1.16018842029139,-5.92511301754088,
-48.3372314657113));
#23862=CARTESIAN_POINT('Ctrl Pts',(-1.51364329259108,-5.92360346889918,
-48.3280294755334));
#23863=CARTESIAN_POINT('Ctrl Pts',(-2.25808685945314,-5.91998502842382,
-48.2988519283619));
#23864=CARTESIAN_POINT('Ctrl Pts',(-2.63432748028667,-5.91860436677903,
-48.2796807290063));
#23865=CARTESIAN_POINT('Ctrl Pts',(-3.38522478842194,-5.91737158402242,
-48.2324397032854));
#23866=CARTESIAN_POINT('Ctrl Pts',(-3.75987742960026,-5.91751946291059,
-48.2043703936481));
#23867=CARTESIAN_POINT('Ctrl Pts',(-4.12900833251928,-5.91876732373882,
-48.1725407225933));
#23868=CARTESIAN_POINT('Ctrl Pts',(0.0835265683561427,-5.90583775506839,
-48.3550682080606));
#23869=CARTESIAN_POINT('Ctrl Pts',(-0.233267711026719,-5.9058377550684,
-48.3550682080605));
#23870=CARTESIAN_POINT('Ctrl Pts',(-0.567298494489859,-5.90562906540037,
-48.3519505469246));
#23871=CARTESIAN_POINT('Ctrl Pts',(-1.25685784211514,-5.90495067814671,
-48.3377896456597));
#23872=CARTESIAN_POINT('Ctrl Pts',(-1.61238233957187,-5.90448098056109,
-48.3267463020468));
#23873=CARTESIAN_POINT('Ctrl Pts',(-2.33187211336571,-5.90343694889075,
-48.2961657002432));
#23874=CARTESIAN_POINT('Ctrl Pts',(-2.69583332783207,-5.90286261480602,
-48.2766286482999));
#23875=CARTESIAN_POINT('Ctrl Pts',(-3.41918785716212,-5.90176568155595,
-48.2296135008224));
#23876=CARTESIAN_POINT('Ctrl Pts',(-3.77857712853939,-5.9012430823906,-48.2021359217356));
#23877=CARTESIAN_POINT('Ctrl Pts',(-4.12926308943376,-5.90082453639418,
-48.1715194405676));
#23878=CARTESIAN_POINT('Ctrl Pts',(0.0835265683621219,-5.88746284406389,
-48.3550682080606));
#23879=CARTESIAN_POINT('Ctrl Pts',(-0.267760844335752,-5.88746284406389,
-48.3550682080606));
#23880=CARTESIAN_POINT('Ctrl Pts',(-0.619048262304891,-5.88746284406389,
-48.3512468523357));
#23881=CARTESIAN_POINT('Ctrl Pts',(-1.32154021141508,-5.88746284406389,
-48.3359596079612));
#23882=CARTESIAN_POINT('Ctrl Pts',(-1.67274475309905,-5.88746284406389,
-48.3244937189391));
#23883=CARTESIAN_POINT('Ctrl Pts',(-2.37498775707864,-5.88746284406389,
-48.2939119483841));
#23884=CARTESIAN_POINT('Ctrl Pts',(-2.72602622991902,-5.88746284406389,
-48.2747960661052));
#23885=CARTESIAN_POINT('Ctrl Pts',(-3.42785327106253,-5.88746284406389,
-48.2289052281065));
#23886=CARTESIAN_POINT('Ctrl Pts',(-3.77864184991366,-5.88746284406389,
-48.2021302712649));
#23887=CARTESIAN_POINT('Ctrl Pts',(-4.12926308943376,-5.88746284406389,
-48.1715194405676));
#23888=CARTESIAN_POINT('',(-4.12845481065586,-6.00705144710501,-48.1954680629781));
#23889=CARTESIAN_POINT('Origin',(-4.15507771262898,-5.88723161925855,-48.4841190147253));
#23890=CARTESIAN_POINT('Ctrl Pts',(-4.12845481065586,-6.00705144710501,
-48.1954680629781));
#23891=CARTESIAN_POINT('Ctrl Pts',(-3.42734501756996,-5.99475664078892,
-48.2515240164107));
#23892=CARTESIAN_POINT('Ctrl Pts',(-2.72609224471469,-5.99214762358689,
-48.2947245925476));
#23893=CARTESIAN_POINT('Ctrl Pts',(-1.32086240220623,-6.00030484987077,
-48.3492527705183));
#23894=CARTESIAN_POINT('Ctrl Pts',(-0.618564041405483,-5.99598725300791,
-48.3550822503411));
#23895=CARTESIAN_POINT('Ctrl Pts',(0.0835265683425695,-6.00666333723547,
-48.3550824830876));
#23896=CARTESIAN_POINT('Ctrl Pts',(27.6169432000905,-6.28105857414854,-39.6589503071862));
#23897=CARTESIAN_POINT('Ctrl Pts',(27.6725217924464,-6.09633085020215,-39.8274976919832));
#23898=CARTESIAN_POINT('Ctrl Pts',(27.4448729346656,-6.06008770502774,-39.939229356356));
#23899=CARTESIAN_POINT('Ctrl Pts',(28.3333834524819,-8.4789807742448,-41.8316237374642));
#23900=CARTESIAN_POINT('Ctrl Pts',(28.3922756330097,-8.30110493969029,-42.0102198945798));
#23901=CARTESIAN_POINT('Ctrl Pts',(28.1589136994597,-8.25800948638859,-42.1135427213873));
#23902=CARTESIAN_POINT('Ctrl Pts',(29.0478992516726,-10.6833293750564,-43.998461079774));
#23903=CARTESIAN_POINT('Ctrl Pts',(29.1067545955585,-10.5025148294077,-44.1769455263626));
#23904=CARTESIAN_POINT('Ctrl Pts',(28.8713287464266,-10.4623581523703,-44.2817497435117));
#23905=CARTESIAN_POINT('Ctrl Pts',(29.7611081292079,-12.8919045823054,-46.1613350574533));
#23906=CARTESIAN_POINT('Ctrl Pts',(29.8183400962187,-12.7034528674627,-46.3348964586614));
#23907=CARTESIAN_POINT('Ctrl Pts',(29.5826474545624,-12.6709337131846,-46.4458225157374));
#23908=CARTESIAN_POINT('Ctrl Pts',(27.4605785366061,-6.10843371318469,-39.9870540284924));
#23909=CARTESIAN_POINT('Ctrl Pts',(27.465458387645,-6.10756827058305,-39.982671765503));
#23910=CARTESIAN_POINT('Ctrl Pts',(27.470433835024,-6.10708538385355,-39.9783580051385));
#23911=CARTESIAN_POINT('Ctrl Pts',(27.475474250485,-6.10700426240367,-39.9741447883131));
#23912=CARTESIAN_POINT('Ctrl Pts',(27.4830348736764,-6.10688258022884,-39.967824963075));
#23913=CARTESIAN_POINT('Ctrl Pts',(27.4907409943993,-6.10766522922468,-39.9617312210474));
#23914=CARTESIAN_POINT('Ctrl Pts',(27.4984985962217,-6.10940561367496,-39.955980126062));
#23915=CARTESIAN_POINT('Ctrl Pts',(27.5023773971328,-6.11027580590009,-39.9531045785694));
#23916=CARTESIAN_POINT('Ctrl Pts',(27.5062692657206,-6.11138525201715,-39.9503148097033));
#23917=CARTESIAN_POINT('Ctrl Pts',(27.5101637009479,-6.1127398416781,-39.9476257773117));
#23918=CARTESIAN_POINT('Ctrl Pts',(27.5111373097547,-6.11307848909333,-39.9469535192137));
#23919=CARTESIAN_POINT('Ctrl Pts',(27.5121110832077,-6.11343245632765,-39.9462875574448));
#23920=CARTESIAN_POINT('Ctrl Pts',(27.5130848657175,-6.11380183251764,-39.9456281258756));
#23921=CARTESIAN_POINT('Ctrl Pts',(27.5145455394822,-6.11435589680261,-39.9446389785216));
#23922=CARTESIAN_POINT('Ctrl Pts',(27.5160062328241,-6.11494463135669,-39.9436645242677));
#23923=CARTESIAN_POINT('Ctrl Pts',(27.5174664350244,-6.11556833384706,-39.942705550843));
#23924=CARTESIAN_POINT('Ctrl Pts',(27.5189266372247,-6.11619203633743,-39.9417465774182));
#23925=CARTESIAN_POINT('Ctrl Pts',(27.5203863482847,-6.11685070666529,-39.9408030849329));
#23926=CARTESIAN_POINT('Ctrl Pts',(27.5218450747583,-6.11754464002833,-39.9398758577402));
#23927=CARTESIAN_POINT('Ctrl Pts',(27.5297560792404,-6.12130799802896,-39.9348472943937));
#23928=CARTESIAN_POINT('Ctrl Pts',(27.5374062985722,-6.12597258662812,-39.930411392287));
#23929=CARTESIAN_POINT('Ctrl Pts',(27.5447641973967,-6.13138771967645,-39.9265070394851));
#23930=CARTESIAN_POINT('Ctrl Pts',(27.5470542145033,-6.13307308497037,-39.9252918780757));
#23931=CARTESIAN_POINT('Ctrl Pts',(27.5493160954356,-6.13483149128261,-39.9241281566109));
#23932=CARTESIAN_POINT('Ctrl Pts',(27.5515493057335,-6.13665930617706,-39.9230139068561));
#23933=CARTESIAN_POINT('Ctrl Pts',(27.5527253791102,-6.13762188656503,-39.9224271105867));
#23934=CARTESIAN_POINT('Ctrl Pts',(27.5538933581835,-6.13860357319269,-39.9218540549599));
#23935=CARTESIAN_POINT('Ctrl Pts',(27.5550530642264,-6.13960373328463,-39.9212944500448));
#23936=CARTESIAN_POINT('Ctrl Pts',(27.5555765385631,-6.1400551909139,-39.9210418525753));
#23937=CARTESIAN_POINT('Ctrl Pts',(27.5560983353807,-6.14051040725671,-39.9207919716895));
#23938=CARTESIAN_POINT('Ctrl Pts',(27.5566184179837,-6.14096936706301,-39.9205448870854));
#23939=CARTESIAN_POINT('Ctrl Pts',(27.5571065033715,-6.14140009013226,-39.9203130039497));
#23940=CARTESIAN_POINT('Ctrl Pts',(27.557593149706,-6.14183402342711,-39.9200834930602));
#23941=CARTESIAN_POINT('Ctrl Pts',(27.5580783374539,-6.14227112540981,-39.9198564005236));
#23942=CARTESIAN_POINT('Ctrl Pts',(27.5650936167147,-6.14859113758576,-39.91657289312));
#23943=CARTESIAN_POINT('Ctrl Pts',(27.5718055899689,-6.15557322588934,-39.9137930036632));
#23944=CARTESIAN_POINT('Ctrl Pts',(27.5782114177422,-6.1630485902823,-39.9114693381554));
#23945=CARTESIAN_POINT('Ctrl Pts',(27.5839675375493,-6.16976576947769,-39.9093813492914));
#23946=CARTESIAN_POINT('Ctrl Pts',(27.5894017151405,-6.17677030338733,-39.9076507714992));
#23947=CARTESIAN_POINT('Ctrl Pts',(27.5945623304161,-6.18399336848785,-39.906237064347));
#23948=CARTESIAN_POINT('Ctrl Pts',(27.5969029162795,-6.18726937399527,-39.9055958805349));
#23949=CARTESIAN_POINT('Ctrl Pts',(27.599187113212,-6.19059093207268,-39.9050203362105));
#23950=CARTESIAN_POINT('Ctrl Pts',(27.6014189311488,-6.19395424178567,-39.9045087946084));
#23951=CARTESIAN_POINT('Ctrl Pts',(27.6041011626861,-6.19799631673864,-39.9038940164068));
#23952=CARTESIAN_POINT('Ctrl Pts',(27.6067075951069,-6.20209746439247,-39.9033697450797));
#23953=CARTESIAN_POINT('Ctrl Pts',(27.6092439514794,-6.20624978925052,-39.9029293953656));
#23954=CARTESIAN_POINT('Ctrl Pts',(27.6114632633054,-6.20988307350132,-39.9025440893657));
#23955=CARTESIAN_POINT('Ctrl Pts',(27.6136289069462,-6.21355555791224,-39.9022230232443));
#23956=CARTESIAN_POINT('Ctrl Pts',(27.6157440919799,-6.21726235805581,-39.9019615796143));
#23957=CARTESIAN_POINT('Ctrl Pts',(27.6219750132014,-6.22818186595202,-39.9011914178383));
#23958=CARTESIAN_POINT('Ctrl Pts',(27.6277878380593,-6.23942896207809,-39.9009317259755));
#23959=CARTESIAN_POINT('Ctrl Pts',(27.6332066390285,-6.25083884461389,-39.9010765586603));
#23960=CARTESIAN_POINT('Ctrl Pts',(27.6343122708321,-6.25316687420542,-39.9011061097775));
#23961=CARTESIAN_POINT('Ctrl Pts',(27.6354014986682,-6.2555018522693,-39.9011525316285));
#23962=CARTESIAN_POINT('Ctrl Pts',(27.6364745204553,-6.25784263179033,-39.9012149693086));
#23963=CARTESIAN_POINT('Ctrl Pts',(27.6426392228307,-6.27129082943956,-39.9015736849657));
#23964=CARTESIAN_POINT('Ctrl Pts',(27.6483061366112,-6.28489536287214,-39.9024185375791));
#23965=CARTESIAN_POINT('Ctrl Pts',(27.6535535090021,-6.2985815443386,-39.903595289237));
#23966=CARTESIAN_POINT('Ctrl Pts',(27.6574502388027,-6.30874498371449,-39.9044691519842));
#23967=CARTESIAN_POINT('Ctrl Pts',(27.6611206154207,-6.31897515336467,-39.9055604607672));
#23968=CARTESIAN_POINT('Ctrl Pts',(27.6645917831624,-6.32926010582614,-39.9068416997379));
#23969=CARTESIAN_POINT('Ctrl Pts',(27.670418092268,-6.34652326238773,-39.9089922423901));
#23970=CARTESIAN_POINT('Ctrl Pts',(27.675680571127,-6.36392973947355,-39.9116755677516));
#23971=CARTESIAN_POINT('Ctrl Pts',(27.6804674646178,-6.38139910649553,-39.9147853711119));
#23972=CARTESIAN_POINT('Ctrl Pts',(27.6857545369784,-6.40069383442647,-39.9182201154663));
#23973=CARTESIAN_POINT('Ctrl Pts',(27.690461568716,-6.42006561689591,-39.9221751468457));
#23974=CARTESIAN_POINT('Ctrl Pts',(27.6946812503251,-6.43945161623791,-39.9265477081944));
#23975=CARTESIAN_POINT('Ctrl Pts',(27.6991993449422,-6.46020858024372,-39.9312294941022));
#23976=CARTESIAN_POINT('Ctrl Pts',(27.7031587031065,-6.48098271066482,-39.9363903152504));
#23977=CARTESIAN_POINT('Ctrl Pts',(27.7066438148032,-6.50173650935267,-39.9419447801428));
#23978=CARTESIAN_POINT('Ctrl Pts',(27.7105819510236,-6.52518806368856,-39.9482212617253));
#23979=CARTESIAN_POINT('Ctrl Pts',(27.7139148163436,-6.54861499428405,-39.9550006703093));
#23980=CARTESIAN_POINT('Ctrl Pts',(27.7167256519374,-6.57199467982627,-39.9622052700919));
#23981=CARTESIAN_POINT('Ctrl Pts',(27.7176622649425,-6.57978514525988,-39.9646059518919));
#23982=CARTESIAN_POINT('Ctrl Pts',(27.7185406109312,-6.58757049922583,-39.9670541566905));
#23983=CARTESIAN_POINT('Ctrl Pts',(27.7193629006997,-6.59535009141639,-39.9695478224821));
#23984=CARTESIAN_POINT('Origin',(29.4643271522699,-12.8919045823054,-46.2591987469795));
#23985=CARTESIAN_POINT('Ctrl Pts',(30.3297286714007,-13.2959337131847,-46.7096495545262));
#23986=CARTESIAN_POINT('Ctrl Pts',(30.2800412871707,-13.2044045823055,-46.63278118881));
#23987=CARTESIAN_POINT('Ctrl Pts',(30.2097727145138,-13.2044045823055,-46.5240729034967));
#23988=CARTESIAN_POINT('Ctrl Pts',(30.2480070382537,-13.2959337183949,-46.7624740763582));
#23989=CARTESIAN_POINT('Ctrl Pts',(30.2237821295074,-13.2092798238967,-46.6749519433113));
#23990=CARTESIAN_POINT('Ctrl Pts',(30.1727791352342,-13.2044045823055,-46.5621348913443));
#23991=CARTESIAN_POINT('Ctrl Pts',(30.1557802945293,-13.2734166054796,-46.7949451596591));
#23992=CARTESIAN_POINT('Ctrl Pts',(30.1567362919807,-13.1931723515309,-46.698954204891));
#23993=CARTESIAN_POINT('Ctrl Pts',(30.1272434959976,-13.1931460297457,-46.5790211908226));
#23994=CARTESIAN_POINT('Ctrl Pts',(29.9810497702099,-13.1901047283842,-46.8078019025926));
#23995=CARTESIAN_POINT('Ctrl Pts',(30.0332579895645,-13.1260474868728,-46.6985032563468));
#23996=CARTESIAN_POINT('Ctrl Pts',(30.0334560808361,-13.1514900886123,-46.5650271793139));
#23997=CARTESIAN_POINT('Ctrl Pts',(29.9021671260579,-13.1321577745916,-46.7892918780939));
#23998=CARTESIAN_POINT('Ctrl Pts',(29.9785578442827,-13.0767072102091,-46.6749582903023));
#23999=CARTESIAN_POINT('Ctrl Pts',(29.9874804360701,-13.1225166214135,-46.535607917148));
#24000=CARTESIAN_POINT('Ctrl Pts',(29.7068169519706,-12.9456232578403,-46.6923959077902));
#24001=CARTESIAN_POINT('Ctrl Pts',(29.850736282044,-12.917759331099,-46.5682098335491));
#24002=CARTESIAN_POINT('Ctrl Pts',(29.8659898138072,-13.0292493378241,-46.4142407544751));
#24003=CARTESIAN_POINT('Ctrl Pts',(29.6248993528429,-12.802121823431,-46.5743671996335));
#24004=CARTESIAN_POINT('Ctrl Pts',(29.8160663686883,-12.7965826300651,-46.4467809431966));
#24005=CARTESIAN_POINT('Ctrl Pts',(29.8034597078097,-12.957479090352,-46.2897702608793));
#24006=CARTESIAN_POINT('Ctrl Pts',(29.5826474545624,-12.6709337131846,-46.4458225157374));
#24007=CARTESIAN_POINT('Ctrl Pts',(29.8183400962187,-12.7034528674627,-46.3348964586614));
#24008=CARTESIAN_POINT('Ctrl Pts',(29.7611081292079,-12.8919045823054,-46.1613350574533));
#24009=CARTESIAN_POINT('Origin',(30.2097727145137,-13.5169045823054,-46.5240729034966));
#24010=CARTESIAN_POINT('Ctrl Pts',(29.7611081292079,-12.8919045823054,-46.1613350574533));
#24011=CARTESIAN_POINT('Ctrl Pts',(29.7689446056648,-12.9040380872524,-46.1850999200892));
#24012=CARTESIAN_POINT('Ctrl Pts',(29.7774029552135,-12.9162817766924,-46.2085325222876));
#24013=CARTESIAN_POINT('Ctrl Pts',(29.7865325971137,-12.9286427508496,-46.2316011837146));
#24014=CARTESIAN_POINT('Ctrl Pts',(29.7946239763792,-12.9395979811959,-46.2520463765046));
#24015=CARTESIAN_POINT('Ctrl Pts',(29.803243400554,-12.9506462200838,-46.2722072543535));
#24016=CARTESIAN_POINT('Ctrl Pts',(29.8124568466866,-12.9617976021851,-46.2920436345019));
#24017=CARTESIAN_POINT('Ctrl Pts',(29.820976079617,-12.972108751808,-46.3103853863879));
#24018=CARTESIAN_POINT('Ctrl Pts',(29.8300034908812,-12.9825085406178,-46.3284505844458));
#24019=CARTESIAN_POINT('Ctrl Pts',(29.8396134313692,-12.9930011868745,-46.3461752269231));
#24020=CARTESIAN_POINT('Ctrl Pts',(29.8486149610157,-13.0028295376813,-46.3627777121238));
#24021=CARTESIAN_POINT('Ctrl Pts',(29.8581277574155,-13.0127396637205,-46.3790820278025));
#24022=CARTESIAN_POINT('Ctrl Pts',(29.8682301303537,-13.0227264646583,-46.3949958588203));
#24023=CARTESIAN_POINT('Ctrl Pts',(29.8775297079321,-13.031919654283,-46.4096450810401));
#24024=CARTESIAN_POINT('Ctrl Pts',(29.8873290303633,-13.0411779829383,-46.4239636984746));
#24025=CARTESIAN_POINT('Ctrl Pts',(29.8977020867377,-13.0504868885806,-46.4378390387971));
#24026=CARTESIAN_POINT('Ctrl Pts',(29.9030617551183,-13.0552967194953,-46.4450083069581));
#24027=CARTESIAN_POINT('Ctrl Pts',(29.9085747980936,-13.0601198606037,-46.4520585243));
#24028=CARTESIAN_POINT('Ctrl Pts',(29.9142527689337,-13.0649528255951,-46.4589689296633));
#24029=CARTESIAN_POINT('Ctrl Pts',(29.9228757513932,-13.0722925202715,-46.4694635774722));
#24030=CARTESIAN_POINT('Ctrl Pts',(29.9318251137018,-13.0796093213738,-46.4795773572471));
#24031=CARTESIAN_POINT('Ctrl Pts',(29.9411925883594,-13.086931462929,-46.4892853924893));
#24032=CARTESIAN_POINT('Ctrl Pts',(29.9431045819531,-13.0884259839454,-46.4912668978437));
#24033=CARTESIAN_POINT('Ctrl Pts',(29.9450340495387,-13.0899206854315,-46.4932313419366));
#24034=CARTESIAN_POINT('Ctrl Pts',(29.9469818564132,-13.0914157380931,-46.4951782578757));
#24035=CARTESIAN_POINT('Ctrl Pts',(29.9549256601176,-13.0975130596637,-46.5031184280495));
#24036=CARTESIAN_POINT('Ctrl Pts',(29.9632075915649,-13.1036283475447,-46.5107647600667));
#24037=CARTESIAN_POINT('Ctrl Pts',(29.9718588309488,-13.109735216012,-46.518012937061));
#24038=CARTESIAN_POINT('Ctrl Pts',(29.980031801798,-13.11550447701,-46.5248604113539));
#24039=CARTESIAN_POINT('Ctrl Pts',(29.9885346137173,-13.1212664690673,-46.5313529626109));
#24040=CARTESIAN_POINT('Ctrl Pts',(29.9973930117943,-13.1269828032032,-46.5373614305493));
#24041=CARTESIAN_POINT('Ctrl Pts',(30.0055746904732,-13.1322624495583,-46.5429108937362));
#24042=CARTESIAN_POINT('Ctrl Pts',(30.0140598659004,-13.1375032622592,-46.548047569981));
#24043=CARTESIAN_POINT('Ctrl Pts',(30.0228656315125,-13.1426584957574,-46.5526298236939));
#24044=CARTESIAN_POINT('Ctrl Pts',(30.0295253896781,-13.1465573740489,-46.5560953601305));
#24045=CARTESIAN_POINT('Ctrl Pts',(30.0363684855418,-13.1504070236379,-46.5592430884801));
#24046=CARTESIAN_POINT('Ctrl Pts',(30.0434000451071,-13.1541794056116,-46.5619934529432));
#24047=CARTESIAN_POINT('Ctrl Pts',(30.0550572816468,-13.1604334305654,-46.5665531311794));
#24048=CARTESIAN_POINT('Ctrl Pts',(30.0674459465525,-13.1665823184279,-46.570124885838));
#24049=CARTESIAN_POINT('Ctrl Pts',(30.0803549315343,-13.1723138052614,-46.572067420129));
#24050=CARTESIAN_POINT('Ctrl Pts',(30.089601156449,-13.1764190557078,-46.5734587850569));
#24051=CARTESIAN_POINT('Ctrl Pts',(30.0990247132506,-13.180252986557,-46.5739543522569));
#24052=CARTESIAN_POINT('Ctrl Pts',(30.1084980236264,-13.1837286680714,-46.5734464756373));
#24053=CARTESIAN_POINT('Ctrl Pts',(30.115560834798,-13.186319956782,-46.573067829048));
#24054=CARTESIAN_POINT('Ctrl Pts',(30.122650932996,-13.1887123032027,-46.5721323870867));
#24055=CARTESIAN_POINT('Ctrl Pts',(30.1297115805048,-13.1908748315003,-46.5706133212394));
#24056=CARTESIAN_POINT('Ctrl Pts',(30.1379679083212,-13.1934035716073,-46.5688370102715));
#24057=CARTESIAN_POINT('Ctrl Pts',(30.1461053622757,-13.1955933528871,-46.5662741485632));
#24058=CARTESIAN_POINT('Ctrl Pts',(30.1540188210239,-13.1974205800258,-46.5629748938067));
#24059=CARTESIAN_POINT('Ctrl Pts',(30.1619718333917,-13.1992569401429,-46.5596591484774));
#24060=CARTESIAN_POINT('Ctrl Pts',(30.1696981454544,-13.2007270768473,-46.5555998526813));
#24061=CARTESIAN_POINT('Ctrl Pts',(30.1771066956215,-13.2018302796858,-46.5508928619014));
#24062=CARTESIAN_POINT('Ctrl Pts',(30.1846349929034,-13.2029513139965,-46.5461097903023));
#24063=CARTESIAN_POINT('Ctrl Pts',(30.1918347533013,-13.2036934504427,-46.5406581808445));
#24064=CARTESIAN_POINT('Ctrl Pts',(30.1986333530818,-13.2040802847478,-46.5346813319021));
#24065=CARTESIAN_POINT('Ctrl Pts',(30.2024773666742,-13.204299005716,-46.531301946541));
#24066=CARTESIAN_POINT('Ctrl Pts',(30.2061935878781,-13.2044045823055,-46.5277553985989));
#24067=CARTESIAN_POINT('Ctrl Pts',(30.2097727145138,-13.2044045823055,-46.5240729034967));
#24068=CARTESIAN_POINT('Ctrl Pts',(27.4605785366061,-6.10843371318469,-39.9870540284924));
#24069=CARTESIAN_POINT('Ctrl Pts',(27.4089435087152,-6.01690458230549,-39.9114801858336));
#24070=CARTESIAN_POINT('Ctrl Pts',(27.4089435087152,-5.8874628440639,-39.9114801858336));
#24071=CARTESIAN_POINT('Ctrl Pts',(27.4926254958792,-6.10275018345573,-39.9582748359069));
#24072=CARTESIAN_POINT('Ctrl Pts',(27.457094436975,-6.01222811249993,-39.8785815735222));
#24073=CARTESIAN_POINT('Ctrl Pts',(27.4761172860278,-5.88746285448466,-39.8655844136585));
#24074=CARTESIAN_POINT('Ctrl Pts',(27.5262766366667,-6.11419577460873,-39.9349635041551));
#24075=CARTESIAN_POINT('Ctrl Pts',(27.5056815629761,-6.02882146164738,-39.8452613916108));
#24076=CARTESIAN_POINT('Ctrl Pts',(27.5432762945934,-5.91065570868296,-39.8194267690275));
#24077=CARTESIAN_POINT('Ctrl Pts',(27.5869602346596,-6.16774318631796,-39.9061265671302));
#24078=CARTESIAN_POINT('Ctrl Pts',(27.583668943987,-6.09780352750744,-39.7916619276919));
#24079=CARTESIAN_POINT('Ctrl Pts',(27.6568986769456,-5.99623773973461,-39.7409950094831));
#24080=CARTESIAN_POINT('Ctrl Pts',(27.6142659702345,-6.20950986590629,-39.9002511491957));
#24081=CARTESIAN_POINT('Ctrl Pts',(27.6140401210967,-6.15046547604275,-39.7707310218534));
#24082=CARTESIAN_POINT('Ctrl Pts',(27.7041874632732,-6.05824038173977,-39.7081745064884));
#24083=CARTESIAN_POINT('Ctrl Pts',(27.6808991139987,-6.3546301407073,-39.9034964109337));
#24084=CARTESIAN_POINT('Ctrl Pts',(27.6737052370323,-6.32861804115438,-39.7296612449018));
#24085=CARTESIAN_POINT('Ctrl Pts',(27.8101683547685,-6.26685602924678,-39.6344682377825));
#24086=CARTESIAN_POINT('Ctrl Pts',(27.7067660427821,-6.47617237885483,-39.9313466488163));
#24087=CARTESIAN_POINT('Ctrl Pts',(27.6709846760168,-6.47276044373897,-39.7316943091956));
#24088=CARTESIAN_POINT('Ctrl Pts',(27.8370886911753,-6.43425950785912,-39.61556810409));
#24089=CARTESIAN_POINT('Ctrl Pts',(27.7193629372986,-6.59535043767467,-39.9695479334715));
#24090=CARTESIAN_POINT('Ctrl Pts',(27.6465610575461,-6.59535043767467,-39.7487692861459));
#24091=CARTESIAN_POINT('Ctrl Pts',(27.83708867484,-6.59535043767467,-39.6155681155102));
#24092=CARTESIAN_POINT('Origin',(27.5852365212336,-5.88746284406389,-40.1695054243999));
#24093=CARTESIAN_POINT('Origin',(28.0161439142367,-6.59535043767467,-39.8716842439453));
#24094=CARTESIAN_POINT('Origin',(0.0835265683620477,-13.5169045823054,0.0824317919394229));
#24095=CARTESIAN_POINT('Origin',(31.5582959274376,-13.5169045823054,-45.624196617704));
#24096=CARTESIAN_POINT('Origin',(13.3939389642122,-12.8919045823054,4.47154756213422));
#24097=CARTESIAN_POINT('Origin',(28.0161439142367,-12.8919045823054,-39.8716842439453));
#24098=CARTESIAN_POINT('Origin',(28.0161439142367,-14.7669045823054,-39.8716842439453));
#24099=CARTESIAN_POINT('Origin',(28.0161439142367,-12.8919045823054,-39.8716842439453));
#24100=CARTESIAN_POINT('Origin',(0.0835265683620477,-5.88746284406389,0.0824317919394229));
#24101=CARTESIAN_POINT('Ctrl Pts',(30.5401339447129,-14.9741386829693,-48.3550682080606));
#24102=CARTESIAN_POINT('Ctrl Pts',(30.6141174651452,-14.8357920829899,-48.3550682080606));
#24103=CARTESIAN_POINT('Ctrl Pts',(30.6583146466958,-14.7531448966913,-48.229253285411));
#24104=CARTESIAN_POINT('Ctrl Pts',(28.492829280589,-13.8793029116944,-48.3550682080606));
#24105=CARTESIAN_POINT('Ctrl Pts',(28.5700753356058,-13.7458678866727,-48.3550682080606));
#24106=CARTESIAN_POINT('Ctrl Pts',(28.6053355619279,-13.6583075326732,-48.232843582883));
#24107=CARTESIAN_POINT('Ctrl Pts',(26.4097780451804,-12.8434482903031,-48.3550682080606));
#24108=CARTESIAN_POINT('Ctrl Pts',(26.4826847058204,-12.7103751542466,-48.3550682080606));
#24109=CARTESIAN_POINT('Ctrl Pts',(26.5160221214703,-12.6224528665269,-48.2364507688974));
#24110=CARTESIAN_POINT('Ctrl Pts',(23.213550958804,-11.4077451872907,-48.3550682080606));
#24111=CARTESIAN_POINT('Ctrl Pts',(23.2738757441258,-11.2735898053145,-48.3550682080606));
#24112=CARTESIAN_POINT('Ctrl Pts',(23.3093293343021,-11.1867499400307,-48.2417141569431));
#24113=CARTESIAN_POINT('Ctrl Pts',(22.1361415983178,-10.9489604127289,-48.3550682080606));
#24114=CARTESIAN_POINT('Ctrl Pts',(22.1939919164413,-10.8151504288131,-48.3550682080606));
#24115=CARTESIAN_POINT('Ctrl Pts',(22.2282518962435,-10.7279650272959,-48.2434431037797));
#24116=CARTESIAN_POINT('Ctrl Pts',(19.9534411816293,-10.0773547210516,-48.3550682080606));
#24117=CARTESIAN_POINT('Ctrl Pts',(20.0062495694822,-9.94441815656816,-48.3550682080606));
#24118=CARTESIAN_POINT('Ctrl Pts',(20.0378275778654,-9.85635900888071,-48.2468078474917));
#24119=CARTESIAN_POINT('Ctrl Pts',(18.8490684843153,-9.66512413195019,-48.3550682080606));
#24120=CARTESIAN_POINT('Ctrl Pts',(18.8991406427071,-9.5324655645878,-48.3550682080606));
#24121=CARTESIAN_POINT('Ctrl Pts',(18.9294012091805,-9.44412830208801,-48.2484415699068));
#24122=CARTESIAN_POINT('Ctrl Pts',(13.3105934045374,-7.75733423685904,-48.3550682080606));
#24123=CARTESIAN_POINT('Ctrl Pts',(13.3719143129995,-7.63508483860106,-48.3550682080606));
#24124=CARTESIAN_POINT('Ctrl Pts',(13.3698756070365,-7.53633525782184,-48.2561639741704));
#24125=CARTESIAN_POINT('Ctrl Pts',(8.78203978180937,-6.70462823795841,-48.3550682080606));
#24126=CARTESIAN_POINT('Ctrl Pts',(8.81311496927653,-6.57519149763133,-48.3550682080606));
#24127=CARTESIAN_POINT('Ctrl Pts',(8.82176014815773,-6.48363668556399,-48.2609639163927));
#24128=CARTESIAN_POINT('Ctrl Pts',(4.11624754821277,-6.31501530004509,-48.3550682080606));
#24129=CARTESIAN_POINT('Ctrl Pts',(4.12707394707883,-6.18536424665212,-48.3550682080606));
#24130=CARTESIAN_POINT('Ctrl Pts',(4.13470171397579,-6.09401826675045,-48.2627408790281));
#24131=CARTESIAN_POINT('Ctrl Pts',(30.5121796307589,-14.6753754514262,-48.2295435588551));
#24132=CARTESIAN_POINT('Ctrl Pts',(30.4851371197009,-14.6690808662602,-48.2391368684286));
#24133=CARTESIAN_POINT('Ctrl Pts',(30.4577982704948,-14.6627210376773,-48.2478016524146));
#24134=CARTESIAN_POINT('Ctrl Pts',(30.4302713467175,-14.6563210590023,-48.2557044117279));
#24135=CARTESIAN_POINT('Ctrl Pts',(30.4010697645148,-14.6495317241356,-48.2640879520604));
#24136=CARTESIAN_POINT('Ctrl Pts',(30.3716560750817,-14.6426970987334,-48.2716137426758));
#24137=CARTESIAN_POINT('Ctrl Pts',(30.3421145822481,-14.6358367158202,-48.2784438176708));
#24138=CARTESIAN_POINT('Ctrl Pts',(30.3092090732797,-14.6281951117635,-48.2860516625169));
#24139=CARTESIAN_POINT('Ctrl Pts',(30.2761445940227,-14.6205214533656,-48.292796328517));
#24140=CARTESIAN_POINT('Ctrl Pts',(30.2429899455176,-14.6128317093194,-48.2988585238745));
#24141=CARTESIAN_POINT('Ctrl Pts',(30.2062238617915,-14.6043043447963,-48.3055810557705));
#24142=CARTESIAN_POINT('Ctrl Pts',(30.1693457982678,-14.5957569385231,-48.3114640731145));
#24143=CARTESIAN_POINT('Ctrl Pts',(30.1324060630064,-14.587201298653,-48.3167055873355));
#24144=CARTESIAN_POINT('Ctrl Pts',(30.1041689095605,-14.5806612703033,-48.3207122603747));
#24145=CARTESIAN_POINT('Ctrl Pts',(30.0758945614216,-14.5741161640292,-48.3243429309501));
#24146=CARTESIAN_POINT('Ctrl Pts',(30.0475982203807,-14.5675696486119,-48.3276721877859));
#24147=CARTESIAN_POINT('Ctrl Pts',(30.0447146594573,-14.5669025208015,-48.3280114583263));
#24148=CARTESIAN_POINT('Ctrl Pts',(30.0418299490014,-14.5662351623918,-48.3283473948448));
#24149=CARTESIAN_POINT('Ctrl Pts',(30.0389439896954,-14.5655675503514,-48.3286800185805));
#24150=CARTESIAN_POINT('Ctrl Pts',(29.9436377737461,-14.5435202618948,-48.3396646189221));
#24151=CARTESIAN_POINT('Ctrl Pts',(29.8480280991363,-14.5214458554098,-48.3469207097561));
#24152=CARTESIAN_POINT('Ctrl Pts',(29.7521618054431,-14.4993564117025,-48.3509992918687));
#24153=CARTESIAN_POINT('Ctrl Pts',(29.6871620963625,-14.4843792246285,-48.3537646710292));
#24154=CARTESIAN_POINT('Ctrl Pts',(29.622044134505,-14.4693950374107,-48.3550680832409));
#24155=CARTESIAN_POINT('Ctrl Pts',(29.5568194237311,-14.454406734056,-48.3550682080516));
#24156=CARTESIAN_POINT('Ctrl Pts',(-30.4912134104872,-14.7531486984911,
-48.2292882301095));
#24157=CARTESIAN_POINT('Ctrl Pts',(-30.4470156710373,-14.8357969973015,
-48.3550682080606));
#24158=CARTESIAN_POINT('Ctrl Pts',(-30.373045062923,-14.9741195676119,-48.3550682080606));
#24159=CARTESIAN_POINT('Ctrl Pts',(-28.4387348231413,-13.6585793127108,
-48.2328767825385));
#24160=CARTESIAN_POINT('Ctrl Pts',(-28.4034671513468,-13.7461362596467,
-48.3550682080606));
#24161=CARTESIAN_POINT('Ctrl Pts',(-28.3262370698434,-13.8795503180506,
-48.3550682080606));
#24162=CARTESIAN_POINT('Ctrl Pts',(-26.3501996831797,-12.6231097579334,
-48.2364817168271));
#24163=CARTESIAN_POINT('Ctrl Pts',(-26.3168499742945,-12.7110265271844,
-48.3550682080606));
#24164=CARTESIAN_POINT('Ctrl Pts',(-26.243961294676,-12.8440806269501,-48.3550682080606));
#24165=CARTESIAN_POINT('Ctrl Pts',(-23.145314529641,-11.1881005852606,-48.2417410418288));
#24166=CARTESIAN_POINT('Ctrl Pts',(-23.1098551901269,-11.2749369501014,
-48.3550682080606));
#24167=CARTESIAN_POINT('Ctrl Pts',(-23.0495359459671,-11.4090714544335,
-48.3550682080606));
#24168=CARTESIAN_POINT('Ctrl Pts',(-22.0649478906704,-10.7295656511252,
-48.2434685231326));
#24169=CARTESIAN_POINT('Ctrl Pts',(-22.0306807474001,-10.8167469967119,
-48.3550682080606));
#24170=CARTESIAN_POINT('Ctrl Pts',(-21.9728343771648,-10.9505365201866,
-48.3550682080606));
#24171=CARTESIAN_POINT('Ctrl Pts',(-19.8762142444861,-9.85847188921458,
-48.246830209952));
#24172=CARTESIAN_POINT('Ctrl Pts',(-19.844626683273,-9.94652588376056,-48.3550682080606));
#24173=CARTESIAN_POINT('Ctrl Pts',(-19.7918171438271,-10.0794427583948,
-48.3550682080606));
#24174=CARTESIAN_POINT('Ctrl Pts',(-18.7666798697007,-9.44570717935272,
-48.2484654765336));
#24175=CARTESIAN_POINT('Ctrl Pts',(-18.7364165373226,-9.53404162556794,
-48.3550682080606));
#24176=CARTESIAN_POINT('Ctrl Pts',(-18.6863395540866,-9.66667804843006,
-48.3550682080606));
#24177=CARTESIAN_POINT('Ctrl Pts',(-13.2023926152288,-7.53595817693426,
-48.2561934845101));
#24178=CARTESIAN_POINT('Ctrl Pts',(-13.2044686097622,-7.63471881015605,
-48.3550682080606));
#24179=CARTESIAN_POINT('Ctrl Pts',(-13.1431103220519,-7.7569290462289,-48.3550682080606));
#24180=CARTESIAN_POINT('Ctrl Pts',(-8.6526970032033,-6.4835029201157,-48.2609915525571));
#24181=CARTESIAN_POINT('Ctrl Pts',(-8.64404384437381,-6.57505277908091,
-48.3550682080606));
#24182=CARTESIAN_POINT('Ctrl Pts',(-8.61298834195424,-6.70446830382948,
-48.3550682080606));
#24183=CARTESIAN_POINT('Ctrl Pts',(-3.96771901147946,-6.09405046754031,
-48.2627672936114));
#24184=CARTESIAN_POINT('Ctrl Pts',(-3.96009147509235,-6.18539206100947,
-48.3550682080606));
#24185=CARTESIAN_POINT('Ctrl Pts',(-3.94926670206929,-6.31502133666111,
-48.3550682080606));
#24186=CARTESIAN_POINT('Ctrl Pts',(-29.3897661934246,-14.4544067125512,
-48.3550682080518));
#24187=CARTESIAN_POINT('Ctrl Pts',(-29.4762602452486,-14.474282601133,-48.3550680438326));
#24188=CARTESIAN_POINT('Ctrl Pts',(-29.5625289546745,-14.4941426280479,
-48.3527732539111));
#24189=CARTESIAN_POINT('Ctrl Pts',(-29.6485434749624,-14.5139794995301,
-48.3478250805349));
#24190=CARTESIAN_POINT('Ctrl Pts',(-29.7231251977381,-14.5311797122927,
-48.3435346038368));
#24191=CARTESIAN_POINT('Ctrl Pts',(-29.7975156566768,-14.548362486812,-48.3372488058751));
#24192=CARTESIAN_POINT('Ctrl Pts',(-29.8716853835464,-14.5655203189317,
-48.3287039250806));
#24193=CARTESIAN_POINT('Ctrl Pts',(-29.8750081603114,-14.566288983565,-48.3283211175314));
#24194=CARTESIAN_POINT('Ctrl Pts',(-29.8783295511836,-14.5670573738946,
-48.3279338770541));
#24195=CARTESIAN_POINT('Ctrl Pts',(-29.8816496610406,-14.5678255143184,
-48.3275421732212));
#24196=CARTESIAN_POINT('Ctrl Pts',(-29.921364211269,-14.5770138703543,-48.3228566832171));
#24197=CARTESIAN_POINT('Ctrl Pts',(-29.961084755409,-14.5862107044419,-48.3175899444853));
#24198=CARTESIAN_POINT('Ctrl Pts',(-30.0007382034786,-14.5953989044396,
-48.3115102233366));
#24199=CARTESIAN_POINT('Ctrl Pts',(-30.0367071665706,-14.6037333631736,
-48.3059954124878));
#24200=CARTESIAN_POINT('Ctrl Pts',(-30.0726218123948,-14.6120609299876,
-48.2998121059003));
#24201=CARTESIAN_POINT('Ctrl Pts',(-30.108407457618,-14.6203642532744,-48.2927569262129));
#24202=CARTESIAN_POINT('Ctrl Pts',(-30.1417601067399,-14.6281030498338,
-48.2861814144082));
#24203=CARTESIAN_POINT('Ctrl Pts',(-30.175001269215,-14.6358209223577,-48.2788488663937));
#24204=CARTESIAN_POINT('Ctrl Pts',(-30.2080423754229,-14.6434973280408,
-48.2705618313201));
#24205=CARTESIAN_POINT('Ctrl Pts',(-30.2384940192198,-14.6505721266275,
-48.2629242589397));
#24206=CARTESIAN_POINT('Ctrl Pts',(-30.2687760027118,-14.6576117669138,
-48.2544760489632));
#24207=CARTESIAN_POINT('Ctrl Pts',(-30.2987888272563,-14.6645931621405,
-48.2450311446474));
#24208=CARTESIAN_POINT('Ctrl Pts',(-30.3143131643305,-14.6682043361767,
-48.2401457038248));
#24209=CARTESIAN_POINT('Ctrl Pts',(-30.3297649549302,-14.6717998028493,
-48.2349930527964));
#24210=CARTESIAN_POINT('Ctrl Pts',(-30.3451264940351,-14.6753754514261,
-48.2295435588555));
#24211=CARTESIAN_POINT('Ctrl Pts',(-4.13722355950312,-6.10843371319295,
-48.2627017454154));
#24212=CARTESIAN_POINT('Ctrl Pts',(-4.13366090217496,-6.10843410331483,
-48.2630131843227));
#24213=CARTESIAN_POINT('Ctrl Pts',(-4.13160726137051,-6.12223873054887,
-48.2774222205278));
#24214=CARTESIAN_POINT('Ctrl Pts',(-4.12818752330401,-6.16064820739695,
-48.306533073772));
#24215=CARTESIAN_POINT('Ctrl Pts',(-4.12682927344009,-6.1854892637356,-48.3210576919346));
#24216=CARTESIAN_POINT('Ctrl Pts',(-4.1255125788106,-6.20946968450871,-48.331053858379));
#24217=CARTESIAN_POINT('Origin',(-44.291473431638,-14.4544045823054,-48.6675682080606));
#24218=CARTESIAN_POINT('Origin',(-29.3897569232175,-14.4544045823054,-48.6675682080606));
#24219=CARTESIAN_POINT('Origin',(29.5568100599416,-14.4544045823054,-48.6675682080606));
#24220=CARTESIAN_POINT('Ctrl Pts',(29.5568100599416,-14.7669045823054,-48.6675682080606));
#24221=CARTESIAN_POINT('Ctrl Pts',(29.5568100599416,-14.7669045823054,-48.3550682080606));
#24222=CARTESIAN_POINT('Ctrl Pts',(29.5568100599416,-14.4544045823054,-48.3550682080606));
#24223=CARTESIAN_POINT('Ctrl Pts',(29.7424051118639,-14.7669045823054,-48.6675682065036));
#24224=CARTESIAN_POINT('Ctrl Pts',(29.7130820249225,-14.7669045823054,-48.3909786805563));
#24225=CARTESIAN_POINT('Ctrl Pts',(29.7225178757419,-14.4924833818637,-48.3550682080606));
#24226=CARTESIAN_POINT('Ctrl Pts',(29.9261186112019,-14.7669045823054,-48.65073395611));
#24227=CARTESIAN_POINT('Ctrl Pts',(29.885222340593,-14.7669045823054,-48.4094018403383));
#24228=CARTESIAN_POINT('Ctrl Pts',(29.88629202078,-14.5302495546685,-48.3466510766381));
#24229=CARTESIAN_POINT('Ctrl Pts',(30.2885287859832,-14.7669045823054,-48.5748131378707));
#24230=CARTESIAN_POINT('Ctrl Pts',(30.2267587801975,-14.7669045823054,-48.3980269109194));
#24231=CARTESIAN_POINT('Ctrl Pts',(30.2089038710123,-14.6048828507185,-48.3086906784128));
#24232=CARTESIAN_POINT('Ctrl Pts',(30.4709665311741,-14.7669045823054,-48.5166482630913));
#24233=CARTESIAN_POINT('Ctrl Pts',(30.4029958016937,-14.7669045823061,-48.373227132016));
#24234=CARTESIAN_POINT('Ctrl Pts',(30.3706213015912,-14.6424253938168,-48.279761206536));
#24235=CARTESIAN_POINT('Ctrl Pts',(30.6299435607004,-14.7669045823054,-48.4165189096496));
#24236=CARTESIAN_POINT('Ctrl Pts',(30.560959047699,-14.7669045823054,-48.3069912849837));
#24237=CARTESIAN_POINT('Ctrl Pts',(30.5121796307589,-14.6753754514262,-48.2295435588551));
#24238=CARTESIAN_POINT('Origin',(30.6299435607004,-14.4544045823054,-48.4165189096496));
#24239=CARTESIAN_POINT('Origin',(31.5582959274376,-13.5169045823054,-45.624196617704));
#24240=CARTESIAN_POINT('Origin',(31.5582959274376,-13.5169045823054,-45.624196617704));
#24241=CARTESIAN_POINT('Origin',(31.5582959274376,-13.5169045823054,-45.624196617704));
#24242=CARTESIAN_POINT('Ctrl Pts',(38.7441826758856,-12.5761796977905,-39.0327738807645));
#24243=CARTESIAN_POINT('Ctrl Pts',(38.3485196429793,-12.4966730216635,-39.3120862649867));
#24244=CARTESIAN_POINT('Ctrl Pts',(38.2952452485764,-12.8445798972111,-38.9722437240839));
#24245=CARTESIAN_POINT('Ctrl Pts',(38.8327231904435,-12.7679658886682,-39.2148934728689));
#24246=CARTESIAN_POINT('Ctrl Pts',(38.4835044759548,-12.6138199372454,-39.3425594757914));
#24247=CARTESIAN_POINT('Ctrl Pts',(38.3710663661159,-12.9405865508053,-39.1587051318414));
#24248=CARTESIAN_POINT('Ctrl Pts',(38.8505926378097,-12.947799979713,-39.4500192046968));
#24249=CARTESIAN_POINT('Ctrl Pts',(38.5841849711601,-12.8036087634365,-39.5090831497147));
#24250=CARTESIAN_POINT('Ctrl Pts',(38.4159465000987,-13.0304169137549,-39.3844915465615));
#24251=CARTESIAN_POINT('Ctrl Pts',(38.7807028232922,-13.1418528526575,-39.7888775131573));
#24252=CARTESIAN_POINT('Ctrl Pts',(38.5946371067972,-13.0167291165572,-39.7950416036854));
#24253=CARTESIAN_POINT('Ctrl Pts',(38.4282877533204,-13.1274080636027,-39.6957098010915));
#24254=CARTESIAN_POINT('Ctrl Pts',(38.7479587227422,-13.1924895597094,-39.8911589997829));
#24255=CARTESIAN_POINT('Ctrl Pts',(38.5857601078203,-13.0721360087908,-39.8805420027495));
#24256=CARTESIAN_POINT('Ctrl Pts',(38.4256296765948,-13.1527155106485,-39.7878990938785));
#24257=CARTESIAN_POINT('Ctrl Pts',(38.6303501830799,-13.2848578326186,-40.1327590777328));
#24258=CARTESIAN_POINT('Ctrl Pts',(38.5262233426554,-13.1766908654362,-40.0825873356879));
#24259=CARTESIAN_POINT('Ctrl Pts',(38.397287636017,-13.1988763557092,-39.9996108902579));
#24260=CARTESIAN_POINT('Ctrl Pts',(38.5301204732258,-13.3151873395653,-40.2706150387653));
#24261=CARTESIAN_POINT('Ctrl Pts',(38.4618886750501,-13.2202535090901,-40.2043352524455));
#24262=CARTESIAN_POINT('Ctrl Pts',(38.3631207749851,-13.2140287022009,-40.1151439306369));
#24263=CARTESIAN_POINT('Ctrl Pts',(38.3844295904368,-13.2823030560806,-40.3632398375542));
#24264=CARTESIAN_POINT('Ctrl Pts',(38.3547920390607,-13.2034487358314,-40.2827072051125));
#24265=CARTESIAN_POINT('Ctrl Pts',(38.2967798358718,-13.1975864244366,-40.1818251675064));
#24266=CARTESIAN_POINT('Origin',(38.3461436957037,-13.5169045823054,-40.1137013224621));
#24267=CARTESIAN_POINT('Origin',(38.6273587102144,-12.8919045823054,-38.970752044692));
#24268=CARTESIAN_POINT('Ctrl Pts',(38.3461436957037,-13.2044045823054,-40.1137013224621));
#24269=CARTESIAN_POINT('Ctrl Pts',(38.3527349505192,-13.2044045823054,-40.1014642897562));
#24270=CARTESIAN_POINT('Ctrl Pts',(38.3586506936916,-13.2039200465849,-40.0889643259692));
#24271=CARTESIAN_POINT('Ctrl Pts',(38.3639906945034,-13.2030865921358,-40.07627240884));
#24272=CARTESIAN_POINT('Ctrl Pts',(38.3695508553509,-13.2022187756393,-40.0630572234514));
#24273=CARTESIAN_POINT('Ctrl Pts',(38.3744876033222,-13.2009724747263,-40.0496336726696));
#24274=CARTESIAN_POINT('Ctrl Pts',(38.3789315603931,-13.199446062585,-40.0360759455575));
#24275=CARTESIAN_POINT('Ctrl Pts',(38.3836173393714,-13.1978365893588,-40.0217804625719));
#24276=CARTESIAN_POINT('Ctrl Pts',(38.3877559277068,-13.1959155151287,-40.0073355755147));
#24277=CARTESIAN_POINT('Ctrl Pts',(38.3915083691255,-13.1937414656795,-39.9928256451289));
#24278=CARTESIAN_POINT('Ctrl Pts',(38.3923482654788,-13.1932548554968,-39.9895779361689));
#24279=CARTESIAN_POINT('Ctrl Pts',(38.3931688235478,-13.1927553638524,-39.9863269663215));
#24280=CARTESIAN_POINT('Ctrl Pts',(38.3939718492354,-13.1922433006301,-39.9830736815322));
#24281=CARTESIAN_POINT('Ctrl Pts',(38.3985388456595,-13.1893310763501,-39.96457148387));
#24282=CARTESIAN_POINT('Ctrl Pts',(38.4024620375392,-13.1860397456251,-39.9460233830121));
#24283=CARTESIAN_POINT('Ctrl Pts',(38.4058467955392,-13.1824628010599,-39.9274371587315));
#24284=CARTESIAN_POINT('Ctrl Pts',(38.4094080083047,-13.1786993826273,-39.9078819943239));
#24285=CARTESIAN_POINT('Ctrl Pts',(38.412373936463,-13.1746195596086,-39.8882843799791));
#24286=CARTESIAN_POINT('Ctrl Pts',(38.4148685466348,-13.1702746943006,-39.8686529670812));
#24287=CARTESIAN_POINT('Ctrl Pts',(38.4157454344845,-13.1687474177584,-39.861752270677));
#24288=CARTESIAN_POINT('Ctrl Pts',(38.416564043558,-13.1671869117775,-39.8548474119525));
#24289=CARTESIAN_POINT('Ctrl Pts',(38.4173295455032,-13.1655939279677,-39.8479388367875));
#24290=CARTESIAN_POINT('Ctrl Pts',(38.4202095417174,-13.1596007526788,-39.8219471715217));
#24291=CARTESIAN_POINT('Ctrl Pts',(38.4223252371397,-13.1531817886309,-39.796040194814));
#24292=CARTESIAN_POINT('Ctrl Pts',(38.423772695553,-13.1464435609449,-39.770219526676));
#24293=CARTESIAN_POINT('Ctrl Pts',(38.4252700922353,-13.1394728599642,-39.743508028475));
#24294=CARTESIAN_POINT('Ctrl Pts',(38.4260531947707,-13.1321600180536,-39.7168886175193));
#24295=CARTESIAN_POINT('Ctrl Pts',(38.4262243221591,-13.1245659628583,-39.6903644177419));
#24296=CARTESIAN_POINT('Ctrl Pts',(38.4264026290774,-13.1166533043878,-39.6627274137112));
#24297=CARTESIAN_POINT('Ctrl Pts',(38.4259173417366,-13.1084348255796,-39.6351935110303));
#24298=CARTESIAN_POINT('Ctrl Pts',(38.4248669041159,-13.0999262547332,-39.6077719485728));
#24299=CARTESIAN_POINT('Ctrl Pts',(38.4245074060405,-13.0970143113834,-39.5983872895176));
#24300=CARTESIAN_POINT('Ctrl Pts',(38.4240815153899,-13.094067983939,-39.5890158539865));
#24301=CARTESIAN_POINT('Ctrl Pts',(38.4235924932819,-13.0910867263844,-39.5796582381904));
#24302=CARTESIAN_POINT('Ctrl Pts',(38.4217908661768,-13.0801033488869,-39.5451834486482));
#24303=CARTESIAN_POINT('Ctrl Pts',(38.4190961268959,-13.0686901791307,-39.5108890101577));
#24304=CARTESIAN_POINT('Ctrl Pts',(38.4155748665864,-13.0568974025755,-39.47679947463));
#24305=CARTESIAN_POINT('Ctrl Pts',(38.4119452755458,-13.0447418240704,-39.4416611826959));
#24306=CARTESIAN_POINT('Ctrl Pts',(38.4074384431895,-13.0321818870426,-39.406740292716));
#24307=CARTESIAN_POINT('Ctrl Pts',(38.4020915182394,-13.0192318837648,-39.3720754913156));
#24308=CARTESIAN_POINT('Ctrl Pts',(38.3968155709718,-13.0064537851295,-39.3378708473499));
#24309=CARTESIAN_POINT('Ctrl Pts',(38.390722128783,-12.9932945861615,-39.3039153924143));
#24310=CARTESIAN_POINT('Ctrl Pts',(38.3838028214921,-12.9797471343051,-39.2702608213597));
#24311=CARTESIAN_POINT('Ctrl Pts',(38.3767438853237,-12.9659263002422,-39.2359271144062));
#24312=CARTESIAN_POINT('Ctrl Pts',(38.3688259942699,-12.9516999140197,-39.201906366769));
#24313=CARTESIAN_POINT('Ctrl Pts',(38.3599859968467,-12.9370593466235,-39.1682713601004));
#24314=CARTESIAN_POINT('Ctrl Pts',(38.3518796591162,-12.923633846796,-39.1374278303379));
#24315=CARTESIAN_POINT('Ctrl Pts',(38.3429974054472,-12.9098590019422,-39.1069088406553));
#24316=CARTESIAN_POINT('Ctrl Pts',(38.3332466950008,-12.8957449858576,-39.0767849714504));
#24317=CARTESIAN_POINT('Ctrl Pts',(38.3323642122487,-12.894467604499,-39.0740586270322));
#24318=CARTESIAN_POINT('Ctrl Pts',(38.3314745869667,-12.8931874634454,-39.0713355286148));
#24319=CARTESIAN_POINT('Ctrl Pts',(38.3305777332763,-12.8919045823054,-39.0686157342182));
#24320=CARTESIAN_POINT('Origin',(28.0161439142367,-12.8919045823054,-39.8716842439453));
#24321=CARTESIAN_POINT('Origin',(28.0161439142367,-12.8919045823054,-39.8716842439453));
#24322=CARTESIAN_POINT('Ctrl Pts',(0.0835265683425695,-6.00666333723547,
-48.3550824830876));
#24323=CARTESIAN_POINT('Ctrl Pts',(-0.26751873653172,-6.01200137934907,
-48.3550825994612));
#24324=CARTESIAN_POINT('Ctrl Pts',(-0.618388065391316,-6.02125184123581,
-48.3536254076414));
#24325=CARTESIAN_POINT('Ctrl Pts',(-1.31980082412786,-6.04818290219911,
-48.350297799115));
#24326=CARTESIAN_POINT('Ctrl Pts',(-1.67034425400482,-6.06586350127566,
-48.3484273824083));
#24327=CARTESIAN_POINT('Ctrl Pts',(-2.72152477473183,-6.1324584507553,-48.3459483822083));
#24328=CARTESIAN_POINT('Ctrl Pts',(-3.4237971299004,-6.17306838545285,-48.3412545192219));
#24329=CARTESIAN_POINT('Ctrl Pts',(-4.1255125788106,-6.20946968450873,-48.331053858379));
#24330=CARTESIAN_POINT('Ctrl Pts',(-0.267518736531456,-6.00132529512168,
-48.3550823667144));
#24331=CARTESIAN_POINT('Ctrl Pts',(-0.540535156492418,-6.00879525432304,
-48.3541407510376));
#24332=CARTESIAN_POINT('Ctrl Pts',(-0.831277824766847,-6.01828947675663,
-48.3524253715914));
#24333=CARTESIAN_POINT('Ctrl Pts',(-1.4451628644355,-6.04432658407313,-48.3485410606893));
#24334=CARTESIAN_POINT('Ctrl Pts',(-1.76830361626289,-6.06089216512314,
-48.3463749782546));
#24335=CARTESIAN_POINT('Ctrl Pts',(-2.78175048167905,-6.12571278894255,
-48.3427355507996));
#24336=CARTESIAN_POINT('Ctrl Pts',(-3.45976825406929,-6.16367997403223,
-48.3372561067169));
#24337=CARTESIAN_POINT('Ctrl Pts',(-4.12617092612534,-6.19747947412217,
-48.3260557751568));
#24338=CARTESIAN_POINT('Ctrl Pts',(-0.618615979168657,-5.99973567328051,
-48.3536249385721));
#24339=CARTESIAN_POINT('Ctrl Pts',(-0.83162301880144,-6.00835114797883,
-48.352053093828));
#24340=CARTESIAN_POINT('Ctrl Pts',(-1.07630838456854,-6.01789996842699,
-48.3500372977422));
#24341=CARTESIAN_POINT('Ctrl Pts',(-1.6193471348745,-6.04289085428944,-48.3454511925192));
#24342=CARTESIAN_POINT('Ctrl Pts',(-1.91769809006312,-6.05836696395434,
-48.3428851569135));
#24343=CARTESIAN_POINT('Ctrl Pts',(-2.87872640181385,-6.11975101512502,
-48.3377026418223));
#24344=CARTESIAN_POINT('Ctrl Pts',(-3.52173694667449,-6.15479195325804,
-48.3313642359895));
#24345=CARTESIAN_POINT('Ctrl Pts',(-4.1268396622487,-6.18527410484422,-48.3199255790051));
#24346=CARTESIAN_POINT('Ctrl Pts',(-1.3209415423196,-5.99820579736957,-48.3438941182277));
#24347=CARTESIAN_POINT('Ctrl Pts',(-1.44672510894581,-6.00829173506076,
-48.3421773991346));
#24348=CARTESIAN_POINT('Ctrl Pts',(-1.62065368286856,-6.01814206512116,
-48.3401377766449));
#24349=CARTESIAN_POINT('Ctrl Pts',(-2.04329097938473,-6.04173521008609,
-48.3350871089986));
#24350=CARTESIAN_POINT('Ctrl Pts',(-2.29199666529032,-6.0555205803039,-48.3320814057566));
#24351=CARTESIAN_POINT('Ctrl Pts',(-3.11802710747004,-6.10935599904102,
-48.3246778342889));
#24352=CARTESIAN_POINT('Ctrl Pts',(-3.66733280245846,-6.13882811018935,
-48.3171415019516));
#24353=CARTESIAN_POINT('Ctrl Pts',(-4.12827543127815,-6.16205725113852,
-48.3065253445717));
#24354=CARTESIAN_POINT('Ctrl Pts',(-1.67216986283335,-5.9982655432998,-48.3356207260257));
#24355=CARTESIAN_POINT('Ctrl Pts',(-1.77074437171872,-6.00864450579839,
-48.3343702273337));
#24356=CARTESIAN_POINT('Ctrl Pts',(-1.91997597377325,-6.0187257861122,-48.3325976279209));
#24357=CARTESIAN_POINT('Ctrl Pts',(-2.29305999396389,-6.04195544062549,
-48.3277770168035));
#24358=CARTESIAN_POINT('Ctrl Pts',(-2.51690957785804,-6.05514353311736,
-48.3247339908856));
#24359=CARTESIAN_POINT('Ctrl Pts',(-3.26035692792899,-6.10489083408603,
-48.3166668014157));
#24360=CARTESIAN_POINT('Ctrl Pts',(-3.75095996563724,-6.13175228789484,
-48.3088106386412));
#24361=CARTESIAN_POINT('Ctrl Pts',(-4.12904246418424,-6.15104576671076,
-48.2992553062901));
#24362=CARTESIAN_POINT('Ctrl Pts',(-2.72609224471469,-5.99214762358687,
-48.2947245925476));
#24363=CARTESIAN_POINT('Ctrl Pts',(-2.78737351536448,-6.00381665756758,
-48.2942918711989));
#24364=CARTESIAN_POINT('Ctrl Pts',(-2.8843828599883,-6.01569196513299,-48.293681485549));
#24365=CARTESIAN_POINT('Ctrl Pts',(-3.12263860656582,-6.04033961885396,
-48.2916809761606));
#24366=CARTESIAN_POINT('Ctrl Pts',(-3.26388338895268,-6.05313466117662,
-48.2902937014433));
#24367=CARTESIAN_POINT('Ctrl Pts',(-3.71314893169586,-6.09364276617914,
-48.2862238404994));
#24368=CARTESIAN_POINT('Ctrl Pts',(-3.98882416158545,-6.11446024451105,
-48.2821814456289));
#24369=CARTESIAN_POINT('Ctrl Pts',(-4.13160728682495,-6.12223844465218,
-48.2774220038444));
#24370=CARTESIAN_POINT('Ctrl Pts',(-3.42734501756996,-5.99475664078893,
-48.2515240164107));
#24371=CARTESIAN_POINT('Ctrl Pts',(-3.46432076032786,-6.00697011627485,
-48.2527720832235));
#24372=CARTESIAN_POINT('Ctrl Pts',(-3.52649817491115,-6.02014444454774,
-48.2541165048377));
#24373=CARTESIAN_POINT('Ctrl Pts',(-3.67166030976089,-6.04594588203951,
-48.2567445235025));
#24374=CARTESIAN_POINT('Ctrl Pts',(-3.75464503002734,-6.05857299125839,
-48.2580281205531));
#24375=CARTESIAN_POINT('Ctrl Pts',(-3.99041609240001,-6.0919301033921,-48.2614073736106));
#24376=CARTESIAN_POINT('Ctrl Pts',(-4.13001933607955,-6.10813589078397,
-48.263031491523));
#24377=CARTESIAN_POINT('Ctrl Pts',(-4.13366096331968,-6.1084336923001,-48.2630127553113));
#24378=CARTESIAN_POINT('Ctrl Pts',(-4.12845481065586,-6.007051447105,-48.1954680629781));
#24379=CARTESIAN_POINT('Ctrl Pts',(-4.12850749787586,-6.01900581052064,
-48.200433936555));
#24380=CARTESIAN_POINT('Ctrl Pts',(-4.12864057911576,-6.03128117156189,
-48.2071191491468));
#24381=CARTESIAN_POINT('Ctrl Pts',(-4.12920120927171,-6.05467770199135,
-48.221588093388));
#24382=CARTESIAN_POINT('Ctrl Pts',(-4.12962875818777,-6.06579887137954,
-48.2293718250376));
#24383=CARTESIAN_POINT('Ctrl Pts',(-4.13155362590474,-6.09473681170807,
-48.2508605601154));
#24384=CARTESIAN_POINT('Ctrl Pts',(-4.13369316567446,-6.10812801481236,
-48.2627031036729));
#24385=CARTESIAN_POINT('Ctrl Pts',(-4.13722371861477,-6.1084337131847,-48.2627017315157));
#24386=CARTESIAN_POINT('Ctrl Pts',(-4.13722361839104,-6.10843370450313,
-48.2627017315515));
#24387=CARTESIAN_POINT('Ctrl Pts',(-4.13701407672473,-6.10841554618144,
-48.2627017996875));
#24388=CARTESIAN_POINT('Ctrl Pts',(-4.13685790799886,-6.10835892240998,
-48.262663281257));
#24389=CARTESIAN_POINT('Ctrl Pts',(-4.13674169752953,-6.10830758140055,
-48.2626265177434));
#24390=CARTESIAN_POINT('Ctrl Pts',(-4.13662522520969,-6.10825612470732,
-48.2625896713927));
#24391=CARTESIAN_POINT('Ctrl Pts',(-4.13654900508533,-6.10820886405876,
-48.2625535279384));
#24392=CARTESIAN_POINT('Ctrl Pts',(-4.13650271508106,-6.10817971723551,
-48.2625311962608));
#24393=CARTESIAN_POINT('Ctrl Pts',(-4.1364102317774,-6.10812148447991,-48.2624865795588));
#24394=CARTESIAN_POINT('Ctrl Pts',(-4.13635999437262,-6.10808254421846,
-48.2624559072796));
#24395=CARTESIAN_POINT('Ctrl Pts',(-4.13631216026214,-6.10804496697942,
-48.2624262729228));
#24396=CARTESIAN_POINT('Ctrl Pts',(-4.13621649204119,-6.10796981250135,
-48.2623670042092));
#24397=CARTESIAN_POINT('Ctrl Pts',(-4.13614678177369,-6.10790555146429,
-48.2623154903795));
#24398=CARTESIAN_POINT('Ctrl Pts',(-4.13607861507656,-6.10783843371639,
-48.262261395266));
#24399=CARTESIAN_POINT('Ctrl Pts',(-4.13584716396225,-6.10761054417216,
-48.2620777223754));
#24400=CARTESIAN_POINT('Ctrl Pts',(-4.13565789362604,-6.10735799473039,
-48.2618699174502));
#24401=CARTESIAN_POINT('Ctrl Pts',(-4.13549318405383,-6.10710655540123,
-48.2616620276179));
#24402=CARTESIAN_POINT('Ctrl Pts',(-4.13530295146511,-6.10681615361189,
-48.2614219236552));
#24403=CARTESIAN_POINT('Ctrl Pts',(-4.13514554673403,-6.10652655415251,
-48.2611810107393));
#24404=CARTESIAN_POINT('Ctrl Pts',(-4.13499914832338,-6.10622795083367,
-48.2609322939333));
#24405=CARTESIAN_POINT('Ctrl Pts',(-4.13499063034215,-6.10621057702851,
-48.2609178227032));
#24406=CARTESIAN_POINT('Ctrl Pts',(-4.13498215077319,-6.10619316218202,
-48.2609033158664));
#24407=CARTESIAN_POINT('Ctrl Pts',(-4.13497370572295,-6.10617570066421,
-48.2608887688412));
#24408=CARTESIAN_POINT('Ctrl Pts',(-4.13474598139209,-6.10570484349367,
-48.2604965021883));
#24409=CARTESIAN_POINT('Ctrl Pts',(-4.13455475664386,-6.10522791969297,
-48.2600983887895));
#24410=CARTESIAN_POINT('Ctrl Pts',(-4.13438266923931,-6.10475153053746,
-48.2597011835133));
#24411=CARTESIAN_POINT('Ctrl Pts',(-4.13411895040737,-6.10402147831793,
-48.2590924782348));
#24412=CARTESIAN_POINT('Ctrl Pts',(-4.13389862072628,-6.10328536512368,
-48.2584796979253));
#24413=CARTESIAN_POINT('Ctrl Pts',(-4.13370045808856,-6.10254802979483,
-48.2578680802102));
#24414=CARTESIAN_POINT('Ctrl Pts',(-4.13333556021568,-6.10119029608581,
-48.2567418436712));
#24415=CARTESIAN_POINT('Ctrl Pts',(-4.13304559573053,-6.0998260029529,-48.255617420827));
#24416=CARTESIAN_POINT('Ctrl Pts',(-4.1327886833905,-6.09845605313882,-48.2544972544273));
#24417=CARTESIAN_POINT('Ctrl Pts',(-4.13238882388217,-6.09632385715694,
-48.2527538224623));
#24418=CARTESIAN_POINT('Ctrl Pts',(-4.13207291555085,-6.09417845354371,
-48.2510208352385));
#24419=CARTESIAN_POINT('Ctrl Pts',(-4.1317961782277,-6.09202099947451,-48.2493008362025));
#24420=CARTESIAN_POINT('Ctrl Pts',(-4.13138155083735,-6.08878854950964,
-48.2467238122451));
#24421=CARTESIAN_POINT('Ctrl Pts',(-4.13105831741888,-6.0855286414402,-48.244175351545));
#24422=CARTESIAN_POINT('Ctrl Pts',(-4.13078034438517,-6.08224206853585,
-48.2416599697016));
#24423=CARTESIAN_POINT('Ctrl Pts',(-4.13058977880351,-6.07998894466698,
-48.239935539106));
#24424=CARTESIAN_POINT('Ctrl Pts',(-4.13042195826053,-6.07772362660907,
-48.2382269095075));
#24425=CARTESIAN_POINT('Ctrl Pts',(-4.13027038076009,-6.07544485148905,
-48.2365347367302));
#24426=CARTESIAN_POINT('Ctrl Pts',(-4.12989286227413,-6.06976934073926,
-48.2323202160853));
#24427=CARTESIAN_POINT('Ctrl Pts',(-4.12961378163258,-6.06401605346406,
-48.2282106199239));
#24428=CARTESIAN_POINT('Ctrl Pts',(-4.12938833601404,-6.05817109637975,
-48.2242324211879));
#24429=CARTESIAN_POINT('Ctrl Pts',(-4.12919574641795,-6.05317797240012,
-48.2208339976892));
#24430=CARTESIAN_POINT('Ctrl Pts',(-4.12904403874395,-6.04811857384527,
-48.2175317800084));
#24431=CARTESIAN_POINT('Ctrl Pts',(-4.12892089419374,-6.04297943677662,
-48.2143536212674));
#24432=CARTESIAN_POINT('Ctrl Pts',(-4.12878312414699,-6.03722994032761,
-48.2107980024637));
#24433=CARTESIAN_POINT('Ctrl Pts',(-4.12868136839902,-6.03138079133467,
-48.2073956831987));
#24434=CARTESIAN_POINT('Ctrl Pts',(-4.1286061408438,-6.02540321593081,-48.204215112076));
#24435=CARTESIAN_POINT('Ctrl Pts',(-4.12854502676884,-6.0205470965177,-48.2016312495348));
#24436=CARTESIAN_POINT('Ctrl Pts',(-4.12850159802488,-6.01560535413783,
-48.1991929077068));
#24437=CARTESIAN_POINT('Ctrl Pts',(-4.12847260770142,-6.01056187471018,
-48.1969709327471));
#24438=CARTESIAN_POINT('Ctrl Pts',(-4.12846591277299,-6.00939715042373,
-48.1964577972745));
#24439=CARTESIAN_POINT('Ctrl Pts',(-4.12845999189732,-6.0082270347227,-48.1959564051244));
#24440=CARTESIAN_POINT('Ctrl Pts',(-4.12845481065586,-6.00705144710501,
-48.1954680629781));
#24441=CARTESIAN_POINT('Ctrl Pts',(-29.2891959206732,-14.4313124010515,
-48.3540540388567));
#24442=CARTESIAN_POINT('Ctrl Pts',(-29.2899746397388,-14.7671408702645,
-48.3291878272403));
#24443=CARTESIAN_POINT('Ctrl Pts',(-29.2771538582069,-14.7669045053135,
-48.6657591384501));
#24444=CARTESIAN_POINT('Ctrl Pts',(-29.4909783664048,-14.4776157931207,
-48.3580817390519));
#24445=CARTESIAN_POINT('Ctrl Pts',(-29.4738070695996,-14.7670932226239,
-48.3824331547409));
#24446=CARTESIAN_POINT('Ctrl Pts',(-29.5030413152524,-14.766904515933,-48.6738002220355));
#24447=CARTESIAN_POINT('Ctrl Pts',(-29.6888652328203,-14.5232222287052,
-48.3502871282448));
#24448=CARTESIAN_POINT('Ctrl Pts',(-29.6826141588837,-14.7670538266072,
-48.4107537194043));
#24449=CARTESIAN_POINT('Ctrl Pts',(-29.7249751299964,-14.7669045263941,
-48.6581913870529));
#24450=CARTESIAN_POINT('Ctrl Pts',(-30.0744334835308,-14.6124212350924,
-48.3047943346257));
#24451=CARTESIAN_POINT('Ctrl Pts',(-30.0911805469422,-14.7669897766034,
-48.3969112259716));
#24452=CARTESIAN_POINT('Ctrl Pts',(-30.1581350349744,-14.7669045468573,
-48.5671620693194));
#24453=CARTESIAN_POINT('Ctrl Pts',(-30.266548451205,-14.657050343384,-48.26838676292));
#24454=CARTESIAN_POINT('Ctrl Pts',(-30.3019621750083,-14.7669625172305,
-48.3638427252435));
#24455=CARTESIAN_POINT('Ctrl Pts',(-30.3752125459255,-14.766904557097,-48.4937819709548));
#24456=CARTESIAN_POINT('Ctrl Pts',(-30.4284642980806,-14.6947854519677,
-48.1964235659436));
#24457=CARTESIAN_POINT('Ctrl Pts',(-30.4842634718295,-14.7669413153223,
-48.2634723170081));
#24458=CARTESIAN_POINT('Ctrl Pts',(-30.5563486668935,-14.7669045657556,
-48.3506792970572));
#24459=CARTESIAN_POINT('Origin',(-30.4628904239763,-14.4544045823054,-48.4165189096496));
#24460=CARTESIAN_POINT('Origin',(0.0835265683620477,-14.4544045823054,0.0824317919394229));
#24461=CARTESIAN_POINT('Origin',(32.2559828833067,-14.4544045823054,-47.3534709072605));
#24462=CARTESIAN_POINT('Ctrl Pts',(32.1346390008072,-14.6836564585996,-47.1787761295051));
#24463=CARTESIAN_POINT('Ctrl Pts',(32.3631522226839,-14.7195047625521,-47.0671198130351));
#24464=CARTESIAN_POINT('Ctrl Pts',(32.3073948493568,-14.9046273277204,-46.8980302578828));
#24465=CARTESIAN_POINT('Ctrl Pts',(31.9843639648594,-14.2208393515122,-46.7214805263384));
#24466=CARTESIAN_POINT('Ctrl Pts',(32.2124425821686,-14.2572370951355,-46.6100784470017));
#24467=CARTESIAN_POINT('Ctrl Pts',(32.1566961228079,-14.4418102212117,-46.441021989494));
#24468=CARTESIAN_POINT('Ctrl Pts',(31.8340251513167,-13.7582547217141,-46.2639539460438));
#24469=CARTESIAN_POINT('Ctrl Pts',(32.0615622174417,-13.7949155819462,-46.1525193435408));
#24470=CARTESIAN_POINT('Ctrl Pts',(32.0059240732351,-13.9792255914462,-45.9837913620383));
#24471=CARTESIAN_POINT('Ctrl Pts',(31.6836214013763,-13.2959337131846,-45.8061901631445));
#24472=CARTESIAN_POINT('Ctrl Pts',(31.9104948844699,-13.3325299785125,-45.6943932409652));
#24473=CARTESIAN_POINT('Ctrl Pts',(31.8550769043756,-13.5169045823054,-45.5263329281778));
#24474=CARTESIAN_POINT('Ctrl Pts',(32.1607495589358,-14.4544045595331,-46.4533144213431));
#24475=CARTESIAN_POINT('Ctrl Pts',(32.1704524589662,-14.464589809121,-46.4827393915657));
#24476=CARTESIAN_POINT('Ctrl Pts',(32.1792350499887,-14.4747854410079,-46.5124192299058));
#24477=CARTESIAN_POINT('Ctrl Pts',(32.1870746530974,-14.4849571274431,-46.5423134022322));
#24478=CARTESIAN_POINT('Ctrl Pts',(32.1943891325094,-14.4944474791847,-46.5702051596324));
#24479=CARTESIAN_POINT('Ctrl Pts',(32.200883324293,-14.5039154723654,-46.5982848321975));
#24480=CARTESIAN_POINT('Ctrl Pts',(32.2064963987694,-14.5133279314553,-46.6265388357118));
#24481=CARTESIAN_POINT('Ctrl Pts',(32.2118478660973,-14.522301706435,-46.6534760120001));
#24482=CARTESIAN_POINT('Ctrl Pts',(32.2163984055497,-14.5312237762477,-46.6805728996695));
#24483=CARTESIAN_POINT('Ctrl Pts',(32.2200515628477,-14.5400795913951,-46.7078177704894));
#24484=CARTESIAN_POINT('Ctrl Pts',(32.2234471358259,-14.5483109825347,-46.7331416039858));
#24485=CARTESIAN_POINT('Ctrl Pts',(32.2260667128419,-14.5564843935868,-46.7585942678845));
#24486=CARTESIAN_POINT('Ctrl Pts',(32.2277998636429,-14.5646141114394,-46.7841509175346));
#24487=CARTESIAN_POINT('Ctrl Pts',(32.2285348731612,-14.5680618322026,-46.7949892016216));
#24488=CARTESIAN_POINT('Ctrl Pts',(32.2291100930038,-14.5715020908807,-46.8058459067609));
#24489=CARTESIAN_POINT('Ctrl Pts',(32.2295157094557,-14.5749379971499,-46.8167175507953));
#24490=CARTESIAN_POINT('Ctrl Pts',(32.2302341780251,-14.5810240191791,-46.835974497843));
#24491=CARTESIAN_POINT('Ctrl Pts',(32.2304309663889,-14.5871115455618,-46.8552737733236));
#24492=CARTESIAN_POINT('Ctrl Pts',(32.2299898035979,-14.593121590845,-46.8745857273906));
#24493=CARTESIAN_POINT('Ctrl Pts',(32.2295649448931,-14.5989095224365,-46.893183968131));
#24494=CARTESIAN_POINT('Ctrl Pts',(32.2285476864384,-14.6046251025894,-46.9117947067213));
#24495=CARTESIAN_POINT('Ctrl Pts',(32.226808708919,-14.6102297042048,-46.9303675333675));
#24496=CARTESIAN_POINT('Ctrl Pts',(32.2251621322189,-14.6155365045113,-46.947953490212));
#24497=CARTESIAN_POINT('Ctrl Pts',(32.222867550472,-14.6207436431622,-46.9655059347368));
#24498=CARTESIAN_POINT('Ctrl Pts',(32.2198039300316,-14.6258519573891,-46.9829517238513));
#24499=CARTESIAN_POINT('Ctrl Pts',(32.2186440659339,-14.62778592747,-46.9895565709079));
#24500=CARTESIAN_POINT('Ctrl Pts',(32.2173739277389,-14.6297061021636,-46.9961457718268));
#24501=CARTESIAN_POINT('Ctrl Pts',(32.2159869766137,-14.6316139267949,-47.0027139299464));
#24502=CARTESIAN_POINT('Ctrl Pts',(32.2132964611226,-14.6353148731598,-47.0154553530929));
#24503=CARTESIAN_POINT('Ctrl Pts',(32.2102245596925,-14.6390800656586,-47.0281862151157));
#24504=CARTESIAN_POINT('Ctrl Pts',(32.2066063719569,-14.6427512671794,-47.0408006165906));
#24505=CARTESIAN_POINT('Ctrl Pts',(32.2031615521097,-14.6462465606208,-47.0528105905711));
#24506=CARTESIAN_POINT('Ctrl Pts',(32.1992207015494,-14.649656542816,-47.0647153880478));
#24507=CARTESIAN_POINT('Ctrl Pts',(32.1946310810407,-14.6528783603918,-47.0763929094605));
#24508=CARTESIAN_POINT('Ctrl Pts',(32.1902432135721,-14.6559585515544,-47.0875571040216));
#24509=CARTESIAN_POINT('Ctrl Pts',(32.1852614610874,-14.6588667966843,-47.0985138216531));
#24510=CARTESIAN_POINT('Ctrl Pts',(32.1795549189995,-14.6615453756132,-47.1091229500894));
#24511=CARTESIAN_POINT('Ctrl Pts',(32.1740290872121,-14.6641391314047,-47.1193961169648));
#24512=CARTESIAN_POINT('Ctrl Pts',(32.1678226434197,-14.6665177507396,-47.1293434730558));
#24513=CARTESIAN_POINT('Ctrl Pts',(32.1608329021082,-14.6686579758318,-47.1388029396664));
#24514=CARTESIAN_POINT('Ctrl Pts',(32.1541159295901,-14.6707146804345,-47.1478932585248));
#24515=CARTESIAN_POINT('Ctrl Pts',(32.146674683016,-14.6725517512568,-47.1565328027866));
#24516=CARTESIAN_POINT('Ctrl Pts',(32.1384470677752,-14.6741705573068,-47.1645458719539));
#24517=CARTESIAN_POINT('Ctrl Pts',(32.1363333475157,-14.6745864376128,-47.1666044741302));
#24518=CARTESIAN_POINT('Ctrl Pts',(32.1341679203907,-14.6749880046772,-47.1686215712106));
#24519=CARTESIAN_POINT('Ctrl Pts',(32.13195017295,-14.6753754514101,-47.1705938672733));
#24520=CARTESIAN_POINT('Origin',(14.8778438489026,-13.5169045823054,4.96086600976507));
#24521=CARTESIAN_POINT('Origin',(29.344152791651,-13.5169045823054,-38.9095962781799));
#24522=CARTESIAN_POINT('Origin',(0.0835265683620477,-12.8919045823054,0.0824317919394229));
#24523=CARTESIAN_POINT('Ctrl Pts',(29.326104774044,-12.8919045823054,-38.5318534679819));
#24524=CARTESIAN_POINT('Ctrl Pts',(29.326104774044,-12.9139187960401,-38.5318534679819));
#24525=CARTESIAN_POINT('Ctrl Pts',(29.3262379991816,-12.9356278245235,-38.534839371807));
#24526=CARTESIAN_POINT('Ctrl Pts',(29.3264870838848,-12.9566097073251,-38.5403603727184));
#24527=CARTESIAN_POINT('Ctrl Pts',(29.3267304618257,-12.9771108756647,-38.5457548823607));
#24528=CARTESIAN_POINT('Ctrl Pts',(29.3270844381453,-12.9969176625798,-38.5535693851653));
#24529=CARTESIAN_POINT('Ctrl Pts',(29.3275331992697,-13.0156824718681,-38.5633972432341));
#24530=CARTESIAN_POINT('Ctrl Pts',(29.327995837035,-13.0350275286559,-38.5735289994125));
#24531=CARTESIAN_POINT('Ctrl Pts',(29.3285591963311,-13.0532645768243,-38.5858001371315));
#24532=CARTESIAN_POINT('Ctrl Pts',(29.3292065902322,-13.0700686738468,-38.5997854381345));
#24533=CARTESIAN_POINT('Ctrl Pts',(29.329811080222,-13.0857591343542,-38.6128439091002));
#24534=CARTESIAN_POINT('Ctrl Pts',(29.3304888352246,-13.1002006435729,-38.6273968808538));
#24535=CARTESIAN_POINT('Ctrl Pts',(29.3312269160076,-13.1131767225615,-38.6431179310376));
#24536=CARTESIAN_POINT('Ctrl Pts',(29.3312793015773,-13.1140977047963,-38.6442337386668));
#24537=CARTESIAN_POINT('Ctrl Pts',(29.331331991325,-13.1150113249639,-38.6453554392112));
#24538=CARTESIAN_POINT('Ctrl Pts',(29.3313849807581,-13.1159175149051,-38.6464829200197));
#24539=CARTESIAN_POINT('Ctrl Pts',(29.33152105734,-13.1182446058459,-38.6493782847288));
#24540=CARTESIAN_POINT('Ctrl Pts',(29.3316591563938,-13.1205242789863,-38.6523112691164));
#24541=CARTESIAN_POINT('Ctrl Pts',(29.3317991613583,-13.1227565895721,-38.6552792745761));
#24542=CARTESIAN_POINT('Ctrl Pts',(29.3324793477165,-13.1336018279018,-38.6696987405676));
#24543=CARTESIAN_POINT('Ctrl Pts',(29.3332010329856,-13.1433259542997,-38.6849362776199));
#24544=CARTESIAN_POINT('Ctrl Pts',(29.3339549946389,-13.1519718239002,-38.7007769154678));
#24545=CARTESIAN_POINT('Ctrl Pts',(29.3347774710834,-13.161403369998,-38.7180570403117));
#24546=CARTESIAN_POINT('Ctrl Pts',(29.3356383745261,-13.1695524259128,-38.736055450668));
#24547=CARTESIAN_POINT('Ctrl Pts',(29.3365286964844,-13.1764446443693,-38.7545492977395));
#24548=CARTESIAN_POINT('Ctrl Pts',(29.3374556677569,-13.1836205748887,-38.7738044276311));
#24549=CARTESIAN_POINT('Ctrl Pts',(29.3384145864597,-13.1894346380349,-38.7935979691783));
#24550=CARTESIAN_POINT('Ctrl Pts',(29.3393977354577,-13.1938753423343,-38.8137207235506));
#24551=CARTESIAN_POINT('Ctrl Pts',(29.340386391301,-13.1983409200474,-38.8339561901333));
#24552=CARTESIAN_POINT('Ctrl Pts',(29.3413996267514,-13.2014181302613,-38.8545262160037));
#24553=CARTESIAN_POINT('Ctrl Pts',(29.3424309768835,-13.2030479859161,-38.8752367598351));
#24554=CARTESIAN_POINT('Ctrl Pts',(29.342999734741,-13.2039468011501,-38.8866579873821));
#24555=CARTESIAN_POINT('Ctrl Pts',(29.3435740193766,-13.2044045823054,-38.8981221352879));
#24556=CARTESIAN_POINT('Ctrl Pts',(29.344152791651,-13.2044045823054,-38.9095962781799));
#24557=CARTESIAN_POINT('Ctrl Pts',(38.5478788395692,-13.5144022989996,-39.7276020745818));
#24558=CARTESIAN_POINT('Ctrl Pts',(38.6381834185545,-13.1933434847834,-40.0014593274924));
#24559=CARTESIAN_POINT('Ctrl Pts',(38.9993997115465,-13.2935409838962,-39.7876377918258));
#24560=CARTESIAN_POINT('Ctrl Pts',(37.6321471688162,-10.8876754024414,-36.9505584011307));
#24561=CARTESIAN_POINT('Ctrl Pts',(37.7135976841852,-10.5315615565335,-37.197564861227));
#24562=CARTESIAN_POINT('Ctrl Pts',(38.0873367198682,-10.6668492065293,-37.0070442715679));
#24563=CARTESIAN_POINT('Ctrl Pts',(36.7092038782167,-8.28316551512454,-34.1516448023406));
#24564=CARTESIAN_POINT('Ctrl Pts',(36.7875685005852,-7.90880841569709,-34.3892929975985));
#24565=CARTESIAN_POINT('Ctrl Pts',(37.1684809904989,-8.06235637916793,-34.2039263650138));
#24566=CARTESIAN_POINT('Ctrl Pts',(35.7758342203384,-5.72100917799142,-31.3211122498619));
#24567=CARTESIAN_POINT('Ctrl Pts',(35.8691121688728,-5.37442442506644,-31.6039865296246));
#24568=CARTESIAN_POINT('Ctrl Pts',(36.2397262089015,-5.50017070394688,-31.3680265018349));
#24569=CARTESIAN_POINT('Ctrl Pts',(36.2681294096903,-7.07886051013668,-32.8140443877542));
#24570=CARTESIAN_POINT('Ctrl Pts',(36.2569664163808,-6.97591157388989,-32.7801889939238));
#24571=CARTESIAN_POINT('Ctrl Pts',(36.2554727333015,-6.87711064623287,-32.7339348504581));
#24572=CARTESIAN_POINT('Ctrl Pts',(36.2630467530083,-6.68740381001557,-32.6293153550853));
#24573=CARTESIAN_POINT('Ctrl Pts',(36.2724147441973,-6.59673597566758,-32.570618363652));
#24574=CARTESIAN_POINT('Ctrl Pts',(36.30162041965,-6.42451466437639,-32.4414153041646));
#24575=CARTESIAN_POINT('Ctrl Pts',(36.321062466775,-6.34396835910598,-32.3720253866706));
#24576=CARTESIAN_POINT('Ctrl Pts',(36.361286826097,-6.23614184370369,-32.256689531614));
#24577=CARTESIAN_POINT('Ctrl Pts',(36.3765528768977,-6.2025085626214,-32.216414958201));
#24578=CARTESIAN_POINT('Ctrl Pts',(36.4125915840679,-6.14483638321709,-32.1317287552063));
#24579=CARTESIAN_POINT('Ctrl Pts',(36.4332088055153,-6.11985717446073,-32.0871018700298));
#24580=CARTESIAN_POINT('Ctrl Pts',(36.459401450406,-6.10843371318468,-32.0401832160515));
#24581=CARTESIAN_POINT('Origin',(35.9713494567465,-14.7669045823054,-32.9119111827578));
#24582=CARTESIAN_POINT('Origin',(35.9713494567465,-12.8919045823054,-32.9119111827578));
#24583=CARTESIAN_POINT('Origin',(35.9713494567465,-7.07886995352309,-32.9119111827578));
#24584=CARTESIAN_POINT('Origin',(22.6388808156566,-12.8919045823054,7.52007219592841));
#24585=CARTESIAN_POINT('Origin',(35.9713494567465,-12.8919045823054,-32.9119111827578));
#24586=CARTESIAN_POINT('Origin',(0.0835265683620477,-13.5169045823054,0.0824317919394229));
#24587=CARTESIAN_POINT('Origin',(37.084741276154,-13.5169045823054,-41.2777797274919));
#24588=CARTESIAN_POINT('Ctrl Pts',(36.2784254248408,-7.15534954851098,-32.836829591711));
#24589=CARTESIAN_POINT('Ctrl Pts',(36.1434013184732,-7.11664814656864,-32.2629428084027));
#24590=CARTESIAN_POINT('Ctrl Pts',(35.7454348445936,-7.18677502471099,-32.6959179419936));
#24591=CARTESIAN_POINT('Ctrl Pts',(36.2588919622279,-7.03238137414826,-32.8057216385754));
#24592=CARTESIAN_POINT('Ctrl Pts',(36.0761096691241,-7.08021162576623,-32.3364442437081));
#24593=CARTESIAN_POINT('Ctrl Pts',(35.7317594193323,-7.01162141076107,-32.7107648798629));
#24594=CARTESIAN_POINT('Ctrl Pts',(36.2544224233627,-6.9007862514849,-32.7478923847614));
#24595=CARTESIAN_POINT('Ctrl Pts',(36.0343634050485,-6.94927177594153,-32.3814124480413));
#24596=CARTESIAN_POINT('Ctrl Pts',(35.7530195024256,-6.83269992253369,-32.6877129958713));
#24597=CARTESIAN_POINT('Ctrl Pts',(36.2640203102083,-6.67697195553546,-32.6234372773615));
#24598=CARTESIAN_POINT('Ctrl Pts',(36.0276939617195,-6.69622936404188,-32.3874954073924));
#24599=CARTESIAN_POINT('Ctrl Pts',(35.8268903954434,-6.53795985193932,-32.6071031454275));
#24600=CARTESIAN_POINT('Ctrl Pts',(36.2744837959597,-6.58104909157633,-32.5604598516983));
#24601=CARTESIAN_POINT('Ctrl Pts',(36.0416953029314,-6.57996991861108,-32.371645126971));
#24602=CARTESIAN_POINT('Ctrl Pts',(35.8724674696584,-6.41511471179818,-32.5572714061768));
#24603=CARTESIAN_POINT('Ctrl Pts',(36.3068728829042,-6.40173475569586,-32.4227465017006));
#24604=CARTESIAN_POINT('Ctrl Pts',(36.100847967489,-6.36383534698761,-32.3054510953759));
#24605=CARTESIAN_POINT('Ctrl Pts',(35.9858853058558,-6.19278444406274,-32.4324748322831));
#24606=CARTESIAN_POINT('Ctrl Pts',(36.3281094141996,-6.32050524456542,-32.3501393983736));
#24607=CARTESIAN_POINT('Ctrl Pts',(36.1424453507782,-6.2630776214194,-32.2590472164985));
#24608=CARTESIAN_POINT('Ctrl Pts',(36.0517003472671,-6.09580032219768,-32.3597580486369));
#24609=CARTESIAN_POINT('Ctrl Pts',(36.3918485606395,-6.16373114058233,-32.1739515607077));
#24610=CARTESIAN_POINT('Ctrl Pts',(36.2655421565245,-6.07811517883126,-32.1210623649169));
#24611=CARTESIAN_POINT('Ctrl Pts',(36.2288436140461,-5.92198390393177,-32.1624016484031));
#24612=CARTESIAN_POINT('Ctrl Pts',(36.4367840484078,-6.09886182619368,-32.071567005352));
#24613=CARTESIAN_POINT('Ctrl Pts',(36.3533716225856,-6.00005797767508,-32.0222299156167));
#24614=CARTESIAN_POINT('Ctrl Pts',(36.343660429214,-5.86097989280999,-32.0334346821493));
#24615=CARTESIAN_POINT('Ctrl Pts',(36.4922864453313,-6.10268725739347,-31.9855710438836));
#24616=CARTESIAN_POINT('Ctrl Pts',(36.4460471988281,-6.01584203961169,-31.9169227992496));
#24617=CARTESIAN_POINT('Ctrl Pts',(36.4638571848965,-5.89881153279529,-31.896661392609));
#24618=CARTESIAN_POINT('Origin',(36.625034450523,-5.88746284406389,-32.186449528893));
#24619=CARTESIAN_POINT('Origin',(0.0835265683620477,-5.88746284406389,0.0824317919394229));
#24620=CARTESIAN_POINT('Origin',(-32.1853547524705,-5.88746284406389,-36.4590760902215));
#24621=CARTESIAN_POINT('Ctrl Pts',(-39.7265072775759,-13.5144022795305,
-38.3819204724802));
#24622=CARTESIAN_POINT('Ctrl Pts',(-40.0003645304861,-13.1933434652888,
-38.4722250514726));
#24623=CARTESIAN_POINT('Ctrl Pts',(-39.7865429947924,-13.2935409644279,
-38.8334413444868));
#24624=CARTESIAN_POINT('Ctrl Pts',(-36.9494636177385,-10.8876753960648,
-37.4661888062163));
#24625=CARTESIAN_POINT('Ctrl Pts',(-37.196470078124,-10.5315615503784,-37.5476393216535));
#24626=CARTESIAN_POINT('Ctrl Pts',(-37.0059494882058,-10.6668492001279,
-37.921378357208));
#24627=CARTESIAN_POINT('Ctrl Pts',(-34.150550032778,-8.28316552163412,-36.5432455201772));
#24628=CARTESIAN_POINT('Ctrl Pts',(-34.3881982285108,-7.90880842257625,
-36.621610142688));
#24629=CARTESIAN_POINT('Ctrl Pts',(-34.2028315954194,-8.06235638571299,
-37.0025226324655));
#24630=CARTESIAN_POINT('Ctrl Pts',(-31.3200174944135,-5.72100919698887,
-35.609875866953));
#24631=CARTESIAN_POINT('Ctrl Pts',(-31.602891774127,-5.37442444417786,-35.7031538154752));
#24632=CARTESIAN_POINT('Ctrl Pts',(-31.3669317464438,-5.50017072293065,
-36.0737678554641));
#24633=CARTESIAN_POINT('Origin',(-38.9696572682695,-12.8919045823054,-38.4614003499128));
#24634=CARTESIAN_POINT('Ctrl Pts',(-32.8129496113305,-7.07886051013307,
-36.1021710493883));
#24635=CARTESIAN_POINT('Ctrl Pts',(-32.7790942175002,-6.97591157388758,
-36.0910080560792));
#24636=CARTESIAN_POINT('Ctrl Pts',(-32.732840074035,-6.87711064623175,-36.089514373));
#24637=CARTESIAN_POINT('Ctrl Pts',(-32.6282205786628,-6.68740381001556,
-36.0970883927067));
#24638=CARTESIAN_POINT('Ctrl Pts',(-32.5695235872295,-6.59673597566758,
-36.1064563838958));
#24639=CARTESIAN_POINT('Ctrl Pts',(-32.4403205277421,-6.42451466437638,
-36.1356620593484));
#24640=CARTESIAN_POINT('Ctrl Pts',(-32.3709306102481,-6.34396835910597,
-36.1551041064734));
#24641=CARTESIAN_POINT('Ctrl Pts',(-32.2555947551915,-6.23614184370368,
-36.1953284657954));
#24642=CARTESIAN_POINT('Ctrl Pts',(-32.2153201817785,-6.2025085626214,-36.2105945165962));
#24643=CARTESIAN_POINT('Ctrl Pts',(-32.1306339787838,-6.1448363832171,-36.2466332237663));
#24644=CARTESIAN_POINT('Ctrl Pts',(-32.0860070936073,-6.11985717446073,
-36.2672504452137));
#24645=CARTESIAN_POINT('Ctrl Pts',(-32.0390884396291,-6.10843371318469,
-36.2934430901044));
#24646=CARTESIAN_POINT('Origin',(0.0835265683620477,-14.4544045823054,0.0824317919394229));
#24647=CARTESIAN_POINT('Origin',(-43.0351235939456,-14.4544045823054,-37.6801663496809));
#24648=CARTESIAN_POINT('Origin',(-46.3845835303221,-14.4544045823054,-37.9450121028891));
#24649=CARTESIAN_POINT('Origin',(6.83612114566778,-14.4544045823054,-20.3954556167886));
#24650=CARTESIAN_POINT('Origin',(-42.442236506563,-14.4544045823054,-36.6450210147876));
#24651=CARTESIAN_POINT('Ctrl Pts',(32.1333443923172,-14.4267018210609,-46.3767934681345));
#24652=CARTESIAN_POINT('Ctrl Pts',(32.1052213194306,-14.7669045823054,-46.3888540627253));
#24653=CARTESIAN_POINT('Ctrl Pts',(32.4199640389762,-14.7669045823054,-46.2552612894439));
#24654=CARTESIAN_POINT('Ctrl Pts',(32.1917878197712,-14.4797609665066,-46.5273115522008));
#24655=CARTESIAN_POINT('Ctrl Pts',(32.2108318123702,-14.7669045823054,-46.4982492296413));
#24656=CARTESIAN_POINT('Ctrl Pts',(32.5026074478398,-14.7669045823054,-46.4513285344375));
#24657=CARTESIAN_POINT('Ctrl Pts',(32.229426473191,-14.5360769750833,-46.6948057129722));
#24658=CARTESIAN_POINT('Ctrl Pts',(32.2987356959689,-14.7669045823054,-46.6757640436418));
#24659=CARTESIAN_POINT('Ctrl Pts',(32.5416287263888,-14.7669045823054,-46.6753447743204));
#24660=CARTESIAN_POINT('Ctrl Pts',(32.2303679539465,-14.6333609973512,-47.0050021456081));
#24661=CARTESIAN_POINT('Ctrl Pts',(32.3251131331188,-14.7669045823054,-47.028208228159));
#24662=CARTESIAN_POINT('Ctrl Pts',(32.4805743442183,-14.7669045823054,-47.1044264916346));
#24663=CARTESIAN_POINT('Ctrl Pts',(32.1934182263391,-14.6768299128517,-47.1557619332086));
#24664=CARTESIAN_POINT('Ctrl Pts',(32.2752623675051,-14.7669045823054,-47.222653288913));
#24665=CARTESIAN_POINT('Ctrl Pts',(32.3777047498528,-14.7669045823054,-47.3212251413928));
#24666=CARTESIAN_POINT('Ctrl Pts',(32.0821172043475,-14.6796363815827,-47.2014099893353));
#24667=CARTESIAN_POINT('Ctrl Pts',(32.1108290781635,-14.7669045823054,-47.2879256345056));
#24668=CARTESIAN_POINT('Ctrl Pts',(32.1539578388482,-14.7669045823054,-47.4064123788888));
#24669=CARTESIAN_POINT('Origin',(32.4575305290195,-14.4544045823054,-46.3554507110303));
#24670=CARTESIAN_POINT('Ctrl Pts',(29.4342239561067,-12.8919045823054,-38.184865357424));
#24671=CARTESIAN_POINT('Ctrl Pts',(29.5041756346414,-12.8919045823054,-38.3970004975819));
#24672=CARTESIAN_POINT('Ctrl Pts',(29.326104774044,-12.8919045823054,-38.5318534679819));
#24673=CARTESIAN_POINT('Ctrl Pts',(29.4342239819946,-13.0608832998917,-38.1848654359315));
#24674=CARTESIAN_POINT('Ctrl Pts',(29.5041756540699,-12.9975414109167,-38.397000556497));
#24675=CARTESIAN_POINT('Ctrl Pts',(29.3261047525712,-12.9763939382004,-38.5318534842432));
#24676=CARTESIAN_POINT('Ctrl Pts',(29.4582227637604,-13.226389889153,-38.2576440316728));
#24677=CARTESIAN_POINT('Ctrl Pts',(29.5231089112903,-13.1003236725302,-38.4544174656888));
#24678=CARTESIAN_POINT('Ctrl Pts',(29.3280674855906,-13.0591472399313,-38.5758498536463));
#24679=CARTESIAN_POINT('Ctrl Pts',(29.5354545666183,-13.4534586900123,-38.4918568435322));
#24680=CARTESIAN_POINT('Ctrl Pts',(29.5773853840454,-13.2166231342364,-38.6190160485472));
#24681=CARTESIAN_POINT('Ctrl Pts',(29.3346698006211,-13.1726816319567,-38.7171327311836));
#24682=CARTESIAN_POINT('Ctrl Pts',(29.5885432101734,-13.5169045492971,-38.6528532209924));
#24683=CARTESIAN_POINT('Ctrl Pts',(29.6131548298068,-13.22877512521,-38.7274903060458));
#24684=CARTESIAN_POINT('Ctrl Pts',(29.3393370685557,-13.2044045823054,-38.8141247129866));
#24685=CARTESIAN_POINT('Ctrl Pts',(29.6409337685891,-13.5169045823054,-38.8117325886538));
#24686=CARTESIAN_POINT('Ctrl Pts',(29.6409337685891,-13.2044045823054,-38.8117325886538));
#24687=CARTESIAN_POINT('Ctrl Pts',(29.344152791651,-13.2044045823054,-38.9095962781799));
#24688=CARTESIAN_POINT('Origin',(29.1374429791686,-12.8919045823054,-38.2827290469501));
#24689=CARTESIAN_POINT('Origin',(35.9713494567465,-12.8919045823054,-32.9119111827578));
#24690=CARTESIAN_POINT('Origin',(35.9713494567465,-12.8919045823054,-32.9119111827578));
#24691=CARTESIAN_POINT('Origin',(37.084741276154,-13.5169045823054,-41.2777797274919));
#24692=CARTESIAN_POINT('Origin',(37.084741276154,-13.5169045823054,-41.2777797274919));
#24693=CARTESIAN_POINT('Origin',(37.084741276154,-13.5169045823054,-41.2777797274919));
#24694=CARTESIAN_POINT('Ctrl Pts',(48.5200123991582,-14.4313124010524,-29.2902906970955));
#24695=CARTESIAN_POINT('Ctrl Pts',(48.4951461875456,-14.7671408702692,-29.2910694161602));
#24696=CARTESIAN_POINT('Ctrl Pts',(48.8317174987565,-14.7669045053135,-29.2782486346292));
#24697=CARTESIAN_POINT('Ctrl Pts',(48.5240400993535,-14.4776157931193,-29.4920731428274));
#24698=CARTESIAN_POINT('Ctrl Pts',(48.5483915150367,-14.767093222629,-29.4749018460235));
#24699=CARTESIAN_POINT('Ctrl Pts',(48.839758582342,-14.766904515933,-29.5041360916753));
#24700=CARTESIAN_POINT('Ctrl Pts',(48.5162454885462,-14.523222228705,-29.6899600092429));
#24701=CARTESIAN_POINT('Ctrl Pts',(48.5767120797059,-14.7670538266106,-29.6837089353061));
#24702=CARTESIAN_POINT('Ctrl Pts',(48.8241497473579,-14.7669045263941,-29.7260699064196));
#24703=CARTESIAN_POINT('Ctrl Pts',(48.4707526949274,-14.6124212350926,-30.0755282599531));
#24704=CARTESIAN_POINT('Ctrl Pts',(48.562869586275,-14.7669897766053,-30.0922753233648));
#24705=CARTESIAN_POINT('Ctrl Pts',(48.733120429625,-14.7669045468573,-30.1592298113981));
#24706=CARTESIAN_POINT('Ctrl Pts',(48.4343451232206,-14.657050343383,-30.2676432276275));
#24707=CARTESIAN_POINT('Ctrl Pts',(48.5298010855454,-14.7669625172313,-30.3030569514312));
#24708=CARTESIAN_POINT('Ctrl Pts',(48.6597403312579,-14.766904557097,-30.3763073223494));
#24709=CARTESIAN_POINT('Ctrl Pts',(48.3623819262458,-14.6947854519682,-30.4295590745031));
#24710=CARTESIAN_POINT('Ctrl Pts',(48.4294306773109,-14.7669413153234,-30.4853582482525));
#24711=CARTESIAN_POINT('Ctrl Pts',(48.5166376573611,-14.7669045657556,-30.5574434433174));
#24712=CARTESIAN_POINT('Origin',(48.5824772699512,-14.4544045823054,-30.4639852003988));
#24713=CARTESIAN_POINT('Origin',(48.8335265683622,-14.4544045823054,-29.39085169964));
#24714=CARTESIAN_POINT('Ctrl Pts',(48.3955019191571,-14.6753754514261,-30.3462212704575));
#24715=CARTESIAN_POINT('Ctrl Pts',(48.4059549771833,-14.6685167481301,-30.3167552206967));
#24716=CARTESIAN_POINT('Ctrl Pts',(48.4153181071138,-14.6615856670197,-30.2869594234401));
#24717=CARTESIAN_POINT('Ctrl Pts',(48.4237914685547,-14.6546090802607,-30.2569496411699));
#24718=CARTESIAN_POINT('Ctrl Pts',(48.4330908949959,-14.646952348534,-30.2240142158746));
#24719=CARTESIAN_POINT('Ctrl Pts',(48.4413185922837,-14.6392407575335,-30.1908208469554));
#24720=CARTESIAN_POINT('Ctrl Pts',(48.448693282195,-14.6314992383765,-30.157477015652));
#24721=CARTESIAN_POINT('Ctrl Pts',(48.4565789660921,-14.6232213075498,-30.1218227824927));
#24722=CARTESIAN_POINT('Ctrl Pts',(48.4634889654078,-14.6149090026934,-30.0859958597154));
#24723=CARTESIAN_POINT('Ctrl Pts',(48.4696439731935,-14.6065829337798,-30.0500850635473));
#24724=CARTESIAN_POINT('Ctrl Pts',(48.4767477541929,-14.5969734300704,-30.0086387420524));
#24725=CARTESIAN_POINT('Ctrl Pts',(48.4828456977915,-14.5873453832268,-29.9670798327071));
#24726=CARTESIAN_POINT('Ctrl Pts',(48.4882202022897,-14.5777205278782,-29.9255015399208));
#24727=CARTESIAN_POINT('Ctrl Pts',(48.4900623043444,-14.5744216254734,-29.9112506524953));
#24728=CARTESIAN_POINT('Ctrl Pts',(48.4918190010901,-14.5711230389451,-29.8969972272884));
#24729=CARTESIAN_POINT('Ctrl Pts',(48.4935005335227,-14.5678255143183,-29.882744437463));
#24730=CARTESIAN_POINT('Ctrl Pts',(48.4938922373557,-14.5670573738945,-29.8794243276061));
#24731=CARTESIAN_POINT('Ctrl Pts',(48.4942794778329,-14.5662889835649,-29.8761029367338));
#24732=CARTESIAN_POINT('Ctrl Pts',(48.4946622853821,-14.5655203189316,-29.8727801599688));
#24733=CARTESIAN_POINT('Ctrl Pts',(48.5045170298835,-14.5457323247156,-29.7872407913554));
#24734=CARTESIAN_POINT('Ctrl Pts',(48.5113680830515,-14.5259112556565,-29.7014082137169));
#24735=CARTESIAN_POINT('Ctrl Pts',(48.5156165893993,-14.5060682995342,-29.615326399795));
#24736=CARTESIAN_POINT('Ctrl Pts',(48.5193003967565,-14.4888628108826,-29.5406863278512));
#24737=CARTESIAN_POINT('Ctrl Pts',(48.5210264259617,-14.4716407563751,-29.4658584862374));
#24738=CARTESIAN_POINT('Ctrl Pts',(48.5210265683534,-14.454406712551,-29.390860969846));
#24739=CARTESIAN_POINT('Origin',(48.8335265683622,-14.4544045823054,-44.2925682080603));
#24740=CARTESIAN_POINT('Origin',(48.8335265683619,-14.4544045823054,29.5557152835192));
#24741=CARTESIAN_POINT('Ctrl Pts',(48.5210265683619,-14.9741386829693,30.5390391682904));
#24742=CARTESIAN_POINT('Ctrl Pts',(48.521026568362,-14.8357920829888,30.6130226887234));
#24743=CARTESIAN_POINT('Ctrl Pts',(48.3952116457107,-14.7531448966902,30.657219870274));
#24744=CARTESIAN_POINT('Ctrl Pts',(48.5210265683619,-13.8793029117135,28.4917345041611));
#24745=CARTESIAN_POINT('Ctrl Pts',(48.521026568362,-13.7458678867053,28.5689805591673));
#24746=CARTESIAN_POINT('Ctrl Pts',(48.398801943192,-13.65830753268,28.6042407855062));
#24747=CARTESIAN_POINT('Ctrl Pts',(48.521026568362,-12.8434482902991,26.4086832687539));
#24748=CARTESIAN_POINT('Ctrl Pts',(48.521026568362,-12.7103751542363,26.4815899293964));
#24749=CARTESIAN_POINT('Ctrl Pts',(48.4024091291961,-12.6224528665228,26.5149273450437));
#24750=CARTESIAN_POINT('Ctrl Pts',(48.521026568362,-11.4077451872927,23.2124561823835));
#24751=CARTESIAN_POINT('Ctrl Pts',(48.521026568362,-11.2735898053172,23.2727809677033));
#24752=CARTESIAN_POINT('Ctrl Pts',(48.4076725172434,-11.186749940031,23.3082345578824));
#24753=CARTESIAN_POINT('Ctrl Pts',(48.521026568362,-10.9489604127228,22.1350468218994));
#24754=CARTESIAN_POINT('Ctrl Pts',(48.521026568362,-10.8151504288079,22.1928971400193));
#24755=CARTESIAN_POINT('Ctrl Pts',(48.4094014640764,-10.727965027292,22.2271571198222));
#24756=CARTESIAN_POINT('Ctrl Pts',(48.521026568362,-10.0773547210577,19.9523464052027));
#24757=CARTESIAN_POINT('Ctrl Pts',(48.521026568362,-9.94441815657111,20.0051547930602));
#24758=CARTESIAN_POINT('Ctrl Pts',(48.4127662077947,-9.85635900888213,20.0367328014427));
#24759=CARTESIAN_POINT('Ctrl Pts',(48.521026568362,-9.6651241319502,18.8479737078929));
#24760=CARTESIAN_POINT('Ctrl Pts',(48.521026568362,-9.53246556458668,18.898045866283));
#24761=CARTESIAN_POINT('Ctrl Pts',(48.4143999302067,-9.4441283020868,18.9283064327585));
#24762=CARTESIAN_POINT('Ctrl Pts',(48.521026568362,-7.75733423685905,13.3094986281149));
#24763=CARTESIAN_POINT('Ctrl Pts',(48.521026568362,-7.63508483859962,13.3708195365843));
#24764=CARTESIAN_POINT('Ctrl Pts',(48.4221223344704,-7.53633525782046,13.368780830614));
#24765=CARTESIAN_POINT('Ctrl Pts',(48.521026568362,-6.70462823796833,8.78094500538595));
#24766=CARTESIAN_POINT('Ctrl Pts',(48.521026568362,-6.57519149763907,8.81202019284637));
#24767=CARTESIAN_POINT('Ctrl Pts',(48.4269222766975,-6.48363668556734,8.82066537173487));
#24768=CARTESIAN_POINT('Ctrl Pts',(48.521026568362,-6.31501530004508,4.11515277179024));
#24769=CARTESIAN_POINT('Ctrl Pts',(48.5210265683621,-6.18536424665105,4.12597917065639));
#24770=CARTESIAN_POINT('Ctrl Pts',(48.4286992393282,-6.09401826674915,4.13360693755336));
#24771=CARTESIAN_POINT('Ctrl Pts',(48.3955019191565,-14.6753754514262,30.5110848543364));
#24772=CARTESIAN_POINT('Ctrl Pts',(48.4052064423862,-14.6690078941722,30.4837288439063));
#24773=CARTESIAN_POINT('Ctrl Pts',(48.4139628772557,-14.6625738073748,30.4560706196742));
#24774=CARTESIAN_POINT('Ctrl Pts',(48.4219415507532,-14.6560985772181,30.4282197016506));
#24775=CARTESIAN_POINT('Ctrl Pts',(48.4304079610655,-14.649227515833,30.3986662552492));
#24776=CARTESIAN_POINT('Ctrl Pts',(48.437998422541,-14.642310020426,30.3688953829949));
#24777=CARTESIAN_POINT('Ctrl Pts',(48.4448791359127,-14.6353661273908,30.3389935466465));
#24778=CARTESIAN_POINT('Ctrl Pts',(48.4525470064664,-14.6276278493874,30.3056709246955));
#24779=CARTESIAN_POINT('Ctrl Pts',(48.459333447508,-14.6198566891109,30.2721852455818));
#24780=CARTESIAN_POINT('Ctrl Pts',(48.4654246307801,-14.6120695184222,30.238609179989));
#24781=CARTESIAN_POINT('Ctrl Pts',(48.4722050743052,-14.6034011745691,30.2012337462881));
#24782=CARTESIAN_POINT('Ctrl Pts',(48.4781237366281,-14.5947127249934,30.1637451913772));
#24783=CARTESIAN_POINT('Ctrl Pts',(48.4833879588141,-14.586017636216,30.126200917409));
#24784=CARTESIAN_POINT('Ctrl Pts',(48.4871194262825,-14.5798542487752,30.0995882038902));
#24785=CARTESIAN_POINT('Ctrl Pts',(48.4905209582135,-14.5736872964226,30.0729464959421));
#24786=CARTESIAN_POINT('Ctrl Pts',(48.4936555202531,-14.5675203997113,30.0462908924709));
#24787=CARTESIAN_POINT('Ctrl Pts',(48.4939882725562,-14.5668657471449,30.0434612424802));
#24788=CARTESIAN_POINT('Ctrl Pts',(48.4943178162041,-14.5662108690007,30.0406304700051));
#24789=CARTESIAN_POINT('Ctrl Pts',(48.494644170793,-14.5655557443929,30.037798484972));
#24790=CARTESIAN_POINT('Ctrl Pts',(48.5055255724454,-14.5437124051737,29.9433736854619));
#24791=CARTESIAN_POINT('Ctrl Pts',(48.5127481549386,-14.5218400677965,29.8486407866783));
#24792=CARTESIAN_POINT('Ctrl Pts',(48.5168466348194,-14.4999508808714,29.7536469513485));
#24793=CARTESIAN_POINT('Ctrl Pts',(48.5196878200913,-14.48477666084,29.6877944661076));
#24794=CARTESIAN_POINT('Ctrl Pts',(48.5210264418471,-14.4695942532302,29.6218162870134));
#24795=CARTESIAN_POINT('Ctrl Pts',(48.521026568353,-14.4544067340556,29.555724647307));
#24796=CARTESIAN_POINT('Ctrl Pts',(48.3952465904111,-14.7531486984911,-30.4923081869096));
#24797=CARTESIAN_POINT('Ctrl Pts',(48.5210265683622,-14.8357969973015,-30.4481104474598));
#24798=CARTESIAN_POINT('Ctrl Pts',(48.5210265683622,-14.9741195676119,-30.3741398393454));
#24799=CARTESIAN_POINT('Ctrl Pts',(48.3988351428458,-13.6585793127145,-28.4398295995618));
#24800=CARTESIAN_POINT('Ctrl Pts',(48.5210265683622,-13.7461362596315,-28.40456192777));
#24801=CARTESIAN_POINT('Ctrl Pts',(48.5210265683622,-13.879550318061,-28.3273318462602));
#24802=CARTESIAN_POINT('Ctrl Pts',(48.4024400771286,-12.6231097579334,-26.3512944596022));
#24803=CARTESIAN_POINT('Ctrl Pts',(48.521026568354,-12.7110265271815,-26.3179447507229));
#24804=CARTESIAN_POINT('Ctrl Pts',(48.5210265683621,-12.8440806269501,-26.2450560710985));
#24805=CARTESIAN_POINT('Ctrl Pts',(48.4076994021303,-11.1881005852606,-23.1464093060635));
#24806=CARTESIAN_POINT('Ctrl Pts',(48.5210265683662,-11.2749369501022,-23.1109499665448));
#24807=CARTESIAN_POINT('Ctrl Pts',(48.5210265683621,-11.4090714544335,-23.0506307223895));
#24808=CARTESIAN_POINT('Ctrl Pts',(48.4094268834328,-10.7295656511245,-22.0660426670943));
#24809=CARTESIAN_POINT('Ctrl Pts',(48.5210265683621,-10.8167469967087,-22.0317755238263));
#24810=CARTESIAN_POINT('Ctrl Pts',(48.5210265683621,-10.9505365201845,-21.9739291535892));
#24811=CARTESIAN_POINT('Ctrl Pts',(48.4127885702549,-9.85847188921516,-19.877309020907));
#24812=CARTESIAN_POINT('Ctrl Pts',(48.5210265683621,-9.94652588376348,-19.8457214596911));
#24813=CARTESIAN_POINT('Ctrl Pts',(48.5210265683621,-10.0794427583968,-19.7929119202474));
#24814=CARTESIAN_POINT('Ctrl Pts',(48.4144238368348,-9.44570717935303,-18.767774646125));
#24815=CARTESIAN_POINT('Ctrl Pts',(48.5210265683621,-9.53404162556802,-18.7375113137474));
#24816=CARTESIAN_POINT('Ctrl Pts',(48.5210265683621,-9.66667804843002,-18.687434330509));
#24817=CARTESIAN_POINT('Ctrl Pts',(48.4221518448129,-7.53595817693283,-13.2034873916435));
#24818=CARTESIAN_POINT('Ctrl Pts',(48.5210265683621,-7.63471881015773,-13.2055633861815));
#24819=CARTESIAN_POINT('Ctrl Pts',(48.5210265683621,-7.75692904622885,-13.1442050984742));
#24820=CARTESIAN_POINT('Ctrl Pts',(48.4269499128865,-6.48350292014371,-8.65379177962918));
#24821=CARTESIAN_POINT('Ctrl Pts',(48.5210265683621,-6.57505277912449,-8.64513862080266));
#24822=CARTESIAN_POINT('Ctrl Pts',(48.5210265683621,-6.7044683038842,-8.61408311837201));
#24823=CARTESIAN_POINT('Ctrl Pts',(48.4287256539129,-6.0940504675403,-3.96881378790178));
#24824=CARTESIAN_POINT('Ctrl Pts',(48.5210265683621,-6.18539206100946,-3.96118625151467));
#24825=CARTESIAN_POINT('Ctrl Pts',(48.5210265683621,-6.3150213366611,-3.95036147849161));
#24826=CARTESIAN_POINT('Origin',(0.0835265683620477,-5.88746284406389,0.0824317919394229));
#24827=CARTESIAN_POINT('Ctrl Pts',(-32.8357348152455,-7.15534954835,-36.112467064513));
#24828=CARTESIAN_POINT('Ctrl Pts',(-32.2618480320884,-7.11664814651665,
-35.9774429580661));
#24829=CARTESIAN_POINT('Ctrl Pts',(-32.6948231655917,-7.18677502448105,
-35.579476484273));
#24830=CARTESIAN_POINT('Ctrl Pts',(-32.8046268621034,-7.03238137403248,
-36.0929336019227));
#24831=CARTESIAN_POINT('Ctrl Pts',(-32.335349467333,-7.08021162563639,-35.9101513087856));
#24832=CARTESIAN_POINT('Ctrl Pts',(-32.7096701034189,-7.01162141060435,
-35.5658010590506));
#24833=CARTESIAN_POINT('Ctrl Pts',(-32.7467976083082,-6.90078625143033,
-36.0884640630633));
#24834=CARTESIAN_POINT('Ctrl Pts',(-32.3803176716213,-6.94927177586967,
-35.868405044745));
#24835=CARTESIAN_POINT('Ctrl Pts',(-32.6866182194288,-6.83269992246191,
-35.5870611421423));
#24836=CARTESIAN_POINT('Ctrl Pts',(-32.6223425009383,-6.67697195553557,
-36.0980619499061));
#24837=CARTESIAN_POINT('Ctrl Pts',(-32.3864006309704,-6.69622936404148,
-35.8617356014171));
#24838=CARTESIAN_POINT('Ctrl Pts',(-32.6060083690053,-6.53795985193926,
-35.6609320351416));
#24839=CARTESIAN_POINT('Ctrl Pts',(-32.5593650752754,-6.58104909157614,
-36.1085254356579));
#24840=CARTESIAN_POINT('Ctrl Pts',(-32.3705503505499,-6.57996991861,-35.8757369426306));
#24841=CARTESIAN_POINT('Ctrl Pts',(-32.5561766297544,-6.41511471179757,
-35.7065091093568));
#24842=CARTESIAN_POINT('Ctrl Pts',(-32.4216517252779,-6.40173475569596,
-36.1409145226018));
#24843=CARTESIAN_POINT('Ctrl Pts',(-32.3043563189527,-6.36383534698789,
-35.9348896071862));
#24844=CARTESIAN_POINT('Ctrl Pts',(-32.4313800558606,-6.19278444406334,
-35.8199269455543));
#24845=CARTESIAN_POINT('Ctrl Pts',(-32.3490446219505,-6.32050524456491,
-36.1621510538971));
#24846=CARTESIAN_POINT('Ctrl Pts',(-32.2579524400761,-6.26307762141883,
-35.9764869904755));
#24847=CARTESIAN_POINT('Ctrl Pts',(-32.3586632722149,-6.09580032219761,
-35.885741986965));
#24848=CARTESIAN_POINT('Ctrl Pts',(-32.1728567843285,-6.16373114062077,
-36.2258902003226));
#24849=CARTESIAN_POINT('Ctrl Pts',(-32.1199675885256,-6.07811517887309,
-36.0995837961962));
#24850=CARTESIAN_POINT('Ctrl Pts',(-32.1613068720281,-5.92198390397422,
-36.0628852537019));
#24851=CARTESIAN_POINT('Ctrl Pts',(-32.0704722290187,-6.09886182625026,
-36.2708256880667));
#24852=CARTESIAN_POINT('Ctrl Pts',(-32.0211351392778,-6.00005797774296,
-36.1874132622081));
#24853=CARTESIAN_POINT('Ctrl Pts',(-32.0323399058407,-5.8609798928657,-36.1777020688111));
#24854=CARTESIAN_POINT('Ctrl Pts',(-31.984476267574,-6.10268725738808,-36.3263280849565));
#24855=CARTESIAN_POINT('Ctrl Pts',(-31.9158280229635,-6.01584203958953,
-36.2800888384076));
#24856=CARTESIAN_POINT('Ctrl Pts',(-31.8955666163655,-5.89881153274382,
-36.2978988244376));
#24857=CARTESIAN_POINT('Origin',(-32.9108164063353,-7.07886995352309,-35.8053910964449));
#24858=CARTESIAN_POINT('Ctrl Pts',(-39.0316791043431,-12.5761796977906,
-38.5782243155831));
#24859=CARTESIAN_POINT('Ctrl Pts',(-39.3109914885678,-12.4966730216632,
-38.1825612826739));
#24860=CARTESIAN_POINT('Ctrl Pts',(-38.971148947661,-12.8445798972116,-38.1292868882747));
#24861=CARTESIAN_POINT('Ctrl Pts',(-39.2137986964445,-12.7679658886679,
-38.6667648301433));
#24862=CARTESIAN_POINT('Ctrl Pts',(-39.3414646993651,-12.6138199372453,
-38.3175461156564));
#24863=CARTESIAN_POINT('Ctrl Pts',(-39.1576103554185,-12.9405865508059,
-38.2051080058143));
#24864=CARTESIAN_POINT('Ctrl Pts',(-39.4489244282751,-12.9477999797135,
-38.6846342775079));
#24865=CARTESIAN_POINT('Ctrl Pts',(-39.5079883732932,-12.8036087634352,
-38.4182266108569));
#24866=CARTESIAN_POINT('Ctrl Pts',(-39.3833967701386,-13.030416913756,-38.2499881397961));
#24867=CARTESIAN_POINT('Ctrl Pts',(-39.7877827367345,-13.1418528526573,
-38.6147444629907));
#24868=CARTESIAN_POINT('Ctrl Pts',(-39.7939468272625,-13.0167291165573,
-38.4286787464956));
#24869=CARTESIAN_POINT('Ctrl Pts',(-39.6946150246688,-13.1274080636027,
-38.2623293930186));
#24870=CARTESIAN_POINT('Ctrl Pts',(-39.8900642233608,-13.1924895597097,
-38.5820003624405));
#24871=CARTESIAN_POINT('Ctrl Pts',(-39.8794472263271,-13.0721360087909,
-38.4198017475188));
#24872=CARTESIAN_POINT('Ctrl Pts',(-39.7868043174562,-13.1527155106486,
-38.2596713162932));
#24873=CARTESIAN_POINT('Ctrl Pts',(-40.1316643013097,-13.2848578326182,
-38.4643918227783));
#24874=CARTESIAN_POINT('Ctrl Pts',(-40.0814925592654,-13.1766908654357,
-38.3602649823531));
#24875=CARTESIAN_POINT('Ctrl Pts',(-39.9985161138346,-13.1988763557094,
-38.2313292757146));
#24876=CARTESIAN_POINT('Ctrl Pts',(-40.2695202623444,-13.3151873395668,
-38.3641621129247));
#24877=CARTESIAN_POINT('Ctrl Pts',(-40.2032404760251,-13.2202535090907,
-38.2959303147521));
#24878=CARTESIAN_POINT('Ctrl Pts',(-40.1140491542167,-13.2140287022007,
-38.1971624146867));
#24879=CARTESIAN_POINT('Ctrl Pts',(-40.36214506113,-13.282303056079,-38.2184712301346));
#24880=CARTESIAN_POINT('Ctrl Pts',(-40.2816124286873,-13.2034487358305,
-38.1888336787549));
#24881=CARTESIAN_POINT('Ctrl Pts',(-40.180730391081,-13.1975864244367,-38.1308214755661));
#24882=CARTESIAN_POINT('Ctrl Pts',(-40.1126065460396,-13.2044045823054,
-38.1801853354021));
#24883=CARTESIAN_POINT('Ctrl Pts',(-40.1003695133337,-13.2044045823054,
-38.1867765902176));
#24884=CARTESIAN_POINT('Ctrl Pts',(-40.0878695495467,-13.2039200465849,
-38.19269233339));
#24885=CARTESIAN_POINT('Ctrl Pts',(-40.0751776324174,-13.2030865921358,
-38.1980323342018));
#24886=CARTESIAN_POINT('Ctrl Pts',(-40.0619624470289,-13.2022187756393,
-38.2035924950493));
#24887=CARTESIAN_POINT('Ctrl Pts',(-40.048538896247,-13.2009724747263,-38.2085292430206));
#24888=CARTESIAN_POINT('Ctrl Pts',(-40.034981169135,-13.199446062585,-38.2129732000915));
#24889=CARTESIAN_POINT('Ctrl Pts',(-40.0206856861494,-13.1978365893588,
-38.2176589790698));
#24890=CARTESIAN_POINT('Ctrl Pts',(-40.0062407990922,-13.1959155151287,
-38.2217975674052));
#24891=CARTESIAN_POINT('Ctrl Pts',(-39.9917308687064,-13.1937414656795,
-38.2255500088239));
#24892=CARTESIAN_POINT('Ctrl Pts',(-39.9884831597464,-13.1932548554968,
-38.2263899051772));
#24893=CARTESIAN_POINT('Ctrl Pts',(-39.985232189899,-13.1927553638524,-38.2272104632462));
#24894=CARTESIAN_POINT('Ctrl Pts',(-39.9819789051098,-13.1922433006301,
-38.2280134889338));
#24895=CARTESIAN_POINT('Ctrl Pts',(-39.9634767074475,-13.1893310763501,
-38.2325804853579));
#24896=CARTESIAN_POINT('Ctrl Pts',(-39.9449286065895,-13.1860397456251,
-38.2365036772376));
#24897=CARTESIAN_POINT('Ctrl Pts',(-39.9263423823089,-13.1824628010599,
-38.2398884352376));
#24898=CARTESIAN_POINT('Ctrl Pts',(-39.9067872179013,-13.1786993826273,
-38.2434496480031));
#24899=CARTESIAN_POINT('Ctrl Pts',(-39.8871896035564,-13.1746195596086,
-38.2464155761614));
#24900=CARTESIAN_POINT('Ctrl Pts',(-39.8675581906585,-13.1702746943005,
-38.2489101863332));
#24901=CARTESIAN_POINT('Ctrl Pts',(-39.8606574942543,-13.1687474177584,
-38.2497870741829));
#24902=CARTESIAN_POINT('Ctrl Pts',(-39.8537526355299,-13.1671869117775,
-38.2506056832564));
#24903=CARTESIAN_POINT('Ctrl Pts',(-39.846844060365,-13.1655939279677,-38.2513711852016));
#24904=CARTESIAN_POINT('Ctrl Pts',(-39.8208523950992,-13.1596007526788,
-38.2542511814158));
#24905=CARTESIAN_POINT('Ctrl Pts',(-39.7949454183915,-13.1531817886309,
-38.2563668768381));
#24906=CARTESIAN_POINT('Ctrl Pts',(-39.7691247502535,-13.1464435609449,
-38.2578143352514));
#24907=CARTESIAN_POINT('Ctrl Pts',(-39.7424132520525,-13.1394728599642,
-38.2593117319337));
#24908=CARTESIAN_POINT('Ctrl Pts',(-39.7157938410967,-13.1321600180536,
-38.2600948344691));
#24909=CARTESIAN_POINT('Ctrl Pts',(-39.6892696413194,-13.1245659628583,
-38.2602659618575));
#24910=CARTESIAN_POINT('Ctrl Pts',(-39.6616326372886,-13.1166533043878,
-38.2604442687758));
#24911=CARTESIAN_POINT('Ctrl Pts',(-39.6340987346077,-13.1084348255795,
-38.259958981435));
#24912=CARTESIAN_POINT('Ctrl Pts',(-39.6066771721502,-13.0999262547332,
-38.2589085438143));
#24913=CARTESIAN_POINT('Ctrl Pts',(-39.5972925130951,-13.0970143113834,
-38.2585490457389));
#24914=CARTESIAN_POINT('Ctrl Pts',(-39.587921077564,-13.094067983939,-38.2581231550883));
#24915=CARTESIAN_POINT('Ctrl Pts',(-39.5785634617679,-13.0910867263844,
-38.2576341329803));
#24916=CARTESIAN_POINT('Ctrl Pts',(-39.5440886722257,-13.0801033488869,
-38.2558325058752));
#24917=CARTESIAN_POINT('Ctrl Pts',(-39.5097942337352,-13.0686901791307,
-38.2531377665943));
#24918=CARTESIAN_POINT('Ctrl Pts',(-39.4757046982075,-13.0568974025755,
-38.2496165062848));
#24919=CARTESIAN_POINT('Ctrl Pts',(-39.4405664062734,-13.0447418240704,
-38.2459869152442));
#24920=CARTESIAN_POINT('Ctrl Pts',(-39.4056455162936,-13.0321818870426,
-38.2414800828879));
#24921=CARTESIAN_POINT('Ctrl Pts',(-39.3709807148931,-13.0192318837648,
-38.2361331579378));
#24922=CARTESIAN_POINT('Ctrl Pts',(-39.3367760709274,-13.0064537851295,
-38.2308572106702));
#24923=CARTESIAN_POINT('Ctrl Pts',(-39.3028206159918,-12.9932945861615,
-38.2247637684813));
#24924=CARTESIAN_POINT('Ctrl Pts',(-39.2691660449372,-12.9797471343051,
-38.2178444611905));
#24925=CARTESIAN_POINT('Ctrl Pts',(-39.2348323379837,-12.9659263002422,
-38.2107855250221));
#24926=CARTESIAN_POINT('Ctrl Pts',(-39.2008115903465,-12.9516999140197,
-38.2028676339683));
#24927=CARTESIAN_POINT('Ctrl Pts',(-39.1671765836779,-12.9370593466235,
-38.1940276365451));
#24928=CARTESIAN_POINT('Ctrl Pts',(-39.1363330539154,-12.923633846796,-38.1859212988146));
#24929=CARTESIAN_POINT('Ctrl Pts',(-39.1058140642328,-12.9098590019422,
-38.1770390451456));
#24930=CARTESIAN_POINT('Ctrl Pts',(-39.0756901950279,-12.8957449858576,
-38.1672883346991));
#24931=CARTESIAN_POINT('Ctrl Pts',(-39.0729638506097,-12.894467604499,-38.1664058519471));
#24932=CARTESIAN_POINT('Ctrl Pts',(-39.0702407521924,-12.8931874634454,
-38.1655162266651));
#24933=CARTESIAN_POINT('Ctrl Pts',(-39.0675209577957,-12.8919045823054,
-38.1646193729747));
#24934=CARTESIAN_POINT('Origin',(-40.1126065460396,-13.5169045823054,-38.1801853354021));
#24935=CARTESIAN_POINT('Ctrl Pts',(-42.7963830377277,-14.6563598281152,
-37.572732204214));
#24936=CARTESIAN_POINT('Ctrl Pts',(-42.8482224231091,-14.7669045823027,
-37.64926336932));
#24937=CARTESIAN_POINT('Ctrl Pts',(-42.9289078842538,-14.7669045823054,
-37.769437584449));
#24938=CARTESIAN_POINT('Ctrl Pts',(-42.858102552525,-14.6732979129424,-37.5515771497065));
#24939=CARTESIAN_POINT('Ctrl Pts',(-42.9221643671718,-14.7669045823064,
-37.6214949477829));
#24940=CARTESIAN_POINT('Ctrl Pts',(-43.0171700719925,-14.7669045823054,
-37.7163455316033));
#24941=CARTESIAN_POINT('Ctrl Pts',(-42.9046371348531,-14.6836226395017,
-37.511596293802));
#24942=CARTESIAN_POINT('Ctrl Pts',(-42.9828541398335,-14.7669045823055,
-37.5612377434468));
#24943=CARTESIAN_POINT('Ctrl Pts',(-43.0894948610397,-14.7669045823054,
-37.6289001478671));
#24944=CARTESIAN_POINT('Ctrl Pts',(-42.930578525807,-14.6837071744118,-37.4337545567665));
#24945=CARTESIAN_POINT('Ctrl Pts',(-43.0197879756039,-14.7669045823053,
-37.4502266440492));
#24946=CARTESIAN_POINT('Ctrl Pts',(-43.1413666883037,-14.7669045823054,
-37.4726705102553));
#24947=CARTESIAN_POINT('Ctrl Pts',(-42.9305937454166,-14.6805726740673,
-37.4030029435815));
#24948=CARTESIAN_POINT('Ctrl Pts',(-43.0218035062137,-14.7669045823054,
-37.4068468927024));
#24949=CARTESIAN_POINT('Ctrl Pts',(-43.1478444705321,-14.7669045823054,
-37.4130984790331));
#24950=CARTESIAN_POINT('Ctrl Pts',(-42.9062631519066,-14.6635276241068,
-37.3097719517883));
#24951=CARTESIAN_POINT('Ctrl Pts',(-42.9975785139956,-14.7669045823054,
-37.2792440170877));
#24952=CARTESIAN_POINT('Ctrl Pts',(-43.134092223999,-14.7669045823054,-37.2376557184966));
#24953=CARTESIAN_POINT('Ctrl Pts',(-42.8588599809403,-14.6424796666932,
-37.2472449190099));
#24954=CARTESIAN_POINT('Ctrl Pts',(-42.9410778224509,-14.7669045823058,
-37.1988871414035));
#24955=CARTESIAN_POINT('Ctrl Pts',(-43.082276268341,-14.7669045823054,-37.1265846080327));
#24956=CARTESIAN_POINT('Ctrl Pts',(-42.6561292830181,-14.560778522968,-37.0605332449033));
#24957=CARTESIAN_POINT('Ctrl Pts',(-42.6929533769163,-14.7669045823044,
-36.9765311644006));
#24958=CARTESIAN_POINT('Ctrl Pts',(-42.8437843379004,-14.7669045823054,
-36.808037040221));
#24959=CARTESIAN_POINT('Ctrl Pts',(-42.4452340977281,-14.485990546607,-36.9651610952557));
#24960=CARTESIAN_POINT('Ctrl Pts',(-42.4208805578758,-14.7669045823061,
-36.9206538390427));
#24961=CARTESIAN_POINT('Ctrl Pts',(-42.5749664504047,-14.7669045823054,
-36.6685486138914));
#24962=CARTESIAN_POINT('Ctrl Pts',(-42.2429004856065,-14.4183787521208,
-36.9115565886974));
#24963=CARTESIAN_POINT('Ctrl Pts',(-42.23469723594,-14.7669045823051,-36.9519162686243));
#24964=CARTESIAN_POINT('Ctrl Pts',(-42.3098537353251,-14.7669045823054,
-36.6082395787205));
#24965=CARTESIAN_POINT('Ctrl Pts',(-42.3443728681154,-14.4544045238107,
-36.9418020085688));
#24966=CARTESIAN_POINT('Ctrl Pts',(-42.3737106494897,-14.4643868520267,
-36.9514761580288));
#24967=CARTESIAN_POINT('Ctrl Pts',(-42.4027641035859,-14.4744011867389,
-36.9619828372566));
#24968=CARTESIAN_POINT('Ctrl Pts',(-42.4314670014265,-14.4844099197098,
-36.9733072590746));
#24969=CARTESIAN_POINT('Ctrl Pts',(-42.4596712580304,-14.4942447759171,
-36.9844349473177));
#24970=CARTESIAN_POINT('Ctrl Pts',(-42.4875385896839,-14.5040728389242,
-36.996351552873));
#24971=CARTESIAN_POINT('Ctrl Pts',(-42.5150050555123,-14.5138432176011,
-37.0090909967157));
#24972=CARTESIAN_POINT('Ctrl Pts',(-42.5401900236358,-14.5228020212953,
-37.0207722406403));
#24973=CARTESIAN_POINT('Ctrl Pts',(-42.5650389656366,-14.5317110776815,
-37.0331459059695));
#24974=CARTESIAN_POINT('Ctrl Pts',(-42.5894839867309,-14.5405368969068,
-37.0462776461334));
#24975=CARTESIAN_POINT('Ctrl Pts',(-42.6126265157218,-14.5488924543229,
-37.0587096942085));
#24976=CARTESIAN_POINT('Ctrl Pts',(-42.6354077244154,-14.5571724059617,
-37.0718219993755));
#24977=CARTESIAN_POINT('Ctrl Pts',(-42.6577407274503,-14.5653692837009,
-37.0856974585248));
#24978=CARTESIAN_POINT('Ctrl Pts',(-42.6784000406813,-14.5729518673985,
-37.0985330568696));
#24979=CARTESIAN_POINT('Ctrl Pts',(-42.6986760027707,-14.5804628051684,
-37.1120227658321));
#24980=CARTESIAN_POINT('Ctrl Pts',(-42.7184682792969,-14.587925101972,-37.1262428650811));
#24981=CARTESIAN_POINT('Ctrl Pts',(-42.728622039289,-14.5917533816866,-37.1335380074387));
#24982=CARTESIAN_POINT('Ctrl Pts',(-42.7386479513117,-14.5955693937988,
-37.1410254719861));
#24983=CARTESIAN_POINT('Ctrl Pts',(-42.7485287260783,-14.5993802185557,
-37.1487152165534));
#24984=CARTESIAN_POINT('Ctrl Pts',(-42.7616540438129,-14.604442401122,-37.1589300370636));
#24985=CARTESIAN_POINT('Ctrl Pts',(-42.7745538904303,-14.6095732512804,
-37.1694686330813));
#24986=CARTESIAN_POINT('Ctrl Pts',(-42.7871269159706,-14.6146451518332,
-37.1804202089125));
#24987=CARTESIAN_POINT('Ctrl Pts',(-42.7989080093126,-14.6193975905872,
-37.1906819821584));
#24988=CARTESIAN_POINT('Ctrl Pts',(-42.8104022403622,-14.6240978916553,
-37.2013072124028));
#24989=CARTESIAN_POINT('Ctrl Pts',(-42.8214944105973,-14.6286695523063,
-37.2123820369564));
#24990=CARTESIAN_POINT('Ctrl Pts',(-42.8321400773418,-14.6330571856305,
-37.2230110562515));
#24991=CARTESIAN_POINT('Ctrl Pts',(-42.8424154792447,-14.6373259480378,
-37.2340550798162));
#24992=CARTESIAN_POINT('Ctrl Pts',(-42.8521871210052,-14.6414408657886,
-37.2455902226561));
#24993=CARTESIAN_POINT('Ctrl Pts',(-42.8616851363247,-14.6454405572215,
-37.2568023573302));
#24994=CARTESIAN_POINT('Ctrl Pts',(-42.8707071510317,-14.6492945993135,
-37.2684795517426));
#24995=CARTESIAN_POINT('Ctrl Pts',(-42.8790997295204,-14.6530074411931,
-37.2806776882817));
#24996=CARTESIAN_POINT('Ctrl Pts',(-42.8869655548277,-14.6564872496522,
-37.2921102189659));
#24997=CARTESIAN_POINT('Ctrl Pts',(-42.8942780129941,-14.6598432010016,
-37.3040012433705));
#24998=CARTESIAN_POINT('Ctrl Pts',(-42.9008873385451,-14.6631120254244,
-37.3163705916822));
#24999=CARTESIAN_POINT('Ctrl Pts',(-42.9013299473147,-14.663330929811,-37.317198933696));
#25000=CARTESIAN_POINT('Ctrl Pts',(-42.9017693952537,-14.6635494557761,
-37.3180294074842));
#25001=CARTESIAN_POINT('Ctrl Pts',(-42.9022056342624,-14.6637676196428,
-37.3188620128984));
#25002=CARTESIAN_POINT('Ctrl Pts',(-42.9080335625763,-14.6666821764586,
-37.3299851920969));
#25003=CARTESIAN_POINT('Ctrl Pts',(-42.9132544517344,-14.6694736866497,
-37.3415545631474));
#25004=CARTESIAN_POINT('Ctrl Pts',(-42.9175148584672,-14.6719975663698,
-37.3534879002389));
#25005=CARTESIAN_POINT('Ctrl Pts',(-42.921639999208,-14.6744413140473,-37.3650423592606));
#25006=CARTESIAN_POINT('Ctrl Pts',(-42.9248639641694,-14.6766346712663,
-37.3769386888275));
#25007=CARTESIAN_POINT('Ctrl Pts',(-42.926860530905,-14.6784666962725,-37.3890588177022));
#25008=CARTESIAN_POINT('Ctrl Pts',(-42.9287803512802,-14.6802282997652,
-37.4007130589293));
#25009=CARTESIAN_POINT('Ctrl Pts',(-42.9295645080495,-14.6816565741043,
-37.4125744533077));
#25010=CARTESIAN_POINT('Ctrl Pts',(-42.9289290029343,-14.6826626743678,
-37.4244909451429));
#25011=CARTESIAN_POINT('Ctrl Pts',(-42.9287732308293,-14.6829092850591,
-37.4274118610765));
#25012=CARTESIAN_POINT('Ctrl Pts',(-42.9285322257575,-14.6831305465446,
-37.4303358517388));
#25013=CARTESIAN_POINT('Ctrl Pts',(-42.9282019541629,-14.6833251552392,
-37.4332602126666));
#25014=CARTESIAN_POINT('Ctrl Pts',(-42.9271345709019,-14.6839540984074,
-37.4427112643312));
#25015=CARTESIAN_POINT('Ctrl Pts',(-42.925040039123,-14.6841943737355,-37.4519923607426));
#25016=CARTESIAN_POINT('Ctrl Pts',(-42.9220297208895,-14.6841331258666,
-37.4609600273967));
#25017=CARTESIAN_POINT('Ctrl Pts',(-42.9189684247695,-14.6840708408026,
-37.4700795559664));
#25018=CARTESIAN_POINT('Ctrl Pts',(-42.9149605958391,-14.6836965195603,
-37.4788739643186));
#25019=CARTESIAN_POINT('Ctrl Pts',(-42.9101526120369,-14.6830632794738,
-37.4872169821896));
#25020=CARTESIAN_POINT('Ctrl Pts',(-42.9052560717732,-14.6824183759742,
-37.495713666997));
#25021=CARTESIAN_POINT('Ctrl Pts',(-42.8995304118283,-14.6815043446903,
-37.5037415250777));
#25022=CARTESIAN_POINT('Ctrl Pts',(-42.8931501145775,-14.6803438374132,
-37.5112053503256));
#25023=CARTESIAN_POINT('Ctrl Pts',(-42.8865120039902,-14.67913643667,-37.5189707718181));
#25024=CARTESIAN_POINT('Ctrl Pts',(-42.8791661545134,-14.6776614503338,
-37.5261253320786));
#25025=CARTESIAN_POINT('Ctrl Pts',(-42.871317367589,-14.675919147448,-37.5326108693554));
#25026=CARTESIAN_POINT('Ctrl Pts',(-42.8705136526921,-14.6757407358287,
-37.533274987642));
#25027=CARTESIAN_POINT('Ctrl Pts',(-42.8697046643841,-14.6755595065434,
-37.5339321330287));
#25028=CARTESIAN_POINT('Ctrl Pts',(-42.8688906217797,-14.6753754510085,
-37.5345822715346));
#25029=CARTESIAN_POINT('Origin',(0.0835265683620477,-14.4544045823054,0.0824317919394229));
#25030=CARTESIAN_POINT('Origin',(15.4714058027788,-14.4544045823054,5.15659338881741));
#25031=CARTESIAN_POINT('Origin',(29.1374429791686,-14.7669045823054,-38.2827290469501));
#25032=CARTESIAN_POINT('Origin',(29.1374429791686,-11.3294045823054,-38.2827290469501));
#25033=CARTESIAN_POINT('Origin',(0.0835265683620477,-12.8919045823054,0.0824317919394229));
#25034=CARTESIAN_POINT('Ctrl Pts',(34.7488729746945,-13.2044045823054,-34.1940362076806));
#25035=CARTESIAN_POINT('Ctrl Pts',(34.7490067374541,-13.2044045823054,-34.1691350833616));
#25036=CARTESIAN_POINT('Ctrl Pts',(34.749145716179,-13.2030022087213,-34.1445008166353));
#25037=CARTESIAN_POINT('Ctrl Pts',(34.7492919647972,-13.2001447338014,-34.1200426226309));
#25038=CARTESIAN_POINT('Ctrl Pts',(34.7494355478613,-13.1973393397408,-34.0960302081331));
#25039=CARTESIAN_POINT('Ctrl Pts',(34.749586164608,-13.1931314656534,-34.0721874632317));
#25040=CARTESIAN_POINT('Ctrl Pts',(34.7497462547033,-13.187422036285,-34.0484389068724));
#25041=CARTESIAN_POINT('Ctrl Pts',(34.7497860634588,-13.1860023027459,-34.042533479238));
#25042=CARTESIAN_POINT('Ctrl Pts',(34.7498264593483,-13.1844894768732,-34.0366339287836));
#25043=CARTESIAN_POINT('Ctrl Pts',(34.7498674817982,-13.1828815404475,-34.0307392028842));
#25044=CARTESIAN_POINT('Ctrl Pts',(34.7500209276666,-13.1768669995856,-34.0086897802678));
#25045=CARTESIAN_POINT('Ctrl Pts',(34.7501794108001,-13.1696750914266,-33.9872331665337));
#25046=CARTESIAN_POINT('Ctrl Pts',(34.7503432418475,-13.1611455958502,-33.9663916514025));
#25047=CARTESIAN_POINT('Ctrl Pts',(34.7505070728949,-13.1526161002738,-33.9455501362714));
#25048=CARTESIAN_POINT('Ctrl Pts',(34.7506762764637,-13.1427495299604,-33.9253233735306));
#25049=CARTESIAN_POINT('Ctrl Pts',(34.7508505176857,-13.1313389816383,-33.9057667392102));
#25050=CARTESIAN_POINT('Ctrl Pts',(34.7509093060885,-13.1274891009823,-33.8991683965153));
#25051=CARTESIAN_POINT('Ctrl Pts',(34.7509669071891,-13.1234784566375,-33.8926739099407));
#25052=CARTESIAN_POINT('Ctrl Pts',(34.7510237261945,-13.1192883941035,-33.8862654556767));
#25053=CARTESIAN_POINT('Ctrl Pts',(34.7511184667809,-13.1123018412986,-33.8755799339813));
#25054=CARTESIAN_POINT('Ctrl Pts',(34.7512095940135,-13.1049166125579,-33.8652988342736));
#25055=CARTESIAN_POINT('Ctrl Pts',(34.7512983550753,-13.0970443878841,-33.8553996398422));
#25056=CARTESIAN_POINT('Ctrl Pts',(34.7513313938886,-13.0941141732644,-33.8517149426379));
#25057=CARTESIAN_POINT('Ctrl Pts',(34.7513641008242,-13.0911162306688,-33.848083590736));
#25058=CARTESIAN_POINT('Ctrl Pts',(34.7513965235091,-13.088045086031,-33.8445060658395));
#25059=CARTESIAN_POINT('Ctrl Pts',(34.751482407832,-13.0799099430592,-33.8350295741887));
#25060=CARTESIAN_POINT('Ctrl Pts',(34.7515659307597,-13.0712950250751,-33.8259697968496));
#25061=CARTESIAN_POINT('Ctrl Pts',(34.7516435388463,-13.0621639241565,-33.81741373038));
#25062=CARTESIAN_POINT('Ctrl Pts',(34.7517211469329,-13.053032823238,-33.8088576639104));
#25063=CARTESIAN_POINT('Ctrl Pts',(34.7517917066434,-13.0433849467636,-33.8008061504376));
#25064=CARTESIAN_POINT('Ctrl Pts',(34.7518655550335,-13.0331862397833,-33.7933487163968));
#25065=CARTESIAN_POINT('Ctrl Pts',(34.7519013947382,-13.0282366579926,-33.7897295144916));
#25066=CARTESIAN_POINT('Ctrl Pts',(34.7519360091844,-13.0231465710756,-33.7862448865609));
#25067=CARTESIAN_POINT('Ctrl Pts',(34.7519691779118,-13.0179182754031,-33.7829138711544));
#25068=CARTESIAN_POINT('Ctrl Pts',(34.7520437167405,-13.0061689239916,-33.7754282060314));
#25069=CARTESIAN_POINT('Ctrl Pts',(34.7521095322082,-12.9939049176378,-33.7688513062993));
#25070=CARTESIAN_POINT('Ctrl Pts',(34.7521646053494,-12.9812267133693,-33.7633720134592));
#25071=CARTESIAN_POINT('Ctrl Pts',(34.7522184025857,-12.9688422309163,-33.7580196619277));
#25072=CARTESIAN_POINT('Ctrl Pts',(34.7522619420059,-12.9560629035372,-33.7537150431855));
#25073=CARTESIAN_POINT('Ctrl Pts',(34.7522936929901,-12.943000609226,-33.7505884810027));
#25074=CARTESIAN_POINT('Ctrl Pts',(34.7523245873487,-12.9302907290149,-33.7475462718877));
#25075=CARTESIAN_POINT('Ctrl Pts',(34.7523443148449,-12.9173133257173,-33.7456196262415));
#25076=CARTESIAN_POINT('Ctrl Pts',(34.7523518990928,-12.9041833323999,-33.7448804669025));
#25077=CARTESIAN_POINT('Ctrl Pts',(34.7523542554978,-12.9001038795416,-33.7446508121261));
#25078=CARTESIAN_POINT('Ctrl Pts',(34.7523554432478,-12.8960097626116,-33.7445354190578));
#25079=CARTESIAN_POINT('Ctrl Pts',(34.7523554432478,-12.8919045823054,-33.7445354190578));
#25080=CARTESIAN_POINT('Origin',(21.1549759309662,-13.5169045823054,7.03075374829756));
#25081=CARTESIAN_POINT('Origin',(34.7488729746945,-13.5169045823054,-34.1940362076806));
#25082=CARTESIAN_POINT('Ctrl Pts',(37.2673094055704,-14.9232028613467,-42.8293153229833));
#25083=CARTESIAN_POINT('Ctrl Pts',(37.3552899674095,-14.6181128259927,-43.0961247721324));
#25084=CARTESIAN_POINT('Ctrl Pts',(37.7096412180108,-14.7022319922259,-42.8977137135733));
#25085=CARTESIAN_POINT('Ctrl Pts',(37.1076947869938,-14.453862129984,-42.345268761239));
#25086=CARTESIAN_POINT('Ctrl Pts',(37.1955707280038,-14.1470746072355,-42.6117609377653));
#25087=CARTESIAN_POINT('Ctrl Pts',(37.550607296294,-14.2328912595893,-42.4131587905921));
#25088=CARTESIAN_POINT('Ctrl Pts',(36.9479116082779,-13.9850662226643,-41.8607110247875));
#25089=CARTESIAN_POINT('Ctrl Pts',(37.0359221508734,-13.6772499732423,-42.1276113934436));
#25090=CARTESIAN_POINT('Ctrl Pts',(37.3914171317387,-13.7640953522116,-41.9280765487537));
#25091=CARTESIAN_POINT('Ctrl Pts',(36.7879602992159,-13.5169045823054,-41.3756434170181));
#25092=CARTESIAN_POINT('Ctrl Pts',(36.8763881414603,-13.2088427643879,-41.6438092866772));
#25093=CARTESIAN_POINT('Ctrl Pts',(37.2320718162657,-13.2959337131846,-41.4424668154812));
#25094=CARTESIAN_POINT('Ctrl Pts',(37.7005406318363,-14.6753754510085,-42.8699853982021));
#25095=CARTESIAN_POINT('Ctrl Pts',(37.6942941487563,-14.6771438430879,-42.8778066598394));
#25096=CARTESIAN_POINT('Ctrl Pts',(37.6873971139536,-14.6786525232815,-42.8851614290357));
#25097=CARTESIAN_POINT('Ctrl Pts',(37.6798997497709,-14.6799030932779,-42.8918545698488));
#25098=CARTESIAN_POINT('Ctrl Pts',(37.6726072486374,-14.681119491854,-42.898364822756));
#25099=CARTESIAN_POINT('Ctrl Pts',(37.6647469214214,-14.6820924420367,-42.9042483364246));
#25100=CARTESIAN_POINT('Ctrl Pts',(37.6564075056867,-14.6828029998435,-42.9093313166295));
#25101=CARTESIAN_POINT('Ctrl Pts',(37.648225521828,-14.6835001437071,-42.914318340099));
#25102=CARTESIAN_POINT('Ctrl Pts',(37.6395829273532,-14.6839452832804,-42.9185340273081));
#25103=CARTESIAN_POINT('Ctrl Pts',(37.6305998593746,-14.6840907481788,-42.921831148677));
#25104=CARTESIAN_POINT('Ctrl Pts',(37.6217179108511,-14.6842345756264,-42.9250911554302));
#25105=CARTESIAN_POINT('Ctrl Pts',(37.6125039938892,-14.6840857258449,-42.9274525885272));
#25106=CARTESIAN_POINT('Ctrl Pts',(37.6030993276363,-14.6835622048232,-42.9287997028454));
#25107=CARTESIAN_POINT('Ctrl Pts',(37.6018091775119,-14.6834903872071,-42.9289845025669));
#25108=CARTESIAN_POINT('Ctrl Pts',(37.6005154638893,-14.6834114599928,-42.9291502622653));
#25109=CARTESIAN_POINT('Ctrl Pts',(37.5992185729682,-14.6833251552392,-42.9292967305854));
#25110=CARTESIAN_POINT('Ctrl Pts',(37.5871874867119,-14.682524517408,-42.9306554978992));
#25111=CARTESIAN_POINT('Ctrl Pts',(37.5751667988684,-14.6812727698323,-42.9305019908788));
#25112=CARTESIAN_POINT('Ctrl Pts',(37.5633248420647,-14.679660389819,-42.9291239695466));
#25113=CARTESIAN_POINT('Ctrl Pts',(37.5511660377452,-14.6780048684052,-42.9277090773963));
#25114=CARTESIAN_POINT('Ctrl Pts',(37.5391953985779,-14.6759682812647,-42.9250042042342));
#25115=CARTESIAN_POINT('Ctrl Pts',(37.5275408602363,-14.6736566051529,-42.921330936022));
#25116=CARTESIAN_POINT('Ctrl Pts',(37.5153677286545,-14.6712420661416,-42.9174942180009));
#25117=CARTESIAN_POINT('Ctrl Pts',(37.5035388927731,-14.6685267231679,-42.9126018607288));
#25118=CARTESIAN_POINT('Ctrl Pts',(37.4921479858276,-14.6656525103353,-42.9070169658405));
#25119=CARTESIAN_POINT('Ctrl Pts',(37.4896849080212,-14.665031013744,-42.9058093332335));
#25120=CARTESIAN_POINT('Ctrl Pts',(37.4872421403176,-14.6644021844318,-42.9045692821918));
#25121=CARTESIAN_POINT('Ctrl Pts',(37.4848203732001,-14.663767619643,-42.9033004106846));
#25122=CARTESIAN_POINT('Ctrl Pts',(37.4722830144273,-14.6604825116887,-42.8967315307926));
#25123=CARTESIAN_POINT('Ctrl Pts',(37.4602321609586,-14.6571124630586,-42.8894367548376));
#25124=CARTESIAN_POINT('Ctrl Pts',(37.4486497152673,-14.6536176840784,-42.8815709768372));
#25125=CARTESIAN_POINT('Ctrl Pts',(37.4365571014837,-14.6499689717431,-42.8733587375569));
#25126=CARTESIAN_POINT('Ctrl Pts',(37.4249739677492,-14.6461842219902,-42.8645245242179));
#25127=CARTESIAN_POINT('Ctrl Pts',(37.4138479847458,-14.6422568272874,-42.8552175604044));
#25128=CARTESIAN_POINT('Ctrl Pts',(37.4019517120116,-14.6380575256611,-42.8452662437594));
#25129=CARTESIAN_POINT('Ctrl Pts',(37.3905769669797,-14.6336952044168,-42.8347747585113));
#25130=CARTESIAN_POINT('Ctrl Pts',(37.3796421032092,-14.6292054571928,-42.8238889904825));
#25131=CARTESIAN_POINT('Ctrl Pts',(37.367941220124,-14.6244011899927,-42.8122406424399));
#25132=CARTESIAN_POINT('Ctrl Pts',(37.3567428099825,-14.6194513461054,-42.8001409114864));
#25133=CARTESIAN_POINT('Ctrl Pts',(37.3459461922268,-14.6144447802764,-42.7877248805979));
#25134=CARTESIAN_POINT('Ctrl Pts',(37.3351495744711,-14.6094382144474,-42.7753088497095));
#25135=CARTESIAN_POINT('Ctrl Pts',(37.3247539006079,-14.6043757482481,-42.7625760014678));
#25136=CARTESIAN_POINT('Ctrl Pts',(37.314673576856,-14.5993802185558,-42.7496235025004));
#25137=CARTESIAN_POINT('Ctrl Pts',(37.2996591606931,-14.591939489111,-42.7303310457666));
#25138=CARTESIAN_POINT('Ctrl Pts',(37.2854163404317,-14.5844764296232,-42.7104876092804));
#25139=CARTESIAN_POINT('Ctrl Pts',(37.271869192699,-14.5769485180956,-42.6902126068496));
#25140=CARTESIAN_POINT('Ctrl Pts',(37.2575210202359,-14.5689754912257,-42.6687387706364));
#25141=CARTESIAN_POINT('Ctrl Pts',(37.2439518403639,-14.5609303686272,-42.6467806455568));
#25142=CARTESIAN_POINT('Ctrl Pts',(37.231074974359,-14.5528049305378,-42.6244379172628));
#25143=CARTESIAN_POINT('Ctrl Pts',(37.216955372675,-14.5438953131443,-42.5999389107556));
#25144=CARTESIAN_POINT('Ctrl Pts',(37.2036667293897,-14.5348900830946,-42.5749770310613));
#25145=CARTESIAN_POINT('Ctrl Pts',(37.1911225229489,-14.5258150805519,-42.5496389875043));
#25146=CARTESIAN_POINT('Ctrl Pts',(37.1780215140351,-14.5163372638589,-42.5231762585891));
#25147=CARTESIAN_POINT('Ctrl Pts',(37.1657318069736,-14.5067848826414,-42.4963019660966));
#25148=CARTESIAN_POINT('Ctrl Pts',(37.1542009804941,-14.4972049637149,-42.4690826148663));
#25149=CARTESIAN_POINT('Ctrl Pts',(37.1421820564311,-14.4872195287323,-42.4407110739313));
#25150=CARTESIAN_POINT('Ctrl Pts',(37.1309877266823,-14.4772057790309,-42.4119630555272));
#25151=CARTESIAN_POINT('Ctrl Pts',(37.1206126001907,-14.4672106594482,-42.3829021690193));
#25152=CARTESIAN_POINT('Ctrl Pts',(37.1161774871905,-14.4629379901138,-42.3704793503043));
#25153=CARTESIAN_POINT('Ctrl Pts',(37.1118927098178,-14.4586685042085,-42.3579993627814));
#25154=CARTESIAN_POINT('Ctrl Pts',(37.1077603688698,-14.4544045238129,-42.3454676445359));
#25155=CARTESIAN_POINT('Origin',(0.0835265683620477,-14.4544045823054,0.0824317919394229));
#25156=CARTESIAN_POINT('Origin',(37.8461247099825,-14.4544045823054,-43.0362183703681));
#25157=CARTESIAN_POINT('Ctrl Pts',(48.833526568362,-14.7669045823054,29.5557152835192));
#25158=CARTESIAN_POINT('Ctrl Pts',(48.521026568362,-14.7669045823054,29.5557152835192));
#25159=CARTESIAN_POINT('Ctrl Pts',(48.521026568362,-14.4544045823054,29.5557152835192));
#25160=CARTESIAN_POINT('Ctrl Pts',(48.8335265666929,-14.7669045823054,29.7413197449171));
#25161=CARTESIAN_POINT('Ctrl Pts',(48.5569389176245,-14.7669045823054,29.7119954162173));
#25162=CARTESIAN_POINT('Ctrl Pts',(48.521026568362,-14.4924853132395,29.7214315040358));
#25163=CARTESIAN_POINT('Ctrl Pts',(48.8166857802236,-14.7669045823054,29.9249596309445));
#25164=CARTESIAN_POINT('Ctrl Pts',(48.5753407341527,-14.7669045823059,29.8840840848071));
#25165=CARTESIAN_POINT('Ctrl Pts',(48.5126061688921,-14.5302363915369,29.8851398847485));
#25166=CARTESIAN_POINT('Ctrl Pts',(48.7408780450792,-14.7669045823054,30.287020683478));
#25167=CARTESIAN_POINT('Ctrl Pts',(48.5640170046697,-14.7669045823049,30.2252857066681));
#25168=CARTESIAN_POINT('Ctrl Pts',(48.4747023121212,-14.6047976733282,30.2074413642911));
#25169=CARTESIAN_POINT('Ctrl Pts',(48.6828517369698,-14.7669045823054,30.4694825866923));
#25170=CARTESIAN_POINT('Ctrl Pts',(48.5393566233762,-14.7669045823071,30.4014929051335));
#25171=CARTESIAN_POINT('Ctrl Pts',(48.4458475996025,-14.6423413865141,30.3691656155262));
#25172=CARTESIAN_POINT('Ctrl Pts',(48.582477269951,-14.7669045823054,30.6288487842779));
#25173=CARTESIAN_POINT('Ctrl Pts',(48.472949645285,-14.7669045823054,30.5598642712766));
#25174=CARTESIAN_POINT('Ctrl Pts',(48.3955019191565,-14.6753754514262,30.5110848543364));
#25175=CARTESIAN_POINT('Origin',(48.582477269951,-14.4544045823054,30.6288487842779));
#25176=CARTESIAN_POINT('Ctrl Pts',(48.5210408433891,-6.00666333723546,0.0824317919201338));
#25177=CARTESIAN_POINT('Ctrl Pts',(48.5210403778953,-5.9853111687807,0.0824317919206602));
#25178=CARTESIAN_POINT('Ctrl Pts',(48.5206820692032,-5.96223275463527,0.0824317919312382));
#25179=CARTESIAN_POINT('Ctrl Pts',(48.5165774172042,-5.92795641804992,0.0824317919333195));
#25180=CARTESIAN_POINT('Ctrl Pts',(48.521026568362,-5.90583775506839,0.0824317919337002));
#25181=CARTESIAN_POINT('Ctrl Pts',(48.521026568362,-5.88746284406389,0.082431791939678));
#25182=CARTESIAN_POINT('Ctrl Pts',(48.5210407270156,-6.00132529512183,0.433477096794441));
#25183=CARTESIAN_POINT('Ctrl Pts',(48.5209806868545,-5.98270666392103,0.355621276196246));
#25184=CARTESIAN_POINT('Ctrl Pts',(48.520716368315,-5.96240686080378,0.33843523650393));
#25185=CARTESIAN_POINT('Ctrl Pts',(48.5165547847583,-5.92787973562316,0.360237634060305));
#25186=CARTESIAN_POINT('Ctrl Pts',(48.5210265683621,-5.90583775506839,0.39922607131656));
#25187=CARTESIAN_POINT('Ctrl Pts',(48.521026568362,-5.88746284406389,0.433719204637548));
#25188=CARTESIAN_POINT('Ctrl Pts',(48.5195832988733,-5.99973567328077,0.784574339427845));
#25189=CARTESIAN_POINT('Ctrl Pts',(48.5197866644975,-5.98152768121122,0.651206501674453));
#25190=CARTESIAN_POINT('Ctrl Pts',(48.5193523631325,-5.96239709811727,0.625439688561988));
#25191=CARTESIAN_POINT('Ctrl Pts',(48.5144416808493,-5.92723732580307,0.666464865111502));
#25192=CARTESIAN_POINT('Ctrl Pts',(48.5179089072263,-5.90562906540035,0.733256854779834));
#25193=CARTESIAN_POINT('Ctrl Pts',(48.5172052126372,-5.88746284406389,0.785006622606558));
#25194=CARTESIAN_POINT('Ctrl Pts',(48.5098524785301,-5.9982057973698,1.48689990256317));
#25195=CARTESIAN_POINT('Ctrl Pts',(48.5114206543233,-5.97907559060222,1.29386039347741));
#25196=CARTESIAN_POINT('Ctrl Pts',(48.5102621676405,-5.9609921479881,1.26166887611461));
#25197=CARTESIAN_POINT('Ctrl Pts',(48.5031898260137,-5.9251130175414,1.32614678057686));
#25198=CARTESIAN_POINT('Ctrl Pts',(48.5037480059615,-5.9049506781467,1.42281620240611));
#25199=CARTESIAN_POINT('Ctrl Pts',(48.5019179682626,-5.88746284406389,1.48749857171671));
#25200=CARTESIAN_POINT('Ctrl Pts',(48.5015790863291,-5.99826554329988,1.83812822306509));
#25201=CARTESIAN_POINT('Ctrl Pts',(48.5041223947854,-5.97774718230277,1.64093757425052));
#25202=CARTESIAN_POINT('Ctrl Pts',(48.5024096539615,-5.95954166014521,1.6109000900691));
#25203=CARTESIAN_POINT('Ctrl Pts',(48.4939878358359,-5.9236034688997,1.67960165287408));
#25204=CARTESIAN_POINT('Ctrl Pts',(48.4927046623486,-5.90448098056108,1.77834069986374));
#25205=CARTESIAN_POINT('Ctrl Pts',(48.4904520792406,-5.88746284406389,1.83870311340082));
#25206=CARTESIAN_POINT('Ctrl Pts',(48.4743149973473,-5.99418693015721,2.54074314428776));
#25207=CARTESIAN_POINT('Ctrl Pts',(48.4757865146801,-5.97194742955365,2.39327412296866));
#25208=CARTESIAN_POINT('Ctrl Pts',(48.4732866422927,-5.9541339311854,2.37176704438306));
#25209=CARTESIAN_POINT('Ctrl Pts',(48.4648102886654,-5.91998502842413,2.42404521972768));
#25210=CARTESIAN_POINT('Ctrl Pts',(48.4621240605451,-5.90343694889074,2.49783047365958));
#25211=CARTESIAN_POINT('Ctrl Pts',(48.4598703086855,-5.88746284406389,2.54094611738039));
#25212=CARTESIAN_POINT('Ctrl Pts',(48.4566988310663,-5.99381953117216,2.89171006783013));
#25213=CARTESIAN_POINT('Ctrl Pts',(48.457044461769,-5.97081802552582,2.7688356338994));
#25214=CARTESIAN_POINT('Ctrl Pts',(48.4539681826447,-5.95257589046842,2.75380781345132));
#25215=CARTESIAN_POINT('Ctrl Pts',(48.4456390893095,-5.91860436677926,2.80028584056467));
#25216=CARTESIAN_POINT('Ctrl Pts',(48.4425870086017,-5.90286261480602,2.86179168812718));
#25217=CARTESIAN_POINT('Ctrl Pts',(48.4407544264066,-5.88746284406389,2.89198459022076));
#25218=CARTESIAN_POINT('Ctrl Pts',(48.4142685323911,-5.99717808806687,3.5932676328871));
#25219=CARTESIAN_POINT('Ctrl Pts',(48.4107714342326,-5.97321241327166,3.5256134946276));
#25220=CARTESIAN_POINT('Ctrl Pts',(48.4062756536138,-5.95314193699471,3.52141678729507));
#25221=CARTESIAN_POINT('Ctrl Pts',(48.3983980635879,-5.91737158402251,3.55118314871125));
#25222=CARTESIAN_POINT('Ctrl Pts',(48.3955718611241,-5.90176568155595,3.58514621746019));
#25223=CARTESIAN_POINT('Ctrl Pts',(48.3948635884079,-5.8874628440639,3.59381163136426));
#25224=CARTESIAN_POINT('Ctrl Pts',(48.3894543999969,-6.00090404394666,3.94385827440172));
#25225=CARTESIAN_POINT('Ctrl Pts',(48.3832404596072,-5.97673620504532,3.90682984442505));
#25226=CARTESIAN_POINT('Ctrl Pts',(48.3779018427349,-5.95526602423799,3.90698296769036));
#25227=CARTESIAN_POINT('Ctrl Pts',(48.37032875395,-5.91751946291063,3.9258357898974));
#25228=CARTESIAN_POINT('Ctrl Pts',(48.3680942820372,-5.90124308239061,3.94453548883914));
#25229=CARTESIAN_POINT('Ctrl Pts',(48.3680886315664,-5.8874628440639,3.94460021021535));
#25230=CARTESIAN_POINT('Ctrl Pts',(48.3614264232796,-6.007051447105,4.29441317095755));
#25231=CARTESIAN_POINT('Ctrl Pts',(48.3514946761257,-5.98314272027373,4.29430779651755));
#25232=CARTESIAN_POINT('Ctrl Pts',(48.3455075205231,-5.9599264156786,4.29450986621202));
#25233=CARTESIAN_POINT('Ctrl Pts',(48.3384990828948,-5.91876732373883,4.29496669282097));
#25234=CARTESIAN_POINT('Ctrl Pts',(48.3374778008691,-5.90082453639418,4.29522144973544));
#25235=CARTESIAN_POINT('Ctrl Pts',(48.3374778008691,-5.88746284406389,4.29522144973544));
#25236=CARTESIAN_POINT('Origin',(48.6500773750269,-5.88723161925852,4.32103607293));
#25237=CARTESIAN_POINT('Origin',(-32.9108164063353,-14.7669045823054,-35.8053910964449));
#25238=CARTESIAN_POINT('Origin',(-32.9108164063353,-12.8919045823054,-35.8053910964449));
#25239=CARTESIAN_POINT('Origin',(7.52116697235096,-12.8919045823054,-22.4729224553552));
#25240=CARTESIAN_POINT('Origin',(-32.9108164063353,-12.8919045823054,-35.8053910964449));
#25241=CARTESIAN_POINT('Origin',(0.0835265683620477,-13.5169045823054,0.0824317919394229));
#25242=CARTESIAN_POINT('Origin',(-41.2766849510695,-13.5169045823054,-36.9187829158523));
#25243=CARTESIAN_POINT('Ctrl Pts',(-42.8282205465608,-14.9232028613467,
-37.1013510452688));
#25244=CARTESIAN_POINT('Ctrl Pts',(-43.0950299957099,-14.6181128259927,
-37.1893316071079));
#25245=CARTESIAN_POINT('Ctrl Pts',(-42.8966189371508,-14.7022319922259,
-37.5436828577092));
#25246=CARTESIAN_POINT('Ctrl Pts',(-42.3441739848189,-14.453862129981,-36.941736426693));
#25247=CARTESIAN_POINT('Ctrl Pts',(-42.6106661613464,-14.1470746072311,
-37.0296123677042));
#25248=CARTESIAN_POINT('Ctrl Pts',(-42.4120640141707,-14.2328912595888,
-37.3846489359903));
#25249=CARTESIAN_POINT('Ctrl Pts',(-41.8596162483688,-13.9850662226602,
-36.7819532479775));
#25250=CARTESIAN_POINT('Ctrl Pts',(-42.1265166170242,-13.6772499732382,
-36.8699637905753));
#25251=CARTESIAN_POINT('Ctrl Pts',(-41.926981772331,-13.7640953522118,-37.2254587714377));
#25252=CARTESIAN_POINT('Ctrl Pts',(-41.3745486405956,-13.5169045823054,
-36.6220019389142));
#25253=CARTESIAN_POINT('Ctrl Pts',(-41.6427145102547,-13.2088427643879,
-36.7104297811587));
#25254=CARTESIAN_POINT('Ctrl Pts',(-41.4413720390587,-13.2959337131846,
-37.0661134559641));
#25255=CARTESIAN_POINT('Origin',(-41.2766849510695,-13.5169045823054,-36.9187829158523));
#25256=CARTESIAN_POINT('Ctrl Pts',(29.326104774044,-11.3294045823054,-38.5318534679819));
#25257=CARTESIAN_POINT('Ctrl Pts',(29.5041756346414,-11.3294045823054,-38.3970004975819));
#25258=CARTESIAN_POINT('Ctrl Pts',(29.4342239561067,-11.3294045823054,-38.184865357424));
#25259=CARTESIAN_POINT('Ctrl Pts',(29.3261048404642,-11.1601003758276,-38.5318534176819));
#25260=CARTESIAN_POINT('Ctrl Pts',(29.5041756838974,-11.2236230318997,-38.3970004597999));
#25261=CARTESIAN_POINT('Ctrl Pts',(29.4342239477177,-11.2447524820091,-38.1848653319834));
#25262=CARTESIAN_POINT('Ctrl Pts',(29.3879020055527,-10.9943058431437,-38.4851778011785));
#25263=CARTESIAN_POINT('Ctrl Pts',(29.5522467105556,-11.120480985332,-38.3601666095093));
#25264=CARTESIAN_POINT('Ctrl Pts',(29.4610377908797,-11.1618552084332,-38.1498951506615));
#25265=CARTESIAN_POINT('Ctrl Pts',(29.5859222979822,-10.7673610427475,-38.3339133713355));
#25266=CARTESIAN_POINT('Ctrl Pts',(29.6910051070021,-11.0035905561212,-38.2530870172994));
#25267=CARTESIAN_POINT('Ctrl Pts',(29.5467078428248,-11.0483828168177,-38.0362328980616));
#25268=CARTESIAN_POINT('Ctrl Pts',(29.7215756454094,-10.7044046130696,-38.2295231964381));
#25269=CARTESIAN_POINT('Ctrl Pts',(29.7830216375393,-10.9913613137645,-38.1816458099468));
#25270=CARTESIAN_POINT('Ctrl Pts',(29.6052696128604,-11.0169045823054,-37.9576620938899));
#25271=CARTESIAN_POINT('Ctrl Pts',(29.8546073333508,-10.7044045823054,-38.1258677820342));
#25272=CARTESIAN_POINT('Ctrl Pts',(29.8546073333508,-11.0169045823054,-38.1258677820342));
#25273=CARTESIAN_POINT('Ctrl Pts',(29.6625358445444,-11.0169045823054,-37.8793626234925));
#25274=CARTESIAN_POINT('Ctrl Pts',(29.6625358445444,-11.0169045823054,-37.8793626234925));
#25275=CARTESIAN_POINT('Ctrl Pts',(29.6486851738549,-11.0169045823054,-37.8983004889245));
#25276=CARTESIAN_POINT('Ctrl Pts',(29.6347995539505,-11.018741507632,-37.9172194534708));
#25277=CARTESIAN_POINT('Ctrl Pts',(29.6210644235878,-11.0223262069025,-37.9358685771032));
#25278=CARTESIAN_POINT('Ctrl Pts',(29.6079659337868,-11.0257447508548,-37.9536532904075));
#25279=CARTESIAN_POINT('Ctrl Pts',(29.5950033242865,-11.0307535195304,-37.9711937956057));
#25280=CARTESIAN_POINT('Ctrl Pts',(29.5823447885438,-11.0373176231359,-37.9882626371803));
#25281=CARTESIAN_POINT('Ctrl Pts',(29.5716026040572,-11.0428879997855,-38.0027474598245));
#25282=CARTESIAN_POINT('Ctrl Pts',(29.5610692588669,-11.0495814926586,-38.0168965067492));
#25283=CARTESIAN_POINT('Ctrl Pts',(29.5508418916121,-11.0574216164539,-38.0305775227158));
#25284=CARTESIAN_POINT('Ctrl Pts',(29.5487244956887,-11.059044775743,-38.0334099356637));
#25285=CARTESIAN_POINT('Ctrl Pts',(29.5466202962154,-11.0607171987456,-38.036222182028));
#25286=CARTESIAN_POINT('Ctrl Pts',(29.5445302949047,-11.0624392724585,-38.0390129068931));
#25287=CARTESIAN_POINT('Ctrl Pts',(29.5350786849189,-11.0702270039863,-38.0516333980223));
#25288=CARTESIAN_POINT('Ctrl Pts',(29.5259128880755,-11.0790298901569,-38.0638160310099));
#25289=CARTESIAN_POINT('Ctrl Pts',(29.5171571849087,-11.0888942095813,-38.07544538592));
#25290=CARTESIAN_POINT('Ctrl Pts',(29.514625005418,-11.0917470047092,-38.0788086353851));
#25291=CARTESIAN_POINT('Ctrl Pts',(29.5121272694726,-11.0946887229266,-38.0821253594875));
#25292=CARTESIAN_POINT('Ctrl Pts',(29.5096673709869,-11.0977208509785,-38.0853921096116));
#25293=CARTESIAN_POINT('Ctrl Pts',(29.5077130397355,-11.1001298051058,-38.0879874654343));
#25294=CARTESIAN_POINT('Ctrl Pts',(29.5057827559271,-11.1025951245287,-38.0905492193572));
#25295=CARTESIAN_POINT('Ctrl Pts',(29.5038785684965,-11.1051169477604,-38.0930746719112));
#25296=CARTESIAN_POINT('Ctrl Pts',(29.4943883336226,-11.1176854031531,-38.1056612153982));
#25297=CARTESIAN_POINT('Ctrl Pts',(29.4855598341066,-11.1317057213307,-38.1173411611829));
#25298=CARTESIAN_POINT('Ctrl Pts',(29.4775886595648,-11.1469740767486,-38.1278665693324));
#25299=CARTESIAN_POINT('Ctrl Pts',(29.4693767293853,-11.1627035866208,-38.1387098793592));
#25300=CARTESIAN_POINT('Ctrl Pts',(29.4620748017894,-11.179757668146,-38.1483277159914));
#25301=CARTESIAN_POINT('Ctrl Pts',(29.4559087086157,-11.1978608317579,-38.1564354879713));
#25302=CARTESIAN_POINT('Ctrl Pts',(29.4495980788777,-11.2163883433315,-38.1647333105184));
#25303=CARTESIAN_POINT('Ctrl Pts',(29.4444773334721,-11.236014539749,-38.1714492216813));
#25304=CARTESIAN_POINT('Ctrl Pts',(29.4407987204571,-11.2563909917773,-38.1762670359295));
#25305=CARTESIAN_POINT('Ctrl Pts',(29.4369636562796,-11.2776340529315,-38.1812897514916));
#25306=CARTESIAN_POINT('Ctrl Pts',(29.4346962366054,-11.299692404456,-38.1842491853732));
#25307=CARTESIAN_POINT('Ctrl Pts',(29.4342900459812,-11.3221161967402,-38.1847791414454));
#25308=CARTESIAN_POINT('Ctrl Pts',(29.434246110956,-11.3245416340106,-38.1848364633824));
#25309=CARTESIAN_POINT('Ctrl Pts',(29.4342239561067,-11.3269712973085,-38.184865357424));
#25310=CARTESIAN_POINT('Ctrl Pts',(29.4342239561067,-11.3294045823054,-38.184865357424));
#25311=CARTESIAN_POINT('Origin',(29.6625358445444,-10.7044045823054,-37.8793626234925));
#25312=CARTESIAN_POINT('Ctrl Pts',(34.4520919977564,-13.5169045823054,-34.2918998972067));
#25313=CARTESIAN_POINT('Ctrl Pts',(34.4520919977564,-13.2044045823054,-34.2918998972067));
#25314=CARTESIAN_POINT('Ctrl Pts',(34.7488729746945,-13.2044045823054,-34.1940362076806));
#25315=CARTESIAN_POINT('Ctrl Pts',(34.4246143593772,-13.5169045582439,-34.2085713368222));
#25316=CARTESIAN_POINT('Ctrl Pts',(34.4350349767327,-13.1861191316365,-34.2401728533213));
#25317=CARTESIAN_POINT('Ctrl Pts',(34.7491730539449,-13.2044045823054,-34.1381738077117));
#25318=CARTESIAN_POINT('Ctrl Pts',(34.3978522728513,-13.5027466839946,-34.1274127557131));
#25319=CARTESIAN_POINT('Ctrl Pts',(34.420802744593,-13.1578432798921,-34.1970122512738));
#25320=CARTESIAN_POINT('Ctrl Pts',(34.7495154373051,-13.1973256316197,-34.0836803810649));
#25321=CARTESIAN_POINT('Ctrl Pts',(34.3459175121228,-13.4449866817215,-33.9699156380316));
#25322=CARTESIAN_POINT('Ctrl Pts',(34.3984170950457,-13.0892356355763,-34.1291256329142));
#25323=CARTESIAN_POINT('Ctrl Pts',(34.7502673139448,-13.1684456335482,-33.9777792652241));
#25324=CARTESIAN_POINT('Ctrl Pts',(34.3222371758063,-13.4031153721669,-33.8981027585021));
#25325=CARTESIAN_POINT('Ctrl Pts',(34.3914218944348,-13.0503322093645,-34.1079120195585));
#25326=CARTESIAN_POINT('Ctrl Pts',(34.7506550934714,-13.147509967376,-33.9294147505826));
#25327=CARTESIAN_POINT('Ctrl Pts',(34.2800267092033,-13.2902331116006,-33.770095490678));
#25328=CARTESIAN_POINT('Ctrl Pts',(34.3847390713609,-12.9767617731721,-34.087645720892));
#25329=CARTESIAN_POINT('Ctrl Pts',(34.7513994248545,-13.0910688568131,-33.8431120353597));
#25330=CARTESIAN_POINT('Ctrl Pts',(34.2628371595374,-13.2224528271011,-33.717966541037));
#25331=CARTESIAN_POINT('Ctrl Pts',(34.3858673504075,-12.9460615526398,-34.091067334764));
#25332=CARTESIAN_POINT('Ctrl Pts',(34.7517320489624,-13.0571787063097,-33.8079153247474));
#25333=CARTESIAN_POINT('Ctrl Pts',(34.2384230621111,-13.065416935761,-33.6439284609247));
#25334=CARTESIAN_POINT('Ctrl Pts',(34.3902784659414,-12.9052920386063,-34.1044444635434));
#25335=CARTESIAN_POINT('Ctrl Pts',(34.7522178573803,-12.9786607574268,-33.7579024304006));
#25336=CARTESIAN_POINT('Ctrl Pts',(34.2319045968862,-12.9802875861309,-33.6241605931184));
#25337=CARTESIAN_POINT('Ctrl Pts',(34.393033636199,-12.8977806170666,-34.1127997802578));
#25338=CARTESIAN_POINT('Ctrl Pts',(34.7523554491597,-12.9360960854271,-33.7445354129988));
#25339=CARTESIAN_POINT('Ctrl Pts',(34.2319046026008,-12.8919045823054,-33.6241606104485));
#25340=CARTESIAN_POINT('Ctrl Pts',(34.3930336345113,-12.8919045823054,-34.112799775138));
#25341=CARTESIAN_POINT('Ctrl Pts',(34.7523554432478,-12.8919045823054,-33.7445354190578));
#25342=CARTESIAN_POINT('Ctrl Pts',(37.7386905645208,-14.6563598281215,-42.7974778141527));
#25343=CARTESIAN_POINT('Ctrl Pts',(37.8152217296418,-14.7669045823078,-42.8493171995473));
#25344=CARTESIAN_POINT('Ctrl Pts',(37.935395944751,-14.7669045823054,-42.9300026606738));
#25345=CARTESIAN_POINT('Ctrl Pts',(37.7175355100096,-14.6732979129446,-42.8591973289493));
#25346=CARTESIAN_POINT('Ctrl Pts',(37.7874533080794,-14.7669045823044,-42.9232591435907));
#25347=CARTESIAN_POINT('Ctrl Pts',(37.8823038919049,-14.7669045823054,-43.0182648484161));
#25348=CARTESIAN_POINT('Ctrl Pts',(37.6775546541054,-14.6836226395046,-42.9057319112783));
#25349=CARTESIAN_POINT('Ctrl Pts',(37.7271961037498,-14.7669045823054,-42.9839489162578));
#25350=CARTESIAN_POINT('Ctrl Pts',(37.7948585081688,-14.7669045823054,-43.0905896374617));
#25351=CARTESIAN_POINT('Ctrl Pts',(37.5997129170687,-14.6837071744148,-42.9316733022326));
#25352=CARTESIAN_POINT('Ctrl Pts',(37.6161850043513,-14.7669045823054,-43.0208827520291));
#25353=CARTESIAN_POINT('Ctrl Pts',(37.6386288705569,-14.7669045823054,-43.1424614647264));
#25354=CARTESIAN_POINT('Ctrl Pts',(37.5689613038834,-14.6805726740705,-42.9316885218425));
#25355=CARTESIAN_POINT('Ctrl Pts',(37.5728052530044,-14.7669045823053,-43.022898282639));
#25356=CARTESIAN_POINT('Ctrl Pts',(37.5790568393347,-14.7669045823054,-43.1489392469548));
#25357=CARTESIAN_POINT('Ctrl Pts',(37.4757303120884,-14.66352762411,-42.9073579283318));
#25358=CARTESIAN_POINT('Ctrl Pts',(37.445202377388,-14.7669045823055,-42.9986732904205));
#25359=CARTESIAN_POINT('Ctrl Pts',(37.4036140787982,-14.7669045823054,-43.1351870004211));
#25360=CARTESIAN_POINT('Ctrl Pts',(37.4132032793102,-14.6424796666972,-42.8599547573657));
#25361=CARTESIAN_POINT('Ctrl Pts',(37.364845501704,-14.7669045823051,-42.9421725988748));
#25362=CARTESIAN_POINT('Ctrl Pts',(37.2925429683339,-14.7669045823054,-43.0833710447635));
#25363=CARTESIAN_POINT('Ctrl Pts',(37.2264916052012,-14.5607785229746,-42.657224059441));
#25364=CARTESIAN_POINT('Ctrl Pts',(37.1424895246967,-14.7669045823062,-42.6940481533457));
#25365=CARTESIAN_POINT('Ctrl Pts',(36.9739954005229,-14.7669045823054,-42.8448791143223));
#25366=CARTESIAN_POINT('Ctrl Pts',(37.1311194555558,-14.4859905466154,-42.4463288741486));
#25367=CARTESIAN_POINT('Ctrl Pts',(37.0866121993381,-14.7669045823059,-42.4219753342952));
#25368=CARTESIAN_POINT('Ctrl Pts',(36.8345069741914,-14.7669045823054,-42.5760612268253));
#25369=CARTESIAN_POINT('Ctrl Pts',(37.0775149489995,-14.4183787521282,-42.2439952620268));
#25370=CARTESIAN_POINT('Ctrl Pts',(37.1178746289163,-14.766904582305,-42.2357920123654));
#25371=CARTESIAN_POINT('Ctrl Pts',(36.7741979390219,-14.7669045823054,-42.3109485117452));
#25372=CARTESIAN_POINT('Origin',(36.8109793750892,-14.4544045823054,-42.4433312829855));
#25373=CARTESIAN_POINT('Origin',(0.0835265683620477,-14.4544045823054,0.0824317919394229));
#25374=CARTESIAN_POINT('Origin',(47.5194292675621,-14.4544045823054,32.2548881068839));
#25375=CARTESIAN_POINT('Ctrl Pts',(39.8249086674878,-6.28105857414855,27.6158484236678));
#25376=CARTESIAN_POINT('Ctrl Pts',(39.9934560522847,-6.09633085020216,27.6714270160236));
#25377=CARTESIAN_POINT('Ctrl Pts',(40.1051877166575,-6.06008770502775,27.4437781582428));
#25378=CARTESIAN_POINT('Ctrl Pts',(41.997582097766,-8.47898077424469,28.3322886760592));
#25379=CARTESIAN_POINT('Ctrl Pts',(42.1761782548842,-8.30110493968489,28.3911808565934));
#25380=CARTESIAN_POINT('Ctrl Pts',(42.2795010816781,-8.25800948639213,28.1578189230589));
#25381=CARTESIAN_POINT('Ctrl Pts',(44.1644194400702,-10.6833293750622,29.0468044752481));
#25382=CARTESIAN_POINT('Ctrl Pts',(44.3429038866861,-10.5025148293853,29.1056598191394));
#25383=CARTESIAN_POINT('Ctrl Pts',(44.4477081038169,-10.4623581523692,28.8702339699961));
#25384=CARTESIAN_POINT('Ctrl Pts',(46.3272934177549,-12.8919045823054,29.7600133527852));
#25385=CARTESIAN_POINT('Ctrl Pts',(46.5008548189629,-12.7034528674627,29.8172453197959));
#25386=CARTESIAN_POINT('Ctrl Pts',(46.611780876039,-12.6709337131846,29.5815526781396));
#25387=CARTESIAN_POINT('Ctrl Pts',(40.153012388794,-6.10843371318468,27.4594837601833));
#25388=CARTESIAN_POINT('Ctrl Pts',(40.1486301258045,-6.10756827058304,27.4643636112223));
#25389=CARTESIAN_POINT('Ctrl Pts',(40.14431636544,-6.10708538385354,27.4693390586013));
#25390=CARTESIAN_POINT('Ctrl Pts',(40.1401031486147,-6.10700426240365,27.4743794740622));
#25391=CARTESIAN_POINT('Ctrl Pts',(40.1337833233766,-6.10688258022881,27.4819400972536));
#25392=CARTESIAN_POINT('Ctrl Pts',(40.127689581349,-6.10766522922463,27.4896462179766));
#25393=CARTESIAN_POINT('Ctrl Pts',(40.1219384863636,-6.1094056136749,27.4974038197989));
#25394=CARTESIAN_POINT('Ctrl Pts',(40.119062938871,-6.11027580590004,27.5012826207101));
#25395=CARTESIAN_POINT('Ctrl Pts',(40.1162731700049,-6.1113852520171,27.5051744892978));
#25396=CARTESIAN_POINT('Ctrl Pts',(40.1135841376133,-6.11273984167805,27.5090689245252));
#25397=CARTESIAN_POINT('Ctrl Pts',(40.1129118795153,-6.11307848909328,27.510042533332));
#25398=CARTESIAN_POINT('Ctrl Pts',(40.1122459177464,-6.11343245632759,27.511016306785));
#25399=CARTESIAN_POINT('Ctrl Pts',(40.1115864861771,-6.11380183251757,27.5119900892948));
#25400=CARTESIAN_POINT('Ctrl Pts',(40.1105973388232,-6.11435589680255,27.5134507630594));
#25401=CARTESIAN_POINT('Ctrl Pts',(40.1096228845693,-6.11494463135663,27.5149114564014));
#25402=CARTESIAN_POINT('Ctrl Pts',(40.1086639111446,-6.115568333847,27.5163716586017));
#25403=CARTESIAN_POINT('Ctrl Pts',(40.1077049377198,-6.11619203633737,27.517831860802));
#25404=CARTESIAN_POINT('Ctrl Pts',(40.1067614452345,-6.11685070666524,27.519291571862));
#25405=CARTESIAN_POINT('Ctrl Pts',(40.1058342180418,-6.11754464002828,27.5207502983356));
#25406=CARTESIAN_POINT('Ctrl Pts',(40.1008056546947,-6.12130799802938,27.5286613028186));
#25407=CARTESIAN_POINT('Ctrl Pts',(40.0963697525875,-6.12597258662923,27.5363115221513));
#25408=CARTESIAN_POINT('Ctrl Pts',(40.0924653997853,-6.13138771967841,27.5436694209767));
#25409=CARTESIAN_POINT('Ctrl Pts',(40.0912502383763,-6.13307308497174,27.5459594380823));
#25410=CARTESIAN_POINT('Ctrl Pts',(40.090086516912,-6.13483149128332,27.5482213190137));
#25411=CARTESIAN_POINT('Ctrl Pts',(40.0889722671577,-6.13665930617706,27.5504545293107));
#25412=CARTESIAN_POINT('Ctrl Pts',(40.0883854708883,-6.13762188656504,27.5516306026875));
#25413=CARTESIAN_POINT('Ctrl Pts',(40.0878124152614,-6.13860357319269,27.5527985817608));
#25414=CARTESIAN_POINT('Ctrl Pts',(40.0872528103463,-6.13960373328463,27.5539582878036));
#25415=CARTESIAN_POINT('Ctrl Pts',(40.0870002128769,-6.14005519091391,27.5544817621404));
#25416=CARTESIAN_POINT('Ctrl Pts',(40.0867503319911,-6.14051040725672,27.555003558958));
#25417=CARTESIAN_POINT('Ctrl Pts',(40.086503247387,-6.14096936706302,27.5555236415609));
#25418=CARTESIAN_POINT('Ctrl Pts',(40.0862713642513,-6.14140009013227,27.5560117269487));
#25419=CARTESIAN_POINT('Ctrl Pts',(40.0860418533618,-6.1418340234271,27.5564983732832));
#25420=CARTESIAN_POINT('Ctrl Pts',(40.0858147608252,-6.14227112540981,27.5569835610311));
#25421=CARTESIAN_POINT('Ctrl Pts',(40.0825312534216,-6.14859113758575,27.563998840292));
#25422=CARTESIAN_POINT('Ctrl Pts',(40.0797513639648,-6.15557322588934,27.5707108135461));
#25423=CARTESIAN_POINT('Ctrl Pts',(40.0774276984569,-6.1630485902823,27.5771166413194));
#25424=CARTESIAN_POINT('Ctrl Pts',(40.075339709593,-6.16976576947768,27.5828727611265));
#25425=CARTESIAN_POINT('Ctrl Pts',(40.0736091318008,-6.17677030338731,27.5883069387177));
#25426=CARTESIAN_POINT('Ctrl Pts',(40.0721954246486,-6.18399336848783,27.5934675539933));
#25427=CARTESIAN_POINT('Ctrl Pts',(40.0715542408364,-6.18726937399525,27.5958081398567));
#25428=CARTESIAN_POINT('Ctrl Pts',(40.070978696512,-6.19059093207267,27.5980923367893));
#25429=CARTESIAN_POINT('Ctrl Pts',(40.07046715491,-6.19395424178566,27.600324154726));
#25430=CARTESIAN_POINT('Ctrl Pts',(40.0698523767083,-6.19799631673864,27.6030063862633));
#25431=CARTESIAN_POINT('Ctrl Pts',(40.0693281053813,-6.20209746439246,27.6056128186841));
#25432=CARTESIAN_POINT('Ctrl Pts',(40.0688877556671,-6.20624978925051,27.6081491750566));
#25433=CARTESIAN_POINT('Ctrl Pts',(40.0685024496673,-6.20988307350131,27.6103684868826));
#25434=CARTESIAN_POINT('Ctrl Pts',(40.0681813835459,-6.21355555791223,27.6125341305234));
#25435=CARTESIAN_POINT('Ctrl Pts',(40.0679199399159,-6.2172623580558,27.6146493155572));
#25436=CARTESIAN_POINT('Ctrl Pts',(40.0671497781398,-6.22818186595188,27.6208802367785));
#25437=CARTESIAN_POINT('Ctrl Pts',(40.0668900862771,-6.23942896207781,27.6266930616364));
#25438=CARTESIAN_POINT('Ctrl Pts',(40.0670349189619,-6.25083884461348,27.6321118626055));
#25439=CARTESIAN_POINT('Ctrl Pts',(40.0670644700791,-6.25316687420515,27.6332174944092));
#25440=CARTESIAN_POINT('Ctrl Pts',(40.0671108919301,-6.25550185226918,27.6343067222454));
#25441=CARTESIAN_POINT('Ctrl Pts',(40.0671733296103,-6.25784263179034,27.6353797440325));
#25442=CARTESIAN_POINT('Ctrl Pts',(40.0675320452674,-6.27129082943959,27.641544446408));
#25443=CARTESIAN_POINT('Ctrl Pts',(40.0683768978808,-6.28489536287217,27.6472113601885));
#25444=CARTESIAN_POINT('Ctrl Pts',(40.0695536495387,-6.29858154433864,27.6524587325793));
#25445=CARTESIAN_POINT('Ctrl Pts',(40.0704275122879,-6.30874498373682,27.6563554623885));
#25446=CARTESIAN_POINT('Ctrl Pts',(40.0715188210737,-6.31897515340961,27.6600258390141));
#25447=CARTESIAN_POINT('Ctrl Pts',(40.0728000600482,-6.32926010589388,27.6634970067625));
#25448=CARTESIAN_POINT('Ctrl Pts',(40.074950602702,-6.34652326245748,27.6693233158672));
#25449=CARTESIAN_POINT('Ctrl Pts',(40.0776339280651,-6.36392973954521,27.6745857947252));
#25450=CARTESIAN_POINT('Ctrl Pts',(40.0807437314268,-6.38139910656903,27.6793726882152));
#25451=CARTESIAN_POINT('Ctrl Pts',(40.0841784757829,-6.400693834502,27.6846597605749));
#25452=CARTESIAN_POINT('Ctrl Pts',(40.0881335071639,-6.42006561697338,27.6893667923115));
#25453=CARTESIAN_POINT('Ctrl Pts',(40.0925060685141,-6.43945161631725,27.6935864739196));
#25454=CARTESIAN_POINT('Ctrl Pts',(40.0971878544237,-6.46020858032532,27.6981045685358));
#25455=CARTESIAN_POINT('Ctrl Pts',(40.1023486755735,-6.48098271074861,27.7020639266992));
#25456=CARTESIAN_POINT('Ctrl Pts',(40.1079031404676,-6.50173650943862,27.705549038395));
#25457=CARTESIAN_POINT('Ctrl Pts',(40.1141796220518,-6.52518806377629,27.7094871746142));
#25458=CARTESIAN_POINT('Ctrl Pts',(40.1209590306374,-6.54861499437352,27.712820039933));
#25459=CARTESIAN_POINT('Ctrl Pts',(40.1281636304217,-6.57199467991746,27.7156308755257));
#25460=CARTESIAN_POINT('Ctrl Pts',(40.1305643122126,-6.57978514532063,27.7165674885266));
#25461=CARTESIAN_POINT('Ctrl Pts',(40.1330125170019,-6.58757049925619,27.7174458345116));
#25462=CARTESIAN_POINT('Ctrl Pts',(40.1355061827836,-6.5953500914164,27.7182681242769));
#25463=CARTESIAN_POINT('Origin',(46.4251571072811,-12.8919045823054,29.4632323758471));
#25464=CARTESIAN_POINT('Ctrl Pts',(-39.6578555996089,-6.28105864379379,
-27.4509848624907));
#25465=CARTESIAN_POINT('Ctrl Pts',(-39.826402984466,-6.09633091980368,-27.5065634548664));
#25466=CARTESIAN_POINT('Ctrl Pts',(-39.9381346488306,-6.060087774673,-27.2789145969897));
#25467=CARTESIAN_POINT('Ctrl Pts',(-41.8305313962535,-8.47898323805638,
-28.1674258951927));
#25468=CARTESIAN_POINT('Ctrl Pts',(-42.0091275727744,-8.30110741938527,
-28.2263180821171));
#25469=CARTESIAN_POINT('Ctrl Pts',(-42.1124503819745,-8.25801195014743,
-27.9929561395079));
#25470=CARTESIAN_POINT('Ctrl Pts',(-43.9973666758772,-10.6833297554487,
-28.8819410142116));
#25471=CARTESIAN_POINT('Ctrl Pts',(-44.1758511208521,-10.5025152076406,
-28.9407963575876));
#25472=CARTESIAN_POINT('Ctrl Pts',(-44.2806553397966,-10.4623585327411,
-28.7053705086298));
#25473=CARTESIAN_POINT('Ctrl Pts',(-46.1602402810308,-12.8919045823054,
-29.5951497689063));
#25474=CARTESIAN_POINT('Ctrl Pts',(-46.3338016822388,-12.7034528674627,
-29.6523817359171));
#25475=CARTESIAN_POINT('Ctrl Pts',(-46.4447277393149,-12.6709337131846,
-29.4166890942607));
#25476=CARTESIAN_POINT('Ctrl Pts',(-39.9859592520697,-6.10843371318464,
-27.2946201763047));
#25477=CARTESIAN_POINT('Ctrl Pts',(-39.9815769890805,-6.10756827058306,
-27.2995000273434));
#25478=CARTESIAN_POINT('Ctrl Pts',(-39.9772632287159,-6.10708538385355,
-27.3044754747224));
#25479=CARTESIAN_POINT('Ctrl Pts',(-39.9730500118906,-6.10700426240366,
-27.3095158901833));
#25480=CARTESIAN_POINT('Ctrl Pts',(-39.9667301866525,-6.10688258022884,
-27.3170765133747));
#25481=CARTESIAN_POINT('Ctrl Pts',(-39.9606364446249,-6.10766522922467,
-27.3247826340977));
#25482=CARTESIAN_POINT('Ctrl Pts',(-39.9548853496395,-6.10940561367495,
-27.3325402359201));
#25483=CARTESIAN_POINT('Ctrl Pts',(-39.9520098021468,-6.11027580590009,
-27.3364190368312));
#25484=CARTESIAN_POINT('Ctrl Pts',(-39.9492200332808,-6.11138525201715,
-27.340310905419));
#25485=CARTESIAN_POINT('Ctrl Pts',(-39.9465310008892,-6.1127398416781,-27.3442053406463));
#25486=CARTESIAN_POINT('Ctrl Pts',(-39.9458587427912,-6.11307848909333,
-27.3451789494531));
#25487=CARTESIAN_POINT('Ctrl Pts',(-39.9451927810223,-6.11343245632765,
-27.3461527229061));
#25488=CARTESIAN_POINT('Ctrl Pts',(-39.944533349453,-6.11380183251763,-27.3471265054159));
#25489=CARTESIAN_POINT('Ctrl Pts',(-39.9435442020991,-6.11435589680261,
-27.3485871791806));
#25490=CARTESIAN_POINT('Ctrl Pts',(-39.9425697478452,-6.11494463135667,
-27.3500478725225));
#25491=CARTESIAN_POINT('Ctrl Pts',(-39.9416107744204,-6.11556833384704,
-27.3515080747228));
#25492=CARTESIAN_POINT('Ctrl Pts',(-39.9406518009957,-6.11619203633741,
-27.3529682769231));
#25493=CARTESIAN_POINT('Ctrl Pts',(-39.9397083085104,-6.11685070666528,
-27.3544279879831));
#25494=CARTESIAN_POINT('Ctrl Pts',(-39.9387810813177,-6.11754464002833,
-27.3558867144568));
#25495=CARTESIAN_POINT('Ctrl Pts',(-39.933752517971,-6.12130799802912,-27.3637977189391));
#25496=CARTESIAN_POINT('Ctrl Pts',(-39.9293166158641,-6.12597258662852,
-27.3714479382713));
#25497=CARTESIAN_POINT('Ctrl Pts',(-39.9254122630621,-6.13138771967716,
-27.3788058370961));
#25498=CARTESIAN_POINT('Ctrl Pts',(-39.9241971016528,-6.13307308497087,
-27.3810958542024));
#25499=CARTESIAN_POINT('Ctrl Pts',(-39.9230333801882,-6.13483149128286,
-27.3833577351343));
#25500=CARTESIAN_POINT('Ctrl Pts',(-39.9219191304336,-6.13665930617706,
-27.3855909454319));
#25501=CARTESIAN_POINT('Ctrl Pts',(-39.9213323341642,-6.13762188656503,
-27.3867670188086));
#25502=CARTESIAN_POINT('Ctrl Pts',(-39.9207592785374,-6.13860357319269,
-27.3879349978819));
#25503=CARTESIAN_POINT('Ctrl Pts',(-39.9201996736223,-6.13960373328462,
-27.3890947039248));
#25504=CARTESIAN_POINT('Ctrl Pts',(-39.9199470761528,-6.1400551909139,-27.3896181782615));
#25505=CARTESIAN_POINT('Ctrl Pts',(-39.919697195267,-6.14051040725671,-27.3901399750791));
#25506=CARTESIAN_POINT('Ctrl Pts',(-39.9194501106629,-6.14096936706301,
-27.3906600576821));
#25507=CARTESIAN_POINT('Ctrl Pts',(-39.9192182275272,-6.14140009013226,
-27.3911481430698));
#25508=CARTESIAN_POINT('Ctrl Pts',(-39.9189887166377,-6.1418340234271,-27.3916347894044));
#25509=CARTESIAN_POINT('Ctrl Pts',(-39.9187616241011,-6.1422711254098,-27.3921199771522));
#25510=CARTESIAN_POINT('Ctrl Pts',(-39.9154781166975,-6.14859113758575,
-27.3991352564131));
#25511=CARTESIAN_POINT('Ctrl Pts',(-39.9126982272407,-6.15557322588935,
-27.4058472296673));
#25512=CARTESIAN_POINT('Ctrl Pts',(-39.9103745617328,-6.16304859028231,
-27.4122530574405));
#25513=CARTESIAN_POINT('Ctrl Pts',(-39.9082865728688,-6.16976576947789,
-27.4180091772478));
#25514=CARTESIAN_POINT('Ctrl Pts',(-39.9065559950766,-6.17677030338776,
-27.4234433548392));
#25515=CARTESIAN_POINT('Ctrl Pts',(-39.9051422879244,-6.18399336848851,
-27.4286039701149));
#25516=CARTESIAN_POINT('Ctrl Pts',(-39.9045011041123,-6.18726937399572,
-27.4309445559781));
#25517=CARTESIAN_POINT('Ctrl Pts',(-39.9039255597879,-6.19059093207291,
-27.4332287529105));
#25518=CARTESIAN_POINT('Ctrl Pts',(-39.9034140181859,-6.19395424178567,
-27.4354605708472));
#25519=CARTESIAN_POINT('Ctrl Pts',(-39.9027992399842,-6.19799631673865,
-27.4381428023844));
#25520=CARTESIAN_POINT('Ctrl Pts',(-39.9022749686572,-6.20209746439248,
-27.4407492348052));
#25521=CARTESIAN_POINT('Ctrl Pts',(-39.901834618943,-6.20624978925053,-27.4432855911778));
#25522=CARTESIAN_POINT('Ctrl Pts',(-39.9014493129432,-6.20988307350132,
-27.4455049030038));
#25523=CARTESIAN_POINT('Ctrl Pts',(-39.9011282468218,-6.21355555791224,
-27.4476705466445));
#25524=CARTESIAN_POINT('Ctrl Pts',(-39.9008668031918,-6.21726235805581,
-27.4497857316783));
#25525=CARTESIAN_POINT('Ctrl Pts',(-39.9000966414157,-6.22818186595271,
-27.4560166529001));
#25526=CARTESIAN_POINT('Ctrl Pts',(-39.899836949553,-6.2394289620795,-27.4618294777584));
#25527=CARTESIAN_POINT('Ctrl Pts',(-39.8999817822378,-6.25083884461606,
-27.4672482787279));
#25528=CARTESIAN_POINT('Ctrl Pts',(-39.900011333355,-6.25316687420688,-27.4683539105311));
#25529=CARTESIAN_POINT('Ctrl Pts',(-39.900057755206,-6.25550185227005,-27.469443138367));
#25530=CARTESIAN_POINT('Ctrl Pts',(-39.9001201928862,-6.25784263179036,
-27.4705161601537));
#25531=CARTESIAN_POINT('Ctrl Pts',(-39.9004789085434,-6.27129082943962,
-27.4766808625291));
#25532=CARTESIAN_POINT('Ctrl Pts',(-39.9013237611568,-6.28489536287222,
-27.4823477763096));
#25533=CARTESIAN_POINT('Ctrl Pts',(-39.9025005128147,-6.29858154433868,
-27.4875951487004));
#25534=CARTESIAN_POINT('Ctrl Pts',(-39.9033743755616,-6.30874498371071,
-27.4914918784995));
#25535=CARTESIAN_POINT('Ctrl Pts',(-39.904465684344,-6.31897515335698,-27.4951622551162));
#25536=CARTESIAN_POINT('Ctrl Pts',(-39.905746923314,-6.32926010581451,-27.4986334228567));
#25537=CARTESIAN_POINT('Ctrl Pts',(-39.9078974659659,-6.3465232623761,-27.5044597319625));
#25538=CARTESIAN_POINT('Ctrl Pts',(-39.910580791327,-6.36392973946194,-27.5097222108217));
#25539=CARTESIAN_POINT('Ctrl Pts',(-39.9136905946869,-6.38139910648396,
-27.5145091043127));
#25540=CARTESIAN_POINT('Ctrl Pts',(-39.917125339041,-6.40069383441468,-27.5197961766734));
#25541=CARTESIAN_POINT('Ctrl Pts',(-39.9210803704199,-6.42006561688391,
-27.5245032084111));
#25542=CARTESIAN_POINT('Ctrl Pts',(-39.9254529317683,-6.43945161622571,
-27.5287228900203));
#25543=CARTESIAN_POINT('Ctrl Pts',(-39.9301347176756,-6.46020858023109,
-27.5332409846376));
#25544=CARTESIAN_POINT('Ctrl Pts',(-39.9352955388234,-6.48098271065176,
-27.537200342802));
#25545=CARTESIAN_POINT('Ctrl Pts',(-39.9408500037156,-6.50173650933919,
-27.5406854544989));
#25546=CARTESIAN_POINT('Ctrl Pts',(-39.9471264852975,-6.52518806367359,
-27.5446235907193));
#25547=CARTESIAN_POINT('Ctrl Pts',(-39.953905893881,-6.54861499426759,-27.5479564560394));
#25548=CARTESIAN_POINT('Ctrl Pts',(-39.9611104936634,-6.57199467980834,
-27.5507672916335));
#25549=CARTESIAN_POINT('Ctrl Pts',(-39.963511175461,-6.57978514523424,-27.5517039046378));
#25550=CARTESIAN_POINT('Ctrl Pts',(-39.9659593802573,-6.58757049919249,
-27.5525822506258));
#25551=CARTESIAN_POINT('Ctrl Pts',(-39.9684530460464,-6.59535009137536,
-27.5534045403938));
#25552=CARTESIAN_POINT('Origin',(-46.258103970557,-12.8919045823054,-29.2983687919682));
#25553=CARTESIAN_POINT('Origin',(0.0835265683620477,-5.88746284406389,0.0824317919394229));
#25554=CARTESIAN_POINT('Origin',(40.3354637847015,-5.88746284406389,27.5841417448109));
#25555=CARTESIAN_POINT('Origin',(-32.9108164063353,-12.8919045823054,-35.8053910964449));
#25556=CARTESIAN_POINT('Origin',(-32.9108164063353,-12.8919045823054,-35.8053910964449));
#25557=CARTESIAN_POINT('Origin',(-41.2766849510695,-13.5169045823054,-36.9187829158523));
#25558=CARTESIAN_POINT('Origin',(-41.2766849510695,-13.5169045823054,-36.9187829158523));
#25559=CARTESIAN_POINT('Origin',(19.8255764196421,-11.0169045823054,-10.0436051386457));
#25560=CARTESIAN_POINT('Origin',(19.8255764196421,-11.3294045823054,-10.0436051386457));
#25561=CARTESIAN_POINT('Origin',(15.4714058027788,-11.3294045823054,5.15659338881741));
#25562=CARTESIAN_POINT('Origin',(20.4191383735183,-11.3294045823054,-9.84787775959334));
#25563=CARTESIAN_POINT('Origin',(0.0835265683620477,-10.7044045823054,0.0824317919394229));
#25564=CARTESIAN_POINT('Origin',(34.0350086811056,-10.7044045823054,-34.02493526194));
#25565=CARTESIAN_POINT('Origin',(29.4071186530799,-14.4544045823054,-19.9904171446541));
#25566=CARTESIAN_POINT('Origin',(20.56141397709,-14.4544045823054,6.83502636924522));
#25567=CARTESIAN_POINT('Ctrl Pts',(46.5427518284381,-14.426701821061,32.1322496158952));
#25568=CARTESIAN_POINT('Ctrl Pts',(46.5548124230274,-14.7669045823053,32.1041265430089));
#25569=CARTESIAN_POINT('Ctrl Pts',(46.4212196497479,-14.7669045823054,32.418869262555));
#25570=CARTESIAN_POINT('Ctrl Pts',(46.6932699125038,-14.479760966508,32.1906930433489));
#25571=CARTESIAN_POINT('Ctrl Pts',(46.6642075899464,-14.7669045823056,32.2097370359491));
#25572=CARTESIAN_POINT('Ctrl Pts',(46.6172868947414,-14.7669045823054,32.5015126714166));
#25573=CARTESIAN_POINT('Ctrl Pts',(46.8607640732745,-14.5360769750828,32.2283316967679));
#25574=CARTESIAN_POINT('Ctrl Pts',(46.8417224039433,-14.766904582305,32.2976409195446));
#25575=CARTESIAN_POINT('Ctrl Pts',(46.8413031346229,-14.7669045823054,32.5405339499658));
#25576=CARTESIAN_POINT('Ctrl Pts',(47.1709605059096,-14.6333609973517,32.229273177524));
#25577=CARTESIAN_POINT('Ctrl Pts',(47.1941665884612,-14.7669045823058,32.3240183566974));
#25578=CARTESIAN_POINT('Ctrl Pts',(47.2703848519362,-14.7669045823054,32.4794795677955));
#25579=CARTESIAN_POINT('Ctrl Pts',(47.3217202935107,-14.6768299128519,32.1923234499164));
#25580=CARTESIAN_POINT('Ctrl Pts',(47.3886116492137,-14.7669045823039,32.2741675910805));
#25581=CARTESIAN_POINT('Ctrl Pts',(47.4871835016963,-14.7669045823054,32.3766099734313));
#25582=CARTESIAN_POINT('Ctrl Pts',(47.3673683496366,-14.6796363815825,32.0810224279246));
#25583=CARTESIAN_POINT('Ctrl Pts',(47.4538839948076,-14.7669045823063,32.1097343017417));
#25584=CARTESIAN_POINT('Ctrl Pts',(47.5723707391893,-14.7669045823054,32.1528630624247));
#25585=CARTESIAN_POINT('Origin',(46.5214090713319,-14.4544045823054,32.4564357525968));
#25586=CARTESIAN_POINT('Ctrl Pts',(47.3365522275749,-14.6753754514101,32.1308553965272));
#25587=CARTESIAN_POINT('Ctrl Pts',(47.3288511935299,-14.6738626255535,32.1395148208736));
#25588=CARTESIAN_POINT('Ctrl Pts',(47.3204694543763,-14.672133306496,32.1473732471581));
#25589=CARTESIAN_POINT('Ctrl Pts',(47.3115921752356,-14.6701816478973,32.1544833559118));
#25590=CARTESIAN_POINT('Ctrl Pts',(47.3024303523205,-14.6681674327095,32.1618213652585));
#25591=CARTESIAN_POINT('Ctrl Pts',(47.2927409984408,-14.6659157786114,32.1683633490873));
#25592=CARTESIAN_POINT('Ctrl Pts',(47.2826925623907,-14.6634429331545,32.1742040106302));
#25593=CARTESIAN_POINT('Ctrl Pts',(47.2720840164946,-14.6608322488258,32.1803702364718));
#25594=CARTESIAN_POINT('Ctrl Pts',(47.2610753316299,-14.6579745808512,32.1857558736056));
#25595=CARTESIAN_POINT('Ctrl Pts',(47.249822974311,-14.654922626477,32.1904958266184));
#25596=CARTESIAN_POINT('Ctrl Pts',(47.2381991868033,-14.6517699298355,32.1953922412145));
#25597=CARTESIAN_POINT('Ctrl Pts',(47.2263150294869,-14.6484098887065,32.1996007485996));
#25598=CARTESIAN_POINT('Ctrl Pts',(47.2143018980764,-14.6449389709829,32.203276757552));
#25599=CARTESIAN_POINT('Ctrl Pts',(47.2017394876037,-14.6413093517213,32.2071208454741));
#25600=CARTESIAN_POINT('Ctrl Pts',(47.1890355849868,-14.6375586122335,32.2103836120104));
#25601=CARTESIAN_POINT('Ctrl Pts',(47.1763025037334,-14.6338375655308,32.213233443221));
#25602=CARTESIAN_POINT('Ctrl Pts',(47.1737601155823,-14.6330945917872,32.2138024631588));
#25603=CARTESIAN_POINT('Ctrl Pts',(47.1712164612877,-14.6323529212115,32.2143549657298));
#25604=CARTESIAN_POINT('Ctrl Pts',(47.1686722902479,-14.6316139267952,32.2148922001907));
#25605=CARTESIAN_POINT('Ctrl Pts',(47.1511506028079,-14.6265244776268,32.2185921300137));
#25606=CARTESIAN_POINT('Ctrl Pts',(47.1334820998403,-14.6213443098223,32.2214605564035));
#25607=CARTESIAN_POINT('Ctrl Pts',(47.1157563330173,-14.6160583702064,32.2236226908213));
#25608=CARTESIAN_POINT('Ctrl Pts',(47.097382295013,-14.6105791118837,32.2258638993602));
#25609=CARTESIAN_POINT('Ctrl Pts',(47.0789461280096,-14.6049864174423,32.2273473716443));
#25610=CARTESIAN_POINT('Ctrl Pts',(47.0605081098987,-14.5993048356876,32.2282053347277));
#25611=CARTESIAN_POINT('Ctrl Pts',(47.0410799411183,-14.5933181440265,32.2291093717826));
#25612=CARTESIAN_POINT('Ctrl Pts',(47.0216489808795,-14.5872331623026,32.2293199157884));
#25613=CARTESIAN_POINT('Ctrl Pts',(47.0022532252739,-14.5811189364151,32.2289664413872));
#25614=CARTESIAN_POINT('Ctrl Pts',(46.9957233691671,-14.579060495586,32.2288474392187));
#25615=CARTESIAN_POINT('Ctrl Pts',(46.9891972935831,-14.5769990339995,32.2286642430615));
#25616=CARTESIAN_POINT('Ctrl Pts',(46.9826759110969,-14.5749379971501,32.2284209330324));
#25617=CARTESIAN_POINT('Ctrl Pts',(46.9572265784279,-14.5668949154057,32.2274714291682));
#25618=CARTESIAN_POINT('Ctrl Pts',(46.931861218954,-14.5588253828872,32.2255941220409));
#25619=CARTESIAN_POINT('Ctrl Pts',(46.9066155065142,-14.5507005312868,32.2229083201426));
#25620=CARTESIAN_POINT('Ctrl Pts',(46.8790846852559,-14.541840260946,32.2199794136135));
#25621=CARTESIAN_POINT('Ctrl Pts',(46.8516950608053,-14.5329148917791,32.2160902190248));
#25622=CARTESIAN_POINT('Ctrl Pts',(46.824464099245,-14.5239279943211,32.2113568491449));
#25623=CARTESIAN_POINT('Ctrl Pts',(46.7960547265605,-14.5145521917591,32.2064186442022));
#25624=CARTESIAN_POINT('Ctrl Pts',(46.7678165411628,-14.5051108161017,32.2005618978972));
#25625=CARTESIAN_POINT('Ctrl Pts',(46.739760685689,-14.4956334644481,32.1938663766911));
#25626=CARTESIAN_POINT('Ctrl Pts',(46.7105476404483,-14.48576521064,32.1868946925061));
#25627=CARTESIAN_POINT('Ctrl Pts',(46.6815308177066,-14.4758595759461,32.1790130518177));
#25628=CARTESIAN_POINT('Ctrl Pts',(46.6527371605959,-14.4659531415139,32.1702582008432));
#25629=CARTESIAN_POINT('Ctrl Pts',(46.6415474723804,-14.4621033383368,32.1668559219176));
#25630=CARTESIAN_POINT('Ctrl Pts',(46.6303917529274,-14.4582533144083,32.1633212693771));
#25631=CARTESIAN_POINT('Ctrl Pts',(46.6192727816467,-14.4544045595309,32.1596547825137));
#25632=CARTESIAN_POINT('Ctrl Pts',(46.8756079148278,-13.2959337131847,30.3286338949779));
#25633=CARTESIAN_POINT('Ctrl Pts',(46.7987395491116,-13.2044045823055,30.2789465107479));
#25634=CARTESIAN_POINT('Ctrl Pts',(46.6900312637983,-13.2044045823055,30.208677938091));
#25635=CARTESIAN_POINT('Ctrl Pts',(46.92843243666,-13.2959337183951,30.2469122618309));
#25636=CARTESIAN_POINT('Ctrl Pts',(46.8409103036131,-13.2092798238961,30.2226873530845));
#25637=CARTESIAN_POINT('Ctrl Pts',(46.7280932516454,-13.2044045823055,30.1716843588109));
#25638=CARTESIAN_POINT('Ctrl Pts',(46.9609035199605,-13.2734166054794,30.1546855181066));
#25639=CARTESIAN_POINT('Ctrl Pts',(46.8649125651919,-13.1931723515307,30.1556415155577));
#25640=CARTESIAN_POINT('Ctrl Pts',(46.7449795511239,-13.1931460297457,30.1261487195746));
#25641=CARTESIAN_POINT('Ctrl Pts',(46.9737602628944,-13.1901047283843,29.9799549937871));
#25642=CARTESIAN_POINT('Ctrl Pts',(46.8644616166491,-13.126047486873,30.0321632131418));
#25643=CARTESIAN_POINT('Ctrl Pts',(46.7309855396157,-13.1514900886124,30.0323613044136));
#25644=CARTESIAN_POINT('Ctrl Pts',(46.9552502383954,-13.1321577745915,29.901072349635));
#25645=CARTESIAN_POINT('Ctrl Pts',(46.8409166506036,-13.076707210209,29.9774630678603));
#25646=CARTESIAN_POINT('Ctrl Pts',(46.7015662774492,-13.1225166214136,29.9863856596473));
#25647=CARTESIAN_POINT('Ctrl Pts',(46.8583542680918,-12.9456232578405,29.7057221755481));
#25648=CARTESIAN_POINT('Ctrl Pts',(46.7341681938515,-12.9177593310992,29.8496415056206));
#25649=CARTESIAN_POINT('Ctrl Pts',(46.5801991147773,-13.0292493378239,29.8648950373845));
#25650=CARTESIAN_POINT('Ctrl Pts',(46.7403255599353,-12.8021218234308,29.6238045764194));
#25651=CARTESIAN_POINT('Ctrl Pts',(46.6127393034986,-12.7965826300641,29.8149715922655));
#25652=CARTESIAN_POINT('Ctrl Pts',(46.4557286211812,-12.9574790903504,29.802364931387));
#25653=CARTESIAN_POINT('Ctrl Pts',(46.611780876039,-12.6709337131846,29.5815526781396));
#25654=CARTESIAN_POINT('Ctrl Pts',(46.5008548189629,-12.7034528674627,29.8172453197959));
#25655=CARTESIAN_POINT('Ctrl Pts',(46.3272934177549,-12.8919045823054,29.7600133527852));
#25656=CARTESIAN_POINT('Origin',(46.6900312637982,-13.5169045823054,30.2086779380909));
#25657=CARTESIAN_POINT('Ctrl Pts',(46.3272934177549,-12.8919045823054,29.7600133527852));
#25658=CARTESIAN_POINT('Ctrl Pts',(46.3510582803902,-12.9040380872518,29.7678498292419));
#25659=CARTESIAN_POINT('Ctrl Pts',(46.3744908825881,-12.9162817766913,29.7763081787903));
#25660=CARTESIAN_POINT('Ctrl Pts',(46.3975595440145,-12.928642750848,29.7854378206903));
#25661=CARTESIAN_POINT('Ctrl Pts',(46.4180047368047,-12.9395979811943,29.7935291999558));
#25662=CARTESIAN_POINT('Ctrl Pts',(46.4381656146539,-12.9506462200823,29.8021486241306));
#25663=CARTESIAN_POINT('Ctrl Pts',(46.4580019948025,-12.9617976021836,29.8113620702633));
#25664=CARTESIAN_POINT('Ctrl Pts',(46.4763437466883,-12.9721087518064,29.8198813031936));
#25665=CARTESIAN_POINT('Ctrl Pts',(46.494408944746,-12.9825085406161,29.8289087144576));
#25666=CARTESIAN_POINT('Ctrl Pts',(46.512133587223,-12.9930011868727,29.8385186549454));
#25667=CARTESIAN_POINT('Ctrl Pts',(46.5287360724235,-13.0028295376794,29.8475201845917));
#25668=CARTESIAN_POINT('Ctrl Pts',(46.545040388102,-13.0127396637185,29.8570329809913));
#25669=CARTESIAN_POINT('Ctrl Pts',(46.5609542191196,-13.0227264646561,29.8671353539293));
#25670=CARTESIAN_POINT('Ctrl Pts',(46.5756034413391,-13.0319196542807,29.8764349315074));
#25671=CARTESIAN_POINT('Ctrl Pts',(46.5899220587733,-13.0411779829359,29.8862342539382));
#25672=CARTESIAN_POINT('Ctrl Pts',(46.6037973990955,-13.050486888578,29.8966073103123));
#25673=CARTESIAN_POINT('Ctrl Pts',(46.6109666672577,-13.0552967194935,29.9019669786938));
#25674=CARTESIAN_POINT('Ctrl Pts',(46.6180168846007,-13.0601198606027,29.9074800216699));
#25675=CARTESIAN_POINT('Ctrl Pts',(46.6249272899651,-13.064952825595,29.913157992511));
#25676=CARTESIAN_POINT('Ctrl Pts',(46.6354219377737,-13.0722925202713,29.9217809749703));
#25677=CARTESIAN_POINT('Ctrl Pts',(46.6455357175484,-13.0796093213736,29.9307303372787));
#25678=CARTESIAN_POINT('Ctrl Pts',(46.6552437527905,-13.0869314629286,29.9400978119362));
#25679=CARTESIAN_POINT('Ctrl Pts',(46.657225258145,-13.0884259839451,29.94200980553));
#25680=CARTESIAN_POINT('Ctrl Pts',(46.6591897022381,-13.0899206854313,29.9439392731158));
#25681=CARTESIAN_POINT('Ctrl Pts',(46.6611366181773,-13.091415738093,29.9458870799904));
#25682=CARTESIAN_POINT('Ctrl Pts',(46.6690767883509,-13.0975130596636,29.9538308836947));
#25683=CARTESIAN_POINT('Ctrl Pts',(46.6767231203679,-13.1036283475445,29.9621128151418));
#25684=CARTESIAN_POINT('Ctrl Pts',(46.6839712973621,-13.1097352160117,29.9707640545256));
#25685=CARTESIAN_POINT('Ctrl Pts',(46.6908187716549,-13.1155044770096,29.9789370253745));
#25686=CARTESIAN_POINT('Ctrl Pts',(46.6973113229118,-13.1212664690668,29.9874398372937));
#25687=CARTESIAN_POINT('Ctrl Pts',(46.7033197908501,-13.1269828032025,29.9962982353705));
#25688=CARTESIAN_POINT('Ctrl Pts',(46.708869254037,-13.1322624495576,30.0044799140491));
#25689=CARTESIAN_POINT('Ctrl Pts',(46.7140059302817,-13.1375032622583,30.0129650894761));
#25690=CARTESIAN_POINT('Ctrl Pts',(46.7185881839945,-13.1426584957564,30.021770855088));
#25691=CARTESIAN_POINT('Ctrl Pts',(46.7220537204315,-13.1465573740482,30.0284306132541));
#25692=CARTESIAN_POINT('Ctrl Pts',(46.7252014487815,-13.1504070236376,30.0352737091184));
#25693=CARTESIAN_POINT('Ctrl Pts',(46.7279518132448,-13.1541794056116,30.0423052686843));
#25694=CARTESIAN_POINT('Ctrl Pts',(46.732511491481,-13.1604334305654,30.053962505224));
#25695=CARTESIAN_POINT('Ctrl Pts',(46.7360832461396,-13.1665823184279,30.0663511701297));
#25696=CARTESIAN_POINT('Ctrl Pts',(46.7380257804305,-13.1723138052614,30.0792601551115));
#25697=CARTESIAN_POINT('Ctrl Pts',(46.7394171453584,-13.1764190557076,30.0885063800258));
#25698=CARTESIAN_POINT('Ctrl Pts',(46.7399127125584,-13.1802529865566,30.0979299368269));
#25699=CARTESIAN_POINT('Ctrl Pts',(46.7394048359389,-13.1837286680709,30.1074032472023));
#25700=CARTESIAN_POINT('Ctrl Pts',(46.7390261893497,-13.1863199567817,30.1144660583743));
#25701=CARTESIAN_POINT('Ctrl Pts',(46.7380907473884,-13.1887123032026,30.1215561565728));
#25702=CARTESIAN_POINT('Ctrl Pts',(46.736571681541,-13.1908748315003,30.128616804082));
#25703=CARTESIAN_POINT('Ctrl Pts',(46.7347953705731,-13.1934035716073,30.1368731318983));
#25704=CARTESIAN_POINT('Ctrl Pts',(46.7322325088647,-13.1955933528871,30.1450105858529));
#25705=CARTESIAN_POINT('Ctrl Pts',(46.7289332541082,-13.1974205800258,30.152924044601));
#25706=CARTESIAN_POINT('Ctrl Pts',(46.7256175087789,-13.1992569401429,30.1608770569688));
#25707=CARTESIAN_POINT('Ctrl Pts',(46.7215582129827,-13.2007270768473,30.1686033690315));
#25708=CARTESIAN_POINT('Ctrl Pts',(46.7168512222028,-13.2018302796858,30.1760119191985));
#25709=CARTESIAN_POINT('Ctrl Pts',(46.7120681506037,-13.2029513139965,30.1835402164805));
#25710=CARTESIAN_POINT('Ctrl Pts',(46.7066165411459,-13.2036934504427,30.1907399768785));
#25711=CARTESIAN_POINT('Ctrl Pts',(46.7006396922035,-13.2040802847478,30.1975385766591));
#25712=CARTESIAN_POINT('Ctrl Pts',(46.6972603068424,-13.204299005716,30.2013825902514));
#25713=CARTESIAN_POINT('Ctrl Pts',(46.6937137589004,-13.2044045823055,30.2050988114553));
#25714=CARTESIAN_POINT('Ctrl Pts',(46.6900312637983,-13.2044045823055,30.208677938091));
#25715=CARTESIAN_POINT('Ctrl Pts',(40.153012388794,-6.10843371318469,27.4594837601833));
#25716=CARTESIAN_POINT('Ctrl Pts',(40.0774385461352,-6.01690458230548,27.4078487322925));
#25717=CARTESIAN_POINT('Ctrl Pts',(40.0774385461352,-5.88746284406389,27.4078487322925));
#25718=CARTESIAN_POINT('Ctrl Pts',(40.1242331962091,-6.1027501834569,27.4915307194576));
#25719=CARTESIAN_POINT('Ctrl Pts',(40.0445399338239,-6.01222811250157,27.4559996605526));
#25720=CARTESIAN_POINT('Ctrl Pts',(40.03154277396,-5.88746285448661,27.4750225096052));
#25721=CARTESIAN_POINT('Ctrl Pts',(40.1009218644572,-6.11419577460901,27.5251818602439));
#25722=CARTESIAN_POINT('Ctrl Pts',(40.0112197519127,-6.02882146164764,27.5045867865534));
#25723=CARTESIAN_POINT('Ctrl Pts',(39.9853851293292,-5.9106557086834,27.5421815181704));
#25724=CARTESIAN_POINT('Ctrl Pts',(40.0720849274312,-6.1677431863177,27.5858654582369));
#25725=CARTESIAN_POINT('Ctrl Pts',(39.9576202879931,-6.0978035275072,27.5825741675642));
#25726=CARTESIAN_POINT('Ctrl Pts',(39.9069533697846,-5.99623773973419,27.655803900523));
#25727=CARTESIAN_POINT('Ctrl Pts',(40.066209509497,-6.20950986590618,27.6131711938117));
#25728=CARTESIAN_POINT('Ctrl Pts',(39.9366893821544,-6.15046547604274,27.6129453446739));
#25729=CARTESIAN_POINT('Ctrl Pts',(39.8741328667897,-6.05824038173977,27.7030926868508));
#25730=CARTESIAN_POINT('Ctrl Pts',(40.0694547712359,-6.3546301407075,27.6798043375759));
#25731=CARTESIAN_POINT('Ctrl Pts',(39.8956196052046,-6.32861804115437,27.6726104606096));
#25732=CARTESIAN_POINT('Ctrl Pts',(39.8004265980845,-6.26685602924677,27.8090735783451));
#25733=CARTESIAN_POINT('Ctrl Pts',(40.0973050091181,-6.47617237885447,27.7056712663594));
#25734=CARTESIAN_POINT('Ctrl Pts',(39.8976526694977,-6.47276044373899,27.6698898995951));
#25735=CARTESIAN_POINT('Ctrl Pts',(39.7815264643901,-6.43425950785913,27.8359939147546));
#25736=CARTESIAN_POINT('Ctrl Pts',(40.1355062937731,-6.59535043767467,27.7182681608758));
#25737=CARTESIAN_POINT('Ctrl Pts',(39.9147276464474,-6.59535043767467,27.6454662811233));
#25738=CARTESIAN_POINT('Ctrl Pts',(39.7815264758118,-6.59535043767467,27.8359938984173));
#25739=CARTESIAN_POINT('Ctrl Pts',(-46.7085547781037,-13.2959337131847,
-30.163770311099));
#25740=CARTESIAN_POINT('Ctrl Pts',(-46.6316864123875,-13.2044045823055,
-30.114082926869));
#25741=CARTESIAN_POINT('Ctrl Pts',(-46.5229781270742,-13.2044045823055,
-30.0438143542121));
#25742=CARTESIAN_POINT('Ctrl Pts',(-46.761379299936,-13.2959337183952,-30.0820486779521));
#25743=CARTESIAN_POINT('Ctrl Pts',(-46.673857166889,-13.2092798238962,-30.057823769206));
#25744=CARTESIAN_POINT('Ctrl Pts',(-46.5610401149215,-13.2044045823055,
-30.0068207749323));
#25745=CARTESIAN_POINT('Ctrl Pts',(-46.7938503832366,-13.2734166054797,
-29.9898219342279));
#25746=CARTESIAN_POINT('Ctrl Pts',(-46.6978594284684,-13.1931723515309,
-29.9907779316791));
#25747=CARTESIAN_POINT('Ctrl Pts',(-46.5779264144001,-13.1931460297457,
-29.961285135696));
#25748=CARTESIAN_POINT('Ctrl Pts',(-46.8067071261701,-13.1901047283841,
-29.8150914099081));
#25749=CARTESIAN_POINT('Ctrl Pts',(-46.6974084799243,-13.1260474868728,
-29.8672996292628));
#25750=CARTESIAN_POINT('Ctrl Pts',(-46.5639324028913,-13.1514900886123,
-29.8674977205345));
#25751=CARTESIAN_POINT('Ctrl Pts',(-46.7881971016712,-13.1321577745915,
-29.7362087657564));
#25752=CARTESIAN_POINT('Ctrl Pts',(-46.6738635138795,-13.0767072102089,
-29.8125994839813));
#25753=CARTESIAN_POINT('Ctrl Pts',(-46.5345131407245,-13.1225166214137,
-29.8215220757683));
#25754=CARTESIAN_POINT('Ctrl Pts',(-46.691301131368,-12.9456232578405,-29.5408585916687));
#25755=CARTESIAN_POINT('Ctrl Pts',(-46.5671150571274,-12.9177593310994,
-29.684777921742));
#25756=CARTESIAN_POINT('Ctrl Pts',(-46.4131459780545,-13.0292493378237,
-29.7000314535059));
#25757=CARTESIAN_POINT('Ctrl Pts',(-46.5732724232098,-12.8021218234311,
-29.4589409925433));
#25758=CARTESIAN_POINT('Ctrl Pts',(-46.4456861667736,-12.7965826300651,
-29.6501080083888));
#25759=CARTESIAN_POINT('Ctrl Pts',(-46.2886754844563,-12.9574790903503,
-29.6375013475079));
#25760=CARTESIAN_POINT('Ctrl Pts',(-46.4447277393149,-12.6709337131846,
-29.4166890942607));
#25761=CARTESIAN_POINT('Ctrl Pts',(-46.3338016822388,-12.7034528674627,
-29.6523817359171));
#25762=CARTESIAN_POINT('Ctrl Pts',(-46.1602402810308,-12.8919045823054,
-29.5951497689063));
#25763=CARTESIAN_POINT('Origin',(-46.5229781270741,-13.5169045823054,-30.0438143542121));
#25764=CARTESIAN_POINT('Ctrl Pts',(-46.1602402810308,-12.8919045823054,
-29.5951497689063));
#25765=CARTESIAN_POINT('Ctrl Pts',(-46.1840051436653,-12.9040380872515,
-29.6029862453627));
#25766=CARTESIAN_POINT('Ctrl Pts',(-46.2074377458625,-12.9162817766905,
-29.6114445949109));
#25767=CARTESIAN_POINT('Ctrl Pts',(-46.2305064072882,-12.9286427508468,
-29.6205742368105));
#25768=CARTESIAN_POINT('Ctrl Pts',(-46.2509516000786,-12.9395979811933,
-29.6286656160761));
#25769=CARTESIAN_POINT('Ctrl Pts',(-46.271112477928,-12.9506462200813,-29.6372850402509));
#25770=CARTESIAN_POINT('Ctrl Pts',(-46.2909488580768,-12.9617976021827,
-29.6464984863837));
#25771=CARTESIAN_POINT('Ctrl Pts',(-46.3092906099622,-12.9721087518052,
-29.6550177193137));
#25772=CARTESIAN_POINT('Ctrl Pts',(-46.3273558080195,-12.9825085406146,
-29.6640451305775));
#25773=CARTESIAN_POINT('Ctrl Pts',(-46.3450804504962,-12.9930011868708,
-29.673655071065));
#25774=CARTESIAN_POINT('Ctrl Pts',(-46.3616829356962,-13.0028295376772,
-29.6826566007109));
#25775=CARTESIAN_POINT('Ctrl Pts',(-46.3779872513743,-13.012739663716,-29.6921693971101));
#25776=CARTESIAN_POINT('Ctrl Pts',(-46.3939010823914,-13.0227264646533,
-29.7022717700477));
#25777=CARTESIAN_POINT('Ctrl Pts',(-46.4085503046105,-13.0319196542775,
-29.7115713476254));
#25778=CARTESIAN_POINT('Ctrl Pts',(-46.4228689220442,-13.0411779829323,
-29.7213706700557));
#25779=CARTESIAN_POINT('Ctrl Pts',(-46.436744262366,-13.0504868885741,-29.7317437264293));
#25780=CARTESIAN_POINT('Ctrl Pts',(-46.4439135305301,-13.0552967194909,
-29.7371033948121));
#25781=CARTESIAN_POINT('Ctrl Pts',(-46.450963747875,-13.0601198606014,-29.7426164377896));
#25782=CARTESIAN_POINT('Ctrl Pts',(-46.4578741532412,-13.0649528255949,
-29.7482944086321));
#25783=CARTESIAN_POINT('Ctrl Pts',(-46.4683688010496,-13.0722925202711,
-29.7569173910913));
#25784=CARTESIAN_POINT('Ctrl Pts',(-46.4784825808242,-13.0796093213733,
-29.7658667533996));
#25785=CARTESIAN_POINT('Ctrl Pts',(-46.488190616066,-13.0869314629283,-29.7752342280569));
#25786=CARTESIAN_POINT('Ctrl Pts',(-46.4901721214206,-13.0884259839449,
-29.7771462216509));
#25787=CARTESIAN_POINT('Ctrl Pts',(-46.4921365655139,-13.0899206854312,
-29.7790756892368));
#25788=CARTESIAN_POINT('Ctrl Pts',(-46.4940834814532,-13.091415738093,-29.7810234961116));
#25789=CARTESIAN_POINT('Ctrl Pts',(-46.5020236516268,-13.0975130596636,
-29.7889672998159));
#25790=CARTESIAN_POINT('Ctrl Pts',(-46.5096699836439,-13.1036283475445,
-29.797249231263));
#25791=CARTESIAN_POINT('Ctrl Pts',(-46.516918160638,-13.1097352160118,-29.8059004706468));
#25792=CARTESIAN_POINT('Ctrl Pts',(-46.5237656349308,-13.1155044770098,
-29.8140734414958));
#25793=CARTESIAN_POINT('Ctrl Pts',(-46.5302581861878,-13.1212664690669,
-29.822576253415));
#25794=CARTESIAN_POINT('Ctrl Pts',(-46.5362666541262,-13.1269828032027,
-29.8314346514919));
#25795=CARTESIAN_POINT('Ctrl Pts',(-46.5418161173131,-13.1322624495578,
-29.8396163301706));
#25796=CARTESIAN_POINT('Ctrl Pts',(-46.5469527935578,-13.1375032622586,
-29.8481015055977));
#25797=CARTESIAN_POINT('Ctrl Pts',(-46.5515350472707,-13.1426584957567,
-29.8569072712097));
#25798=CARTESIAN_POINT('Ctrl Pts',(-46.5550005837076,-13.1465573740484,
-29.8635670293756));
#25799=CARTESIAN_POINT('Ctrl Pts',(-46.5581483120574,-13.1504070236377,
-29.8704101252397));
#25800=CARTESIAN_POINT('Ctrl Pts',(-46.5608986765207,-13.1541794056116,
-29.8774416848054));
#25801=CARTESIAN_POINT('Ctrl Pts',(-46.5654583547569,-13.1604334305654,
-29.8890989213451));
#25802=CARTESIAN_POINT('Ctrl Pts',(-46.5690301094155,-13.1665823184279,
-29.9014875862509));
#25803=CARTESIAN_POINT('Ctrl Pts',(-46.5709726437064,-13.1723138052614,
-29.9143965712326));
#25804=CARTESIAN_POINT('Ctrl Pts',(-46.5723640086343,-13.1764190557077,
-29.9236427961473));
#25805=CARTESIAN_POINT('Ctrl Pts',(-46.5728595758343,-13.1802529865569,
-29.9330663529488));
#25806=CARTESIAN_POINT('Ctrl Pts',(-46.5723516992147,-13.1837286680714,
-29.9425396633246));
#25807=CARTESIAN_POINT('Ctrl Pts',(-46.5719730526255,-13.186319956782,-29.9496024744962));
#25808=CARTESIAN_POINT('Ctrl Pts',(-46.5710376106642,-13.1887123032027,
-29.9566925726943));
#25809=CARTESIAN_POINT('Ctrl Pts',(-46.5695185448169,-13.1908748315003,
-29.9637532202032));
#25810=CARTESIAN_POINT('Ctrl Pts',(-46.567742233849,-13.1934035716073,-29.9720095480195));
#25811=CARTESIAN_POINT('Ctrl Pts',(-46.5651793721406,-13.1955933528871,
-29.980147001974));
#25812=CARTESIAN_POINT('Ctrl Pts',(-46.5618801173841,-13.1974205800258,
-29.9880604607222));
#25813=CARTESIAN_POINT('Ctrl Pts',(-46.5585643720548,-13.1992569401429,
-29.99601347309));
#25814=CARTESIAN_POINT('Ctrl Pts',(-46.5545050762587,-13.2007270768473,
-30.0037397851527));
#25815=CARTESIAN_POINT('Ctrl Pts',(-46.5497980854788,-13.2018302796858,
-30.0111483353198));
#25816=CARTESIAN_POINT('Ctrl Pts',(-46.5450150138797,-13.2029513139966,
-30.0186766326018));
#25817=CARTESIAN_POINT('Ctrl Pts',(-46.5395634044218,-13.2036934504427,
-30.0258763929997));
#25818=CARTESIAN_POINT('Ctrl Pts',(-46.5335865554794,-13.2040802847478,
-30.0326749927803));
#25819=CARTESIAN_POINT('Ctrl Pts',(-46.5302071701183,-13.204299005716,-30.0365190063726));
#25820=CARTESIAN_POINT('Ctrl Pts',(-46.5266606221764,-13.2044045823055,
-30.0402352275765));
#25821=CARTESIAN_POINT('Ctrl Pts',(-46.5229781270742,-13.2044045823055,
-30.0438143542121));
#25822=CARTESIAN_POINT('Ctrl Pts',(-39.9859592520697,-6.10843371318464,
-27.2946201763047));
#25823=CARTESIAN_POINT('Ctrl Pts',(-39.9103854094108,-6.01690458230545,
-27.242985148414));
#25824=CARTESIAN_POINT('Ctrl Pts',(-39.9103854094107,-5.88746284406389,
-27.2429851484142));
#25825=CARTESIAN_POINT('Ctrl Pts',(-39.9571800594855,-6.1027501834571,-27.3266671355783));
#25826=CARTESIAN_POINT('Ctrl Pts',(-39.8774867971012,-6.01222811250108,
-27.2911360766742));
#25827=CARTESIAN_POINT('Ctrl Pts',(-39.8644896372362,-5.88746285448629,
-27.3101589257258));
#25828=CARTESIAN_POINT('Ctrl Pts',(-39.9338687277324,-6.11419577460858,
-27.3603182763651));
#25829=CARTESIAN_POINT('Ctrl Pts',(-39.844166615188,-6.02882146164754,-27.3397232026743));
#25830=CARTESIAN_POINT('Ctrl Pts',(-39.8183319926051,-5.91065570868315,
-27.3773179342917));
#25831=CARTESIAN_POINT('Ctrl Pts',(-39.9050317907078,-6.16774318631813,
-27.421001874358));
#25832=CARTESIAN_POINT('Ctrl Pts',(-39.7905671512696,-6.09780352750732,
-27.4177105836857));
#25833=CARTESIAN_POINT('Ctrl Pts',(-39.7399002330605,-5.99623773973444,
-27.4909403166441));
#25834=CARTESIAN_POINT('Ctrl Pts',(-39.8991563727726,-6.20950986590617,
-27.4483076099329));
#25835=CARTESIAN_POINT('Ctrl Pts',(-39.7696362454303,-6.15046547604259,
-27.4480817607952));
#25836=CARTESIAN_POINT('Ctrl Pts',(-39.7070797300657,-6.05824038173967,
-27.5382291029718));
#25837=CARTESIAN_POINT('Ctrl Pts',(-39.9024016345124,-6.35463014070754,
-27.514940753697));
#25838=CARTESIAN_POINT('Ctrl Pts',(-39.7285664684805,-6.32861804115478,
-27.5077468767305));
#25839=CARTESIAN_POINT('Ctrl Pts',(-39.6333734613603,-6.26685602924698,
-27.6442099944664));
#25840=CARTESIAN_POINT('Ctrl Pts',(-39.930251872391,-6.47617237885538,-27.5408076824795));
#25841=CARTESIAN_POINT('Ctrl Pts',(-39.7305995327717,-6.47276044373959,
-27.5050263157192));
#25842=CARTESIAN_POINT('Ctrl Pts',(-39.6144733276653,-6.43425950785897,
-27.6711303308768));
#25843=CARTESIAN_POINT('Ctrl Pts',(-39.968453157049,-6.59535043767467,-27.553404576997));
#25844=CARTESIAN_POINT('Ctrl Pts',(-39.7476745097234,-6.59535043767467,
-27.4806026972444));
#25845=CARTESIAN_POINT('Ctrl Pts',(-39.6144733390877,-6.59535043767467,
-27.6711303145384));
#25846=CARTESIAN_POINT('Origin',(-40.1684106479774,-5.8874628440639,-27.419278160932));
#25847=CARTESIAN_POINT('Origin',(-39.8705894675228,-6.59535043767467,-27.8501855539351));
#25848=CARTESIAN_POINT('Origin',(0.0835265683620477,-13.5169045823054,0.0824317919394229));
#25849=CARTESIAN_POINT('Origin',(-45.6231018412815,-13.5169045823054,-31.3923375671359));
#25850=CARTESIAN_POINT('Origin',(4.47264233855679,-12.8919045823054,-13.2279806039107));
#25851=CARTESIAN_POINT('Origin',(-39.8705894675228,-12.8919045823054,-27.8501855539351));
#25852=CARTESIAN_POINT('Origin',(-39.8705894675228,-14.7669045823054,-27.8501855539351));
#25853=CARTESIAN_POINT('Origin',(-39.8705894675228,-12.8919045823054,-27.8501855539351));
#25854=CARTESIAN_POINT('Origin',(0.0835265683620477,-12.8919045823054,0.0824317919394229));
#25855=CARTESIAN_POINT('Ctrl Pts',(-34.1929414312581,-13.2044045823054,
-34.5829146143929));
#25856=CARTESIAN_POINT('Ctrl Pts',(-34.1680403069389,-13.2044045823054,
-34.5830483771525));
#25857=CARTESIAN_POINT('Ctrl Pts',(-34.1434060402122,-13.2030022087212,
-34.5831873558775));
#25858=CARTESIAN_POINT('Ctrl Pts',(-34.1189478462075,-13.2001447338013,
-34.5833336044956));
#25859=CARTESIAN_POINT('Ctrl Pts',(-34.094935431709,-13.1973393397406,-34.5834771875598));
#25860=CARTESIAN_POINT('Ctrl Pts',(-34.071092686807,-13.193131465653,-34.5836278043066));
#25861=CARTESIAN_POINT('Ctrl Pts',(-34.0473441304472,-13.1874220362844,
-34.5837878944019));
#25862=CARTESIAN_POINT('Ctrl Pts',(-34.0414387028137,-13.1860023027455,
-34.5838277031574));
#25863=CARTESIAN_POINT('Ctrl Pts',(-34.0355391523601,-13.184489476873,-34.5838680990468));
#25864=CARTESIAN_POINT('Ctrl Pts',(-34.0296444264616,-13.1828815404475,
-34.5839091214968));
#25865=CARTESIAN_POINT('Ctrl Pts',(-34.0075950038454,-13.1768669995857,
-34.5840625673653));
#25866=CARTESIAN_POINT('Ctrl Pts',(-33.9861383901114,-13.1696750914267,
-34.5842210504987));
#25867=CARTESIAN_POINT('Ctrl Pts',(-33.9652968749802,-13.1611455958503,
-34.5843848815461));
#25868=CARTESIAN_POINT('Ctrl Pts',(-33.9444553598491,-13.1526161002739,
-34.5845487125934));
#25869=CARTESIAN_POINT('Ctrl Pts',(-33.9242285971081,-13.1427495299604,
-34.5847179161621));
#25870=CARTESIAN_POINT('Ctrl Pts',(-33.9046719627877,-13.1313389816383,
-34.5848921573841));
#25871=CARTESIAN_POINT('Ctrl Pts',(-33.8980736200928,-13.1274891009823,
-34.5849509457869));
#25872=CARTESIAN_POINT('Ctrl Pts',(-33.8915791335182,-13.1234784566375,
-34.5850085468875));
#25873=CARTESIAN_POINT('Ctrl Pts',(-33.8851706792542,-13.1192883941035,
-34.5850653658929));
#25874=CARTESIAN_POINT('Ctrl Pts',(-33.8744851575582,-13.1123018412982,
-34.5851601064793));
#25875=CARTESIAN_POINT('Ctrl Pts',(-33.86420405785,-13.104916612557,-34.5852512337119));
#25876=CARTESIAN_POINT('Ctrl Pts',(-33.854304863418,-13.0970443878827,-34.5853399947737));
#25877=CARTESIAN_POINT('Ctrl Pts',(-33.8506201662143,-13.0941141732634,
-34.585373033587));
#25878=CARTESIAN_POINT('Ctrl Pts',(-33.846988814313,-13.0911162306683,-34.5854057405226));
#25879=CARTESIAN_POINT('Ctrl Pts',(-33.843411289417,-13.088045086031,-34.5854381632075));
#25880=CARTESIAN_POINT('Ctrl Pts',(-33.8339347977663,-13.0799099430592,
-34.5855240475303));
#25881=CARTESIAN_POINT('Ctrl Pts',(-33.8248750204272,-13.071295025075,-34.585607570458));
#25882=CARTESIAN_POINT('Ctrl Pts',(-33.8163189539575,-13.0621639241565,
-34.5856851785447));
#25883=CARTESIAN_POINT('Ctrl Pts',(-33.8077628874879,-13.053032823238,-34.5857627866313));
#25884=CARTESIAN_POINT('Ctrl Pts',(-33.7997113740151,-13.0433849467635,
-34.5858333463418));
#25885=CARTESIAN_POINT('Ctrl Pts',(-33.7922539399743,-13.0331862397832,
-34.5859071947319));
#25886=CARTESIAN_POINT('Ctrl Pts',(-33.7886347380691,-13.0282366579925,
-34.5859430344366));
#25887=CARTESIAN_POINT('Ctrl Pts',(-33.7851501101384,-13.0231465710756,
-34.5859776488828));
#25888=CARTESIAN_POINT('Ctrl Pts',(-33.7818190947318,-13.0179182754031,
-34.5860108176103));
#25889=CARTESIAN_POINT('Ctrl Pts',(-33.7743334296083,-13.0061689239908,
-34.5860853564389));
#25890=CARTESIAN_POINT('Ctrl Pts',(-33.7677565298757,-12.993904917636,-34.5861511719067));
#25891=CARTESIAN_POINT('Ctrl Pts',(-33.7622772370354,-12.9812267133663,
-34.5862062450479));
#25892=CARTESIAN_POINT('Ctrl Pts',(-33.7569248855037,-12.9688422309121,
-34.5862600422842));
#25893=CARTESIAN_POINT('Ctrl Pts',(-33.7526202667613,-12.9560629035318,
-34.5863035817044));
#25894=CARTESIAN_POINT('Ctrl Pts',(-33.7494937045786,-12.9430006092192,
-34.5863353326885));
#25895=CARTESIAN_POINT('Ctrl Pts',(-33.7464514954637,-12.9302907290069,
-34.5863662270471));
#25896=CARTESIAN_POINT('Ctrl Pts',(-33.7445248498179,-12.9173133257079,
-34.5863859545434));
#25897=CARTESIAN_POINT('Ctrl Pts',(-33.7437856904794,-12.9041833323892,
-34.5863935387912));
#25898=CARTESIAN_POINT('Ctrl Pts',(-33.7435560357035,-12.9001038795344,
-34.5863958951962));
#25899=CARTESIAN_POINT('Ctrl Pts',(-33.7434406426353,-12.896009762608,-34.5863970829463));
#25900=CARTESIAN_POINT('Ctrl Pts',(-33.7434406426353,-12.8919045823054,
-34.5863970829463));
#25901=CARTESIAN_POINT('Origin',(7.03184852472011,-13.5169045823054,-20.9890175706648));
#25902=CARTESIAN_POINT('Origin',(-34.1929414312581,-13.5169045823054,-34.5829146143929));
#25903=CARTESIAN_POINT('Origin',(19.8255764196421,-11.3294045823054,-10.0436051386457));
#25904=CARTESIAN_POINT('Origin',(19.2694623393243,-11.3294045823054,-9.75836466172779));
#25905=CARTESIAN_POINT('Ctrl Pts',(34.2554728506688,-10.7044045823054,-34.2464116713807));
#25906=CARTESIAN_POINT('Ctrl Pts',(34.2554728506688,-11.0169045823054,-34.2464116713807));
#25907=CARTESIAN_POINT('Ctrl Pts',(34.0350086811056,-11.0169045823054,-34.02493526194));
#25908=CARTESIAN_POINT('Ctrl Pts',(34.3179692702965,-10.7044046073823,-34.1842008865451));
#25909=CARTESIAN_POINT('Ctrl Pts',(34.2942143893231,-11.034944931327,-34.2078471963309));
#25910=CARTESIAN_POINT('Ctrl Pts',(34.0599086143365,-11.0169045823054,-33.9753904270529));
#25911=CARTESIAN_POINT('Ctrl Pts',(34.3787106266475,-10.718650676671,-34.123396588746));
#25912=CARTESIAN_POINT('Ctrl Pts',(34.3266517180123,-11.063071415628,-34.1754830902681));
#25913=CARTESIAN_POINT('Ctrl Pts',(34.084059078646,-11.0240276257398,-33.9269149742339));
#25914=CARTESIAN_POINT('Ctrl Pts',(34.4961549499042,-10.7765752156551,-34.005239772344));
#25915=CARTESIAN_POINT('Ctrl Pts',(34.377889924456,-11.1314870357703,-34.1245297803838));
#25916=CARTESIAN_POINT('Ctrl Pts',(34.1306669722307,-11.0529899027286,-33.8326289586376));
#25917=CARTESIAN_POINT('Ctrl Pts',(34.5495749085591,-10.8185639645427,-33.95119120071));
#25918=CARTESIAN_POINT('Ctrl Pts',(34.3941245222472,-11.1704305366375,-34.1085208978415));
#25919=CARTESIAN_POINT('Ctrl Pts',(34.1518217449246,-11.0739842709863,-33.7894549020566));
#25920=CARTESIAN_POINT('Ctrl Pts',(34.6445000675177,-10.9314866347395,-33.8547910317575));
#25921=CARTESIAN_POINT('Ctrl Pts',(34.4101878971174,-11.2441510617714,-34.0933162668226));
#25922=CARTESIAN_POINT('Ctrl Pts',(34.1893600410275,-11.1304456109602,-33.7123980746659));
#25923=CARTESIAN_POINT('Ctrl Pts',(34.6830766509629,-10.999293715727,-33.8154157688772));
#25924=CARTESIAN_POINT('Ctrl Pts',(34.4081565684008,-11.2750326114058,-34.0959850824422));
#25925=CARTESIAN_POINT('Ctrl Pts',(34.2045857764074,-11.1643491474262,-33.6808947305844));
#25926=CARTESIAN_POINT('Ctrl Pts',(34.7377600096266,-11.1560957480195,-33.7595102293617));
#25927=CARTESIAN_POINT('Ctrl Pts',(34.3990150768359,-11.3160025899706,-34.1063442197293));
#25928=CARTESIAN_POINT('Ctrl Pts',(34.2261553564882,-11.2427501667525,-33.636152825177));
#25929=CARTESIAN_POINT('Ctrl Pts',(34.752355455618,-11.2411599901507,-33.7445354063799));
#25930=CARTESIAN_POINT('Ctrl Pts',(34.3930336310338,-11.3235538600012,-34.1127997789392));
#25931=CARTESIAN_POINT('Ctrl Pts',(34.2319046000613,-11.2852822850309,-33.6241606027471));
#25932=CARTESIAN_POINT('Ctrl Pts',(34.7523554432478,-11.3294045823054,-33.7445354190578));
#25933=CARTESIAN_POINT('Ctrl Pts',(34.3930336345113,-11.3294045823054,-34.112799775138));
#25934=CARTESIAN_POINT('Ctrl Pts',(34.2319046026008,-11.3294045823054,-33.6241606104485));
#25935=CARTESIAN_POINT('Ctrl Pts',(34.2319046026008,-11.3294045823054,-33.6241606104486));
#25936=CARTESIAN_POINT('Ctrl Pts',(34.2319046026008,-11.3159760597526,-33.6241606104486));
#25937=CARTESIAN_POINT('Ctrl Pts',(34.2313701235195,-11.3026664608407,-33.6252754613691));
#25938=CARTESIAN_POINT('Ctrl Pts',(34.2303262007385,-11.2895978753996,-33.6274497561314));
#25939=CARTESIAN_POINT('Ctrl Pts',(34.2292621420608,-11.2762772141441,-33.6296659901783));
#25940=CARTESIAN_POINT('Ctrl Pts',(34.2276689072531,-11.2632073639016,-33.6329826731796));
#25941=CARTESIAN_POINT('Ctrl Pts',(34.2255963210687,-11.2505062466188,-33.6372928524732));
#25942=CARTESIAN_POINT('Ctrl Pts',(34.2234556661661,-11.2373879940772,-33.641744588428));
#25943=CARTESIAN_POINT('Ctrl Pts',(34.2208037862985,-11.2246635682847,-33.6472558461806));
#25944=CARTESIAN_POINT('Ctrl Pts',(34.2177184383504,-11.212443933042,-33.6536619679777));
#25945=CARTESIAN_POINT('Ctrl Pts',(34.2169622262201,-11.2094489267884,-33.6552320946191));
#25946=CARTESIAN_POINT('Ctrl Pts',(34.2161800730707,-11.2064841392024,-33.6568557778232));
#25947=CARTESIAN_POINT('Ctrl Pts',(34.2153733079896,-11.2035509891889,-33.6585302199796));
#25948=CARTESIAN_POINT('Ctrl Pts',(34.2139688035159,-11.1984446423577,-33.6614452711567));
#25949=CARTESIAN_POINT('Ctrl Pts',(34.212499775488,-11.19346758092,-33.6644930487698));
#25950=CARTESIAN_POINT('Ctrl Pts',(34.2109735777768,-11.18862206557,-33.6676578884119));
#25951=CARTESIAN_POINT('Ctrl Pts',(34.2077635090097,-11.1784304387767,-33.6743145311349));
#25952=CARTESIAN_POINT('Ctrl Pts',(34.2042866771259,-11.1687879968701,-33.6814958205249));
#25953=CARTESIAN_POINT('Ctrl Pts',(34.2005926189786,-11.1596600078883,-33.6891304879687));
#25954=CARTESIAN_POINT('Ctrl Pts',(34.1964998574857,-11.149546826037,-33.697589172613));
#25955=CARTESIAN_POINT('Ctrl Pts',(34.1921518053766,-11.1400969285548,-33.706563836516));
#25956=CARTESIAN_POINT('Ctrl Pts',(34.1875784009834,-11.1312146907202,-33.7159897117274));
#25957=CARTESIAN_POINT('Ctrl Pts',(34.1827894597102,-11.1219138479108,-33.7258598126315));
#25958=CARTESIAN_POINT('Ctrl Pts',(34.1777533000673,-11.113235294885,-33.7362249700341));
#25959=CARTESIAN_POINT('Ctrl Pts',(34.1724822309008,-11.1050933657994,-33.7470566898643));
#25960=CARTESIAN_POINT('Ctrl Pts',(34.1718566195823,-11.1041270185878,-33.7483422822765));
#25961=CARTESIAN_POINT('Ctrl Pts',(34.1712276759863,-11.1031682588511,-33.7496344946185));
#25962=CARTESIAN_POINT('Ctrl Pts',(34.1705954024983,-11.1022169660873,-33.7509333164964));
#25963=CARTESIAN_POINT('Ctrl Pts',(34.1678668043632,-11.0981116292185,-33.7565384272931));
#25964=CARTESIAN_POINT('Ctrl Pts',(34.1651007375946,-11.0941782436166,-33.7622161899406));
#25965=CARTESIAN_POINT('Ctrl Pts',(34.162294156686,-11.0904041712721,-33.7679726124447));
#25966=CARTESIAN_POINT('Ctrl Pts',(34.1537568943567,-11.0789239229899,-33.785482917901));
#25967=CARTESIAN_POINT('Ctrl Pts',(34.1448975552561,-11.0689908784591,-33.8035911672373));
#25968=CARTESIAN_POINT('Ctrl Pts',(34.1357398214884,-11.0604019317832,-33.8222409108108));
#25969=CARTESIAN_POINT('Ctrl Pts',(34.1265820877206,-11.0518129851072,-33.8408906543843));
#25970=CARTESIAN_POINT('Ctrl Pts',(34.1171258275511,-11.0445686309467,-33.8600822647688));
#25971=CARTESIAN_POINT('Ctrl Pts',(34.1073798559662,-11.0385127393806,-33.8797906568829));
#25972=CARTESIAN_POINT('Ctrl Pts',(34.0969865438925,-11.0320546073838,-33.9008081068036));
#25973=CARTESIAN_POINT('Ctrl Pts',(34.0865219665413,-11.0271158190903,-33.9218908816861));
#25974=CARTESIAN_POINT('Ctrl Pts',(34.075958462414,-11.0235921824178,-33.943096926213));
#25975=CARTESIAN_POINT('Ctrl Pts',(34.0652130000177,-11.0200078504663,-33.9646682486918));
#25976=CARTESIAN_POINT('Ctrl Pts',(34.0543651598294,-11.0178879088427,-33.986367234626));
#25977=CARTESIAN_POINT('Ctrl Pts',(34.0433794528319,-11.0171750715249,-34.008264765842));
#25978=CARTESIAN_POINT('Ctrl Pts',(34.0405982750767,-11.0169946072825,-34.0138084169449));
#25979=CARTESIAN_POINT('Ctrl Pts',(34.037808230387,-11.0169045823054,-34.0193648371644));
#25980=CARTESIAN_POINT('Ctrl Pts',(34.0350086811056,-11.0169045823054,-34.02493526194));
#25981=CARTESIAN_POINT('Origin',(0.0835265683620477,-14.4544045823054,0.0824317919394229));
#25982=CARTESIAN_POINT('Origin',(9.92432302202933,-14.4544045823054,19.2683675629017));
#25983=CARTESIAN_POINT('Origin',(-4.99063502851588,-14.4544045823054,15.4703110263562));
#25984=CARTESIAN_POINT('Origin',(18.7518431265311,-14.4544045823054,23.2994061884498));
#25985=CARTESIAN_POINT('Ctrl Pts',(47.3447344898066,-14.6836564585996,32.1335442243844));
#25986=CARTESIAN_POINT('Ctrl Pts',(47.2330781733367,-14.7195047625521,32.3620574462612));
#25987=CARTESIAN_POINT('Ctrl Pts',(47.0639886181844,-14.9046273277204,32.306300072934));
#25988=CARTESIAN_POINT('Ctrl Pts',(46.88743888664,-14.2208393515121,31.9832691884364));
#25989=CARTESIAN_POINT('Ctrl Pts',(46.7760368073049,-14.2572370951372,32.2113478057363));
#25990=CARTESIAN_POINT('Ctrl Pts',(46.6069803497971,-14.44181022121,32.1556013463856));
#25991=CARTESIAN_POINT('Ctrl Pts',(46.4299123063411,-13.7582547217156,31.8329303749028));
#25992=CARTESIAN_POINT('Ctrl Pts',(46.3184777038413,-13.7949155819421,32.060467441034));
#25993=CARTESIAN_POINT('Ctrl Pts',(46.1497497223463,-13.9792255914392,32.0048292968144));
#25994=CARTESIAN_POINT('Ctrl Pts',(45.9721485234461,-13.2959337131846,31.6825266249535));
#25995=CARTESIAN_POINT('Ctrl Pts',(45.8603516012668,-13.3325299785125,31.9094001080471));
#25996=CARTESIAN_POINT('Ctrl Pts',(45.6922912884794,-13.5169045823054,31.8539821279529));
#25997=CARTESIAN_POINT('Origin',(45.7901549780056,-13.5169045823054,31.5572011510148));
#25998=CARTESIAN_POINT('Origin',(0.0835265683620477,-13.5169045823054,0.0824317919394229));
#25999=CARTESIAN_POINT('Origin',(45.7901549780056,-13.5169045823054,31.5572011510148));
#26000=CARTESIAN_POINT('Origin',(-4.3055892018327,-12.8919045823054,13.3928441877896));
#26001=CARTESIAN_POINT('Origin',(40.0376426042469,-12.8919045823054,28.0150491378139));
#26002=CARTESIAN_POINT('Origin',(0.0835265683620477,-5.8874628440639,0.0824317919394229));
#26003=CARTESIAN_POINT('Ctrl Pts',(-48.3539734316379,-14.9741386829693,
-30.3741755844114));
#26004=CARTESIAN_POINT('Ctrl Pts',(-48.3539734316379,-14.8357920829905,
-30.4481591048434));
#26005=CARTESIAN_POINT('Ctrl Pts',(-48.2281585089893,-14.7531448966919,
-30.4923562863941));
#26006=CARTESIAN_POINT('Ctrl Pts',(-48.3539734316379,-13.8793029116966,
-28.3268709202925));
#26007=CARTESIAN_POINT('Ctrl Pts',(-48.353973431638,-13.7458678866791,-28.4041169753078));
#26008=CARTESIAN_POINT('Ctrl Pts',(-48.2317488064611,-13.6583075326763,
-28.439377201631));
#26009=CARTESIAN_POINT('Ctrl Pts',(-48.3539734316379,-12.8434482903031,
-26.2438196848709));
#26010=CARTESIAN_POINT('Ctrl Pts',(-48.3539734316379,-12.7103751542451,
-26.3167263455105));
#26011=CARTESIAN_POINT('Ctrl Pts',(-48.2353559924772,-12.6224528665257,
-26.3500637611613));
#26012=CARTESIAN_POINT('Ctrl Pts',(-48.3539734316379,-11.4077451872907,
-23.0475925985065));
#26013=CARTESIAN_POINT('Ctrl Pts',(-48.353973431638,-11.2735898053161,-23.1079173838282));
#26014=CARTESIAN_POINT('Ctrl Pts',(-48.2406193805204,-11.1867499400323,
-23.143370974004));
#26015=CARTESIAN_POINT('Ctrl Pts',(-48.3539734316379,-10.9489604127269,
-21.9701832380143));
#26016=CARTESIAN_POINT('Ctrl Pts',(-48.353973431638,-10.8151504288127,-22.0280335561356));
#26017=CARTESIAN_POINT('Ctrl Pts',(-48.2423483273574,-10.7279650272951,
-22.0622935359395));
#26018=CARTESIAN_POINT('Ctrl Pts',(-48.3539734316379,-10.0773547210536,
-19.7874828213299));
#26019=CARTESIAN_POINT('Ctrl Pts',(-48.353973431638,-9.94441815656983,-19.8402912091848));
#26020=CARTESIAN_POINT('Ctrl Pts',(-48.2457130710704,-9.85635900888278,
-19.871869217566));
#26021=CARTESIAN_POINT('Ctrl Pts',(-48.3539734316379,-9.66512413195427,
-18.6831101240159));
#26022=CARTESIAN_POINT('Ctrl Pts',(-48.353973431638,-9.53246556459247,-18.7331822824075));
#26023=CARTESIAN_POINT('Ctrl Pts',(-48.2473467934865,-9.44412830209105,
-18.7634428488815));
#26024=CARTESIAN_POINT('Ctrl Pts',(-48.3539734316379,-7.7573342368428,-13.1446350442278));
#26025=CARTESIAN_POINT('Ctrl Pts',(-48.353973431638,-7.63508483858545,-13.2059559526897));
#26026=CARTESIAN_POINT('Ctrl Pts',(-48.2550691977422,-7.53633525781305,
-13.2039172467247));
#26027=CARTESIAN_POINT('Ctrl Pts',(-48.3539734316379,-6.70462823796961,
-8.61608142151409));
#26028=CARTESIAN_POINT('Ctrl Pts',(-48.353973431638,-6.57519149764306,-8.64715660898112));
#26029=CARTESIAN_POINT('Ctrl Pts',(-48.259869139976,-6.48363668557058,-8.65580178786413));
#26030=CARTESIAN_POINT('Ctrl Pts',(-48.3539734316379,-6.31501530004509,
-3.95028918791133));
#26031=CARTESIAN_POINT('Ctrl Pts',(-48.353973431638,-6.18536424665269,-3.96111558677735));
#26032=CARTESIAN_POINT('Ctrl Pts',(-48.2616461026061,-6.09401826675112,
-3.9687433536743));
#26033=CARTESIAN_POINT('Ctrl Pts',(-48.2284487824325,-14.6753754514262,
-30.3462212704574));
#26034=CARTESIAN_POINT('Ctrl Pts',(-48.2380517942861,-14.6690745001747,
-30.3191514097119));
#26035=CARTESIAN_POINT('Ctrl Pts',(-48.2467246024825,-14.6627081744215,
-30.2917846168048));
#26036=CARTESIAN_POINT('Ctrl Pts',(-48.2546340278731,-14.656301600065,-30.26422929553));
#26037=CARTESIAN_POINT('Ctrl Pts',(-48.2630249404881,-14.6495050247221,
-30.2349965407501));
#26038=CARTESIAN_POINT('Ctrl Pts',(-48.2705565129546,-14.6426630446869,
-30.2055511526331));
#26039=CARTESIAN_POINT('Ctrl Pts',(-48.2773911339934,-14.6357952456547,
-30.1759776611132));
#26040=CARTESIAN_POINT('Ctrl Pts',(-48.2850046107278,-14.6281448100487,
-30.1430340511656));
#26041=CARTESIAN_POINT('Ctrl Pts',(-48.2917532457326,-14.6204622387226,
-30.1099310736677));
#26042=CARTESIAN_POINT('Ctrl Pts',(-48.2978182296841,-14.6127635931359,
-30.0767379272495));
#26043=CARTESIAN_POINT('Ctrl Pts',(-48.3045464712037,-14.6042230351895,
-30.0399148280156));
#26044=CARTESIAN_POINT('Ctrl Pts',(-48.3104330917546,-14.5956624333502,
-30.0029796599166));
#26045=CARTESIAN_POINT('Ctrl Pts',(-48.3156769463159,-14.5870937621613,
-29.9659834425651));
#26046=CARTESIAN_POINT('Ctrl Pts',(-48.3196586203822,-14.5805875451302,
-29.9378921068009));
#26047=CARTESIAN_POINT('Ctrl Pts',(-48.3232685595429,-14.5740764123797,
-29.9097644296832));
#26048=CARTESIAN_POINT('Ctrl Pts',(-48.3265802528816,-14.567564046071,-29.8816156801631));
#26049=CARTESIAN_POINT('Ctrl Pts',(-48.3269187812443,-14.5668983380848,
-29.8787382548971));
#26050=CARTESIAN_POINT('Ctrl Pts',(-48.3272539901496,-14.5662323997339,
-29.8758596817254));
#26051=CARTESIAN_POINT('Ctrl Pts',(-48.3275859006452,-14.5655662082161,
-29.8729798623161));
#26052=CARTESIAN_POINT('Ctrl Pts',(-48.3385590056696,-14.5435416275269,
-29.7777717828841));
#26053=CARTESIAN_POINT('Ctrl Pts',(-48.3458113929029,-14.521489722448,-29.6822597427751));
#26054=CARTESIAN_POINT('Ctrl Pts',(-48.349892235323,-14.4994225808413,-29.5864906154957));
#26055=CARTESIAN_POINT('Ctrl Pts',(-48.3526660001049,-14.4844234571493,
-29.5213959597605));
#26056=CARTESIAN_POINT('Ctrl Pts',(-48.3539733066297,-14.4694172066211,
-29.4561822481182));
#26057=CARTESIAN_POINT('Ctrl Pts',(-48.353973431629,-14.454406734056,-29.3908610634297));
#26058=CARTESIAN_POINT('Ctrl Pts',(-48.2281934536869,-14.7531486984911,
30.6571717707886));
#26059=CARTESIAN_POINT('Ctrl Pts',(-48.3539734316379,-14.8357969973015,
30.6129740313388));
#26060=CARTESIAN_POINT('Ctrl Pts',(-48.3539734316379,-14.9741195676119,
30.5390034232244));
#26061=CARTESIAN_POINT('Ctrl Pts',(-48.2317820061024,-13.6585793127022,
28.6046931834481));
#26062=CARTESIAN_POINT('Ctrl Pts',(-48.353973431646,-13.7461362596114,28.5694255116643));
#26063=CARTESIAN_POINT('Ctrl Pts',(-48.3539734316379,-13.8795503180259,
28.4921954301588));
#26064=CARTESIAN_POINT('Ctrl Pts',(-48.2353869404035,-12.6231097579324,
26.5161580434808));
#26065=CARTESIAN_POINT('Ctrl Pts',(-48.353973431638,-12.711026527187,26.4828083346013));
#26066=CARTESIAN_POINT('Ctrl Pts',(-48.3539734316379,-12.844080626948,26.4099196549775));
#26067=CARTESIAN_POINT('Ctrl Pts',(-48.2406462654066,-11.1881005852611,
23.3112728899427));
#26068=CARTESIAN_POINT('Ctrl Pts',(-48.353973431638,-11.2749369501005,23.2758135504267));
#26069=CARTESIAN_POINT('Ctrl Pts',(-48.3539734316379,-11.4090714544345,
23.2154943062685));
#26070=CARTESIAN_POINT('Ctrl Pts',(-48.24237374671,-10.7295656511252,22.2309062509719));
#26071=CARTESIAN_POINT('Ctrl Pts',(-48.353973431638,-10.816746996712,22.1966391076998));
#26072=CARTESIAN_POINT('Ctrl Pts',(-48.3539734316379,-10.9505365201866,
22.1387927374662));
#26073=CARTESIAN_POINT('Ctrl Pts',(-48.2457354335294,-9.85847188921457,
20.0421726047875));
#26074=CARTESIAN_POINT('Ctrl Pts',(-48.3539734316379,-9.94652588376064,
20.0105850435767));
#26075=CARTESIAN_POINT('Ctrl Pts',(-48.3539734316379,-10.0794427583948,
19.9577755041285));
#26076=CARTESIAN_POINT('Ctrl Pts',(-48.2473707001107,-9.44570717935305,
18.932638230004));
#26077=CARTESIAN_POINT('Ctrl Pts',(-48.3539734316379,-9.53404162556803,
18.9023748976264));
#26078=CARTESIAN_POINT('Ctrl Pts',(-48.3539734316379,-9.66667804843004,
18.852297914388));
#26079=CARTESIAN_POINT('Ctrl Pts',(-48.2550987080888,-7.53595817693284,
13.3683509755226));
#26080=CARTESIAN_POINT('Ctrl Pts',(-48.353973431638,-7.63471881015775,13.3704269700606));
#26081=CARTESIAN_POINT('Ctrl Pts',(-48.3539734316379,-7.75692904622887,
13.3090686823533));
#26082=CARTESIAN_POINT('Ctrl Pts',(-48.2598967761517,-6.48350292013321,
8.81865536350909));
#26083=CARTESIAN_POINT('Ctrl Pts',(-48.3539734316379,-6.57505277910396,
8.81000220468341));
#26084=CARTESIAN_POINT('Ctrl Pts',(-48.3539734316379,-6.70446830386371,
8.77894670225279));
#26085=CARTESIAN_POINT('Ctrl Pts',(-48.2616725171888,-6.0940504675403,4.13367737178086));
#26086=CARTESIAN_POINT('Ctrl Pts',(-48.3539734316379,-6.18539206100946,
4.12604983539374));
#26087=CARTESIAN_POINT('Ctrl Pts',(-48.3539734316379,-6.3150213366611,4.11522506237069));
#26088=CARTESIAN_POINT('Ctrl Pts',(-48.3539734316292,-14.4544067125518,
29.5557245537287));
#26089=CARTESIAN_POINT('Ctrl Pts',(-48.3539732674099,-14.474282601141,29.6422186055862));
#26090=CARTESIAN_POINT('Ctrl Pts',(-48.3516784774865,-14.4941426280635,
29.7284873150456));
#26091=CARTESIAN_POINT('Ctrl Pts',(-48.3467303041063,-14.5139794995535,
29.8145018353666));
#26092=CARTESIAN_POINT('Ctrl Pts',(-48.3424398274083,-14.5311797123081,
29.8890835581078));
#26093=CARTESIAN_POINT('Ctrl Pts',(-48.3361540294485,-14.5483624868197,
29.9634740170122));
#26094=CARTESIAN_POINT('Ctrl Pts',(-48.3276091486579,-14.5655203189316,
30.0376437438476));
#26095=CARTESIAN_POINT('Ctrl Pts',(-48.3272263411088,-14.5662889835649,
30.0409665206127));
#26096=CARTESIAN_POINT('Ctrl Pts',(-48.3268391006314,-14.5670573738945,
30.044287911485));
#26097=CARTESIAN_POINT('Ctrl Pts',(-48.3264473967985,-14.5678255143183,
30.0476080213421));
#26098=CARTESIAN_POINT('Ctrl Pts',(-48.3217619067946,-14.5770138703539,
30.0873225715689));
#26099=CARTESIAN_POINT('Ctrl Pts',(-48.316495168063,-14.5862107044412,30.1270431157074));
#26100=CARTESIAN_POINT('Ctrl Pts',(-48.3104154469146,-14.5953989044386,
30.1666965637756));
#26101=CARTESIAN_POINT('Ctrl Pts',(-48.3049006360659,-14.6037333631727,
30.2026655268679));
#26102=CARTESIAN_POINT('Ctrl Pts',(-48.2987173294784,-14.6120609299868,
30.2385801726924));
#26103=CARTESIAN_POINT('Ctrl Pts',(-48.291662149791,-14.6203642532736,30.2743658179158));
#26104=CARTESIAN_POINT('Ctrl Pts',(-48.2850866379861,-14.6281030498333,
30.3077184670388));
#26105=CARTESIAN_POINT('Ctrl Pts',(-48.2777540899714,-14.6358209223575,
30.3409596295151));
#26106=CARTESIAN_POINT('Ctrl Pts',(-48.2694670548976,-14.6434973280408,
30.3740007357241));
#26107=CARTESIAN_POINT('Ctrl Pts',(-48.2618294825168,-14.6505721266279,
30.4044523795226));
#26108=CARTESIAN_POINT('Ctrl Pts',(-48.2533812725397,-14.6576117669145,
30.4347343630163));
#26109=CARTESIAN_POINT('Ctrl Pts',(-48.2439363682233,-14.6645931621416,
30.4647471875625));
#26110=CARTESIAN_POINT('Ctrl Pts',(-48.2390509274011,-14.6682043361774,
30.480271524635));
#26111=CARTESIAN_POINT('Ctrl Pts',(-48.2338982763733,-14.6717998028497,
30.4957233152332));
#26112=CARTESIAN_POINT('Ctrl Pts',(-48.2284487824329,-14.6753754514261,
30.5110848543365));
#26113=CARTESIAN_POINT('Ctrl Pts',(-48.2616069689928,-6.10843371319294,
4.30318191980438));
#26114=CARTESIAN_POINT('Ctrl Pts',(-48.2619184079005,-6.10843410331518,
4.29961926247631));
#26115=CARTESIAN_POINT('Ctrl Pts',(-48.2763274441054,-6.12223873054911,
4.29756562167191));
#26116=CARTESIAN_POINT('Ctrl Pts',(-48.3054382973494,-6.16064820739694,
4.29414588360541));
#26117=CARTESIAN_POINT('Ctrl Pts',(-48.319962915512,-6.1854892637356,4.29278763374148));
#26118=CARTESIAN_POINT('Ctrl Pts',(-48.3299590819564,-6.2094696845087,4.291470939112));
#26119=CARTESIAN_POINT('Origin',(-48.6664734316379,-14.4544045823054,-44.2925682080606));
#26120=CARTESIAN_POINT('Origin',(-48.6664734316379,-14.4544045823054,29.555715283519));
#26121=CARTESIAN_POINT('Origin',(-48.6664734316379,-14.4544045823054,-29.3908516996402));
#26122=CARTESIAN_POINT('Ctrl Pts',(-48.666473431638,-14.7669045823054,-29.3908516996402));
#26123=CARTESIAN_POINT('Ctrl Pts',(-48.353973431638,-14.7669045823054,-29.3908516996402));
#26124=CARTESIAN_POINT('Ctrl Pts',(-48.353973431638,-14.4544045823054,-29.3908516996402));
#26125=CARTESIAN_POINT('Ctrl Pts',(-48.6664734300675,-14.7669045823054,
-29.5764473463203));
#26126=CARTESIAN_POINT('Ctrl Pts',(-48.3898840300057,-14.7669045823054,
-29.5471242124449));
#26127=CARTESIAN_POINT('Ctrl Pts',(-48.353973431638,-14.4924835039823,-29.5565600468581));
#26128=CARTESIAN_POINT('Ctrl Pts',(-48.6496385395544,-14.7669045823054,
-29.760152449079));
#26129=CARTESIAN_POINT('Ctrl Pts',(-48.4083048654681,-14.7669045823054,
-29.7192585224243));
#26130=CARTESIAN_POINT('Ctrl Pts',(-48.345555980154,-14.5302479546778,-29.7203266919373));
#26131=CARTESIAN_POINT('Ctrl Pts',(-48.5737303814916,-14.7669045823054,
-30.1225239035316));
#26132=CARTESIAN_POINT('Ctrl Pts',(-48.3969357334759,-14.7669045823054,
-30.0607578147132));
#26133=CARTESIAN_POINT('Ctrl Pts',(-48.307601912007,-14.6048732634489,-30.0429041209019));
#26134=CARTESIAN_POINT('Ctrl Pts',(-48.5155778976522,-14.7669045823054,
-30.3049694134568));
#26135=CARTESIAN_POINT('Ctrl Pts',(-48.3721493817961,-14.7669045823059,
-30.2369968366664));
#26136=CARTESIAN_POINT('Ctrl Pts',(-48.2786791401611,-14.6424170542665,
-30.2046271131434));
#26137=CARTESIAN_POINT('Ctrl Pts',(-48.415424133227,-14.7669045823054,-30.4639852003989));
#26138=CARTESIAN_POINT('Ctrl Pts',(-48.305896508561,-14.7669045823054,-30.3950006873975));
#26139=CARTESIAN_POINT('Ctrl Pts',(-48.2284487824325,-14.6753754514262,
-30.3462212704574));
#26140=CARTESIAN_POINT('Origin',(-48.415424133227,-14.4544045823054,-30.4639852003989));
#26141=CARTESIAN_POINT('Origin',(-45.6231018412815,-13.5169045823054,-31.3923375671359));
#26142=CARTESIAN_POINT('Origin',(-45.6231018412815,-13.5169045823054,-31.3923375671359));
#26143=CARTESIAN_POINT('Origin',(-45.6231018412815,-13.5169045823054,-31.3923375671359));
#26144=CARTESIAN_POINT('Origin',(-39.8705894675228,-12.8919045823054,-27.8501855539351));
#26145=CARTESIAN_POINT('Origin',(-39.8705894675228,-12.8919045823054,-27.8501855539351));
#26146=CARTESIAN_POINT('Ctrl Pts',(-34.2908051207842,-13.5169045823054,
-34.2861336374548));
#26147=CARTESIAN_POINT('Ctrl Pts',(-34.2908051207842,-13.2044045823054,
-34.2861336374548));
#26148=CARTESIAN_POINT('Ctrl Pts',(-34.1929414312581,-13.2044045823054,
-34.5829146143929));
#26149=CARTESIAN_POINT('Ctrl Pts',(-34.2074765603999,-13.5169045582439,
-34.2586559990757));
#26150=CARTESIAN_POINT('Ctrl Pts',(-34.2390780768993,-13.186119131637,-34.2690766164313));
#26151=CARTESIAN_POINT('Ctrl Pts',(-34.1370790312896,-13.2044045823054,
-34.583214693643));
#26152=CARTESIAN_POINT('Ctrl Pts',(-34.1263179792903,-13.5027466839947,
-34.2318939125496));
#26153=CARTESIAN_POINT('Ctrl Pts',(-34.1959174748504,-13.1578432798924,
-34.2548443842914));
#26154=CARTESIAN_POINT('Ctrl Pts',(-34.0825856046419,-13.1973256316195,
-34.5835570770033));
#26155=CARTESIAN_POINT('Ctrl Pts',(-33.9688208616094,-13.4449866817214,
-34.1799591518213));
#26156=CARTESIAN_POINT('Ctrl Pts',(-34.1280308564926,-13.0892356355759,
-34.2324587347441));
#26157=CARTESIAN_POINT('Ctrl Pts',(-33.9766844888021,-13.1684456335484,
-34.5843089536435));
#26158=CARTESIAN_POINT('Ctrl Pts',(-33.8970079820796,-13.4031153721668,
-34.1562788155047));
#26159=CARTESIAN_POINT('Ctrl Pts',(-34.106817243136,-13.0503322093645,-34.2254635341332));
#26160=CARTESIAN_POINT('Ctrl Pts',(-33.92831997416,-13.147509967376,-34.5846967331698));
#26161=CARTESIAN_POINT('Ctrl Pts',(-33.7690007142555,-13.2902331116007,
-34.1140683489017));
#26162=CARTESIAN_POINT('Ctrl Pts',(-34.0865509444696,-12.9767617731722,
-34.2187807110593));
#26163=CARTESIAN_POINT('Ctrl Pts',(-33.8420172589373,-13.0910688568131,
-34.585441064553));
#26164=CARTESIAN_POINT('Ctrl Pts',(-33.7168717646145,-13.2224528271011,
-34.0968787992358));
#26165=CARTESIAN_POINT('Ctrl Pts',(-34.0899725583413,-12.9460615526393,
-34.2199089901059));
#26166=CARTESIAN_POINT('Ctrl Pts',(-33.8068205483247,-13.0571787063092,
-34.5857736886607));
#26167=CARTESIAN_POINT('Ctrl Pts',(-33.6428336845022,-13.0654169357611,
-34.0724647018095));
#26168=CARTESIAN_POINT('Ctrl Pts',(-34.1033496871212,-12.9052920386068,
-34.2243201056398));
#26169=CARTESIAN_POINT('Ctrl Pts',(-33.7568076539782,-12.9786607574272,
-34.5862594970788));
#26170=CARTESIAN_POINT('Ctrl Pts',(-33.6230658166974,-12.9802875861308,
-34.0659462365851));
#26171=CARTESIAN_POINT('Ctrl Pts',(-34.1117050038364,-12.8977806170664,
-34.2270752758985));
#26172=CARTESIAN_POINT('Ctrl Pts',(-33.7434406365763,-12.9360960854268,
-34.5863970888581));
#26173=CARTESIAN_POINT('Ctrl Pts',(-33.6230658340261,-12.8919045823054,
-34.0659462422992));
#26174=CARTESIAN_POINT('Ctrl Pts',(-34.1117049987155,-12.8919045823054,
-34.2270752742097));
#26175=CARTESIAN_POINT('Ctrl Pts',(-33.7434406426353,-12.8919045823054,
-34.5863970829463));
#26176=CARTESIAN_POINT('Origin',(-33.5252021444999,-12.8919045823054,-34.3627272192373));
#26177=CARTESIAN_POINT('Origin',(0.0835265683620477,-11.3294045823054,0.0824317919394229));
#26178=CARTESIAN_POINT('Origin',(6.83612114566777,-11.3294045823054,-20.3954556167886));
#26179=CARTESIAN_POINT('Origin',(20.56141397709,-11.3294045823054,6.83502636924522));
#26180=CARTESIAN_POINT('Origin',(20.56141397709,-11.3294045823054,6.83502636924522));
#26181=CARTESIAN_POINT('Origin',(10.2095634989472,-14.4544045823054,19.8244816432194));
#26182=CARTESIAN_POINT('Origin',(10.2095634989472,-14.4544045823054,19.8244816432194));
#26183=CARTESIAN_POINT('Origin',(45.7901549780056,-13.5169045823054,31.5572011510148));
#26184=CARTESIAN_POINT('Origin',(45.7901549780056,-13.5169045823054,31.5572011510148));
#26185=CARTESIAN_POINT('Origin',(40.0376426042469,-12.8919045823054,28.0150491378139));
#26186=CARTESIAN_POINT('Origin',(40.0376426042469,-12.8919045823054,28.0150491378139));
#26187=CARTESIAN_POINT('Ctrl Pts',(-48.353987706665,-6.00666333723547,0.0824317919588709));
#26188=CARTESIAN_POINT('Ctrl Pts',(-48.3539878230387,-6.01200137934915,
0.433477096833169));
#26189=CARTESIAN_POINT('Ctrl Pts',(-48.3525306312191,-6.02125184123593,
0.784346425692766));
#26190=CARTESIAN_POINT('Ctrl Pts',(-48.3492030226928,-6.04818290219923,
1.48575918442931));
#26191=CARTESIAN_POINT('Ctrl Pts',(-48.3473326059861,-6.06586350127576,
1.83630261430625));
#26192=CARTESIAN_POINT('Ctrl Pts',(-48.3448536057857,-6.13245845075532,
2.88748313503321));
#26193=CARTESIAN_POINT('Ctrl Pts',(-48.3401597427993,-6.17306838545285,
3.5897554902018));
#26194=CARTESIAN_POINT('Ctrl Pts',(-48.3299590819564,-6.20946968450872,
4.29147093911199));
#26195=CARTESIAN_POINT('Ctrl Pts',(-48.3539875902919,-6.00132529512177,
0.433477096832907));
#26196=CARTESIAN_POINT('Ctrl Pts',(-48.3530459746152,-6.00879525432317,
0.706493516793873));
#26197=CARTESIAN_POINT('Ctrl Pts',(-48.3513305951691,-6.01828947675677,
0.997236185068297));
#26198=CARTESIAN_POINT('Ctrl Pts',(-48.3474462842671,-6.04432658407327,
1.61112122473693));
#26199=CARTESIAN_POINT('Ctrl Pts',(-48.3452802018324,-6.06089216512325,
1.9342619765643));
#26200=CARTESIAN_POINT('Ctrl Pts',(-48.341640774377,-6.12571278894257,2.9477088419804));
#26201=CARTESIAN_POINT('Ctrl Pts',(-48.3361613302943,-6.16367997403222,
3.62572661437067));
#26202=CARTESIAN_POINT('Ctrl Pts',(-48.3249609987342,-6.19747947412216,
4.29212928642674));
#26203=CARTESIAN_POINT('Ctrl Pts',(-48.3525301621497,-5.99973567328063,
0.784574339470114));
#26204=CARTESIAN_POINT('Ctrl Pts',(-48.3509583174057,-6.00835114797897,
0.9975813791029));
#26205=CARTESIAN_POINT('Ctrl Pts',(-48.34894252132,-6.01789996842715,1.24226674486999));
#26206=CARTESIAN_POINT('Ctrl Pts',(-48.344356416097,-6.04289085428958,1.78530549517593));
#26207=CARTESIAN_POINT('Ctrl Pts',(-48.3417903804913,-6.05836696395447,
2.08365645036453));
#26208=CARTESIAN_POINT('Ctrl Pts',(-48.3366078653997,-6.11975101512505,
3.0446847621152));
#26209=CARTESIAN_POINT('Ctrl Pts',(-48.3302694595669,-6.15479195325803,
3.68769530697585));
#26210=CARTESIAN_POINT('Ctrl Pts',(-48.3188308025825,-6.18527410484421,
4.29279802255009));
#26211=CARTESIAN_POINT('Ctrl Pts',(-48.3427993418055,-5.9982057973697,1.48689990262106));
#26212=CARTESIAN_POINT('Ctrl Pts',(-48.3410826227124,-6.0082917350609,1.61268346924727));
#26213=CARTESIAN_POINT('Ctrl Pts',(-48.3390430002227,-6.01814206512131,
1.78661204317002));
#26214=CARTESIAN_POINT('Ctrl Pts',(-48.3339923325764,-6.04173521008623,
2.20924933968616));
#26215=CARTESIAN_POINT('Ctrl Pts',(-48.3309866293343,-6.05552058030403,
2.45795502559173));
#26216=CARTESIAN_POINT('Ctrl Pts',(-48.3235830578663,-6.10935599904105,
3.28398546777139));
#26217=CARTESIAN_POINT('Ctrl Pts',(-48.316046725529,-6.13882811018934,3.83329116275982));
#26218=CARTESIAN_POINT('Ctrl Pts',(-48.3054305681491,-6.16205725113851,
4.29423379157955));
#26219=CARTESIAN_POINT('Ctrl Pts',(-48.3345259496034,-5.9982655432999,1.8381282231348));
#26220=CARTESIAN_POINT('Ctrl Pts',(-48.3332754509115,-6.00864450579851,
1.93670273202018));
#26221=CARTESIAN_POINT('Ctrl Pts',(-48.3315028514988,-6.01872578611233,
2.08593433407471));
#26222=CARTESIAN_POINT('Ctrl Pts',(-48.3266822403813,-6.04195544062561,
2.45901835426532));
#26223=CARTESIAN_POINT('Ctrl Pts',(-48.3236392144634,-6.05514353311748,
2.68286793815945));
#26224=CARTESIAN_POINT('Ctrl Pts',(-48.3155720249932,-6.10489083408607,
3.42631528823035));
#26225=CARTESIAN_POINT('Ctrl Pts',(-48.3077158622186,-6.13175228789483,
3.9169183259386));
#26226=CARTESIAN_POINT('Ctrl Pts',(-48.2981605298675,-6.15104576671075,
4.29500082448565));
#26227=CARTESIAN_POINT('Ctrl Pts',(-48.293629816125,-5.99214762358688,2.89205060501609));
#26228=CARTESIAN_POINT('Ctrl Pts',(-48.2931970947763,-6.0038166575676,2.9533318756659));
#26229=CARTESIAN_POINT('Ctrl Pts',(-48.2925867091264,-6.01569196513301,
3.05034122028972));
#26230=CARTESIAN_POINT('Ctrl Pts',(-48.2905861997381,-6.040339618854,3.28859696686724));
#26231=CARTESIAN_POINT('Ctrl Pts',(-48.2891989250207,-6.05313466117666,
3.4298417492541));
#26232=CARTESIAN_POINT('Ctrl Pts',(-48.2851290640768,-6.09364276617915,
3.87910729199725));
#26233=CARTESIAN_POINT('Ctrl Pts',(-48.2810866692063,-6.11446024451104,
4.15478252188684));
#26234=CARTESIAN_POINT('Ctrl Pts',(-48.2763272274218,-6.12223844465217,
4.29756564712637));
#26235=CARTESIAN_POINT('Ctrl Pts',(-48.2504292399881,-5.99475664078892,
3.59330337787141));
#26236=CARTESIAN_POINT('Ctrl Pts',(-48.2516773068009,-6.00697011627484,
3.63027912062932));
#26237=CARTESIAN_POINT('Ctrl Pts',(-48.253021728415,-6.02014444454773,3.69245653521261));
#26238=CARTESIAN_POINT('Ctrl Pts',(-48.2556497470798,-6.04594588203951,
3.83761867006235));
#26239=CARTESIAN_POINT('Ctrl Pts',(-48.2569333441305,-6.05857299125839,
3.92060339032879));
#26240=CARTESIAN_POINT('Ctrl Pts',(-48.260312597188,-6.09193010339209,4.15637445270144));
#26241=CARTESIAN_POINT('Ctrl Pts',(-48.2619367151003,-6.10813589078396,
4.29597769638096));
#26242=CARTESIAN_POINT('Ctrl Pts',(-48.2619179788887,-6.1084336923001,4.29961932362109));
#26243=CARTESIAN_POINT('Ctrl Pts',(-48.1943732865555,-6.00705144710499,
4.29441317095732));
#26244=CARTESIAN_POINT('Ctrl Pts',(-48.1993391601324,-6.01900581052063,
4.29446585817732));
#26245=CARTESIAN_POINT('Ctrl Pts',(-48.2060243727241,-6.03128117156189,
4.29459893941721));
#26246=CARTESIAN_POINT('Ctrl Pts',(-48.2204933169654,-6.05467770199134,
4.29515956957315));
#26247=CARTESIAN_POINT('Ctrl Pts',(-48.2282770486149,-6.06579887137953,
4.2955871184892));
#26248=CARTESIAN_POINT('Ctrl Pts',(-48.2497657836928,-6.09473681170807,
4.29751198620615));
#26249=CARTESIAN_POINT('Ctrl Pts',(-48.2616083272502,-6.10812801481236,
4.29965152597587));
#26250=CARTESIAN_POINT('Ctrl Pts',(-48.2616069550931,-6.10843371318469,
4.30318207891618));
#26251=CARTESIAN_POINT('Ctrl Pts',(-48.2616069551289,-6.10843370450312,
4.30318197869235));
#26252=CARTESIAN_POINT('Ctrl Pts',(-48.2616070232649,-6.10841554618156,
4.30297243702759));
#26253=CARTESIAN_POINT('Ctrl Pts',(-48.261568504835,-6.10835892241089,4.30281626830296));
#26254=CARTESIAN_POINT('Ctrl Pts',(-48.2615317413218,-6.10830758140196,
4.30270005783412));
#26255=CARTESIAN_POINT('Ctrl Pts',(-48.2614948949699,-6.108256124707,4.30258358550975));
#26256=CARTESIAN_POINT('Ctrl Pts',(-48.2614587515144,-6.10820886405691,
4.30250736538357));
#26257=CARTESIAN_POINT('Ctrl Pts',(-48.2614364198362,-6.10817971723294,
4.3024610753784));
#26258=CARTESIAN_POINT('Ctrl Pts',(-48.261391803134,-6.10812148447717,4.30236859207495));
#26259=CARTESIAN_POINT('Ctrl Pts',(-48.2613611308546,-6.10808254421549,
4.30231835467004));
#26260=CARTESIAN_POINT('Ctrl Pts',(-48.2613314964975,-6.10804496697612,
4.30227052055935));
#26261=CARTESIAN_POINT('Ctrl Pts',(-48.2612722277834,-6.10796981249738,
4.30217485233798));
#26262=CARTESIAN_POINT('Ctrl Pts',(-48.2612207139529,-6.10790555145939,
4.30210514206976));
#26263=CARTESIAN_POINT('Ctrl Pts',(-48.2611666188386,-6.10783843371047,
4.30203697537195));
#26264=CARTESIAN_POINT('Ctrl Pts',(-48.2609812244811,-6.10760840828066,
4.30180335499264));
#26265=CARTESIAN_POINT('Ctrl Pts',(-48.2607712975097,-6.10735331838435,
4.30161270338785));
#26266=CARTESIAN_POINT('Ctrl Pts',(-48.2605614051161,-6.10709948505642,
4.30144691969731));
#26267=CARTESIAN_POINT('Ctrl Pts',(-48.2602786597362,-6.10675754698275,
4.30122359301185));
#26268=CARTESIAN_POINT('Ctrl Pts',(-48.2599937148647,-6.10641533300863,
4.30104387204264));
#26269=CARTESIAN_POINT('Ctrl Pts',(-48.2596984045309,-6.10606098282255,
4.30087738558224));
#26270=CARTESIAN_POINT('Ctrl Pts',(-48.2592951604377,-6.1055771202446,4.30065004954269));
#26271=CARTESIAN_POINT('Ctrl Pts',(-48.2588878641398,-6.10508918081615,
4.30045936658896));
#26272=CARTESIAN_POINT('Ctrl Pts',(-48.2584803602671,-6.10460034109874,
4.30028708750468));
#26273=CARTESIAN_POINT('Ctrl Pts',(-48.2577834928373,-6.10376438222755,
4.29999247513237));
#26274=CARTESIAN_POINT('Ctrl Pts',(-48.2570827132334,-6.10292193531566,
4.2997513336239));
#26275=CARTESIAN_POINT('Ctrl Pts',(-48.2563837106908,-6.10207801393888,
4.29953565913165));
#26276=CARTESIAN_POINT('Ctrl Pts',(-48.2552039588319,-6.10065367317838,
4.29917165132385));
#26277=CARTESIAN_POINT('Ctrl Pts',(-48.254026426545,-6.09922194596883,4.29888122427205));
#26278=CARTESIAN_POINT('Ctrl Pts',(-48.2528540013546,-6.09778441771827,
4.29862403126663));
#26279=CARTESIAN_POINT('Ctrl Pts',(-48.2510293554768,-6.09554719182277,
4.29822376167079));
#26280=CARTESIAN_POINT('Ctrl Pts',(-48.2492165852536,-6.09329562622209,
4.29790736627066));
#26281=CARTESIAN_POINT('Ctrl Pts',(-48.2474182713127,-6.09103086693172,
4.2976305747359));
#26282=CARTESIAN_POINT('Ctrl Pts',(-48.2447139428525,-6.08762509174139,
4.29721433193871));
#26283=CARTESIAN_POINT('Ctrl Pts',(-48.2420414322396,-6.08418870246316,
4.29689093118225));
#26284=CARTESIAN_POINT('Ctrl Pts',(-48.239407025734,-6.08072383167611,4.29661384152446));
#26285=CARTESIAN_POINT('Ctrl Pts',(-48.2380751607036,-6.07897211255965,
4.2964737545543));
#26286=CARTESIAN_POINT('Ctrl Pts',(-48.2367524918963,-6.07721238041329,
4.29634631195034));
#26287=CARTESIAN_POINT('Ctrl Pts',(-48.2354399603075,-6.07544485148905,
4.29622874106152));
#26288=CARTESIAN_POINT('Ctrl Pts',(-48.2312254371352,-6.06976933733557,
4.29585122234916));
#26289=CARTESIAN_POINT('Ctrl Pts',(-48.22711583857,-6.06401604656339,4.29557214159525));
#26290=CARTESIAN_POINT('Ctrl Pts',(-48.2231376376079,-6.05817108586382,
4.29534669590986));
#26291=CARTESIAN_POINT('Ctrl Pts',(-48.2197392166315,-6.05317796529557,
4.29515410650737));
#26292=CARTESIAN_POINT('Ctrl Pts',(-48.2164370013549,-6.04811857023788,
4.29500239895895));
#26293=CARTESIAN_POINT('Ctrl Pts',(-48.2132588448447,-6.04297943677661,
4.29487925449518));
#26294=CARTESIAN_POINT('Ctrl Pts',(-48.2098408541154,-6.03745248727896,
4.29474681714221));
#26295=CARTESIAN_POINT('Ctrl Pts',(-48.206564810075,-6.03183339812509,4.29464768913944));
#26296=CARTESIAN_POINT('Ctrl Pts',(-48.2034906784034,-6.02609676302333,
4.29457335819765));
#26297=CARTESIAN_POINT('Ctrl Pts',(-48.2008503025217,-6.02116955931759,
4.29450951525046));
#26298=CARTESIAN_POINT('Ctrl Pts',(-48.1983577537265,-6.01615482893866,
4.29446412495472));
#26299=CARTESIAN_POINT('Ctrl Pts',(-48.1960855539946,-6.01103540679842,
4.29443373440248));
#26300=CARTESIAN_POINT('Ctrl Pts',(-48.195712281463,-6.01019439813361,4.29442874190195));
#26301=CARTESIAN_POINT('Ctrl Pts',(-48.1953450670276,-6.00935058232647,
4.29442415648971));
#26302=CARTESIAN_POINT('Ctrl Pts',(-48.1949843830272,-6.00850392013414,
4.2944199650574));
#26303=CARTESIAN_POINT('Ctrl Pts',(-48.1947785238618,-6.00802069056991,
4.29441757281168));
#26304=CARTESIAN_POINT('Ctrl Pts',(-48.1945747929681,-6.00753653413945,
4.29441530891201));
#26305=CARTESIAN_POINT('Ctrl Pts',(-48.1943732865555,-6.007051447105,4.29441317095728));
#26306=CARTESIAN_POINT('Ctrl Pts',(-48.352959262434,-14.4313124010519,29.4551542809743));
#26307=CARTESIAN_POINT('Ctrl Pts',(-48.3280930508149,-14.7671408703067,
29.45593300004));
#26308=CARTESIAN_POINT('Ctrl Pts',(-48.6646643620667,-14.7669045053135,
29.4431122185066));
#26309=CARTESIAN_POINT('Ctrl Pts',(-48.3569869626293,-14.4776157931201,
29.656936726707));
#26310=CARTESIAN_POINT('Ctrl Pts',(-48.3813383783207,-14.7670932226576,
29.6397654298998));
#26311=CARTESIAN_POINT('Ctrl Pts',(-48.6727054456496,-14.766904515933,29.668999675558));
#26312=CARTESIAN_POINT('Ctrl Pts',(-48.3491923518221,-14.5232222287049,
29.8548235931214));
#26313=CARTESIAN_POINT('Ctrl Pts',(-48.4096589429883,-14.7670538266339,
29.8485725191841));
#26314=CARTESIAN_POINT('Ctrl Pts',(-48.6570966106634,-14.7669045263941,
29.8909334903031));
#26315=CARTESIAN_POINT('Ctrl Pts',(-48.3036995582031,-14.6124212350927,
30.2403918438327));
#26316=CARTESIAN_POINT('Ctrl Pts',(-48.395816449558,-14.7669897766186,30.2571389072456));
#26317=CARTESIAN_POINT('Ctrl Pts',(-48.5660672929221,-14.7669045468573,
30.3240933952862));
#26318=CARTESIAN_POINT('Ctrl Pts',(-48.2672919864971,-14.6570503433833,
30.4325068115059));
#26319=CARTESIAN_POINT('Ctrl Pts',(-48.3627479488335,-14.7669625172413,
30.4679205353142));
#26320=CARTESIAN_POINT('Ctrl Pts',(-48.492687194552,-14.766904557097,30.5411709062376));
#26321=CARTESIAN_POINT('Ctrl Pts',(-48.1953287895212,-14.694785451968,30.5944226583824));
#26322=CARTESIAN_POINT('Ctrl Pts',(-48.2623775405895,-14.7669413153286,
30.6502218321353));
#26323=CARTESIAN_POINT('Ctrl Pts',(-48.3495845206488,-14.7669045657556,
30.7223070272069));
#26324=CARTESIAN_POINT('Origin',(-48.415424133227,-14.4544045823054,30.6288487842778));
#26325=CARTESIAN_POINT('Origin',(0.0835265683620477,-14.4544045823054,0.0824317919394229));
#26326=CARTESIAN_POINT('Origin',(-47.352376130838,-14.4544045823054,-32.090024523005));
#26327=CARTESIAN_POINT('Ctrl Pts',(-47.1776813530825,-14.6836564585996,
-31.9686806405055));
#26328=CARTESIAN_POINT('Ctrl Pts',(-47.0660250366126,-14.7195047625521,
-32.1971938623823));
#26329=CARTESIAN_POINT('Ctrl Pts',(-46.8969354814603,-14.9046273277204,
-32.1414364890551));
#26330=CARTESIAN_POINT('Ctrl Pts',(-46.7203857499136,-14.2208393515128,
-31.8184056045622));
#26331=CARTESIAN_POINT('Ctrl Pts',(-46.6089836705754,-14.2572370951416,
-32.0464842218602));
#26332=CARTESIAN_POINT('Ctrl Pts',(-46.43992721307,-14.4418102212131,-31.9907377625058));
#26333=CARTESIAN_POINT('Ctrl Pts',(-46.2628591696178,-13.7582547217153,
-31.6680667910224));
#26334=CARTESIAN_POINT('Ctrl Pts',(-46.1514245671171,-13.7949155819443,
-31.895603857149));
#26335=CARTESIAN_POINT('Ctrl Pts',(-45.9826965856166,-13.9792255914456,
-31.8399657129337));
#26336=CARTESIAN_POINT('Ctrl Pts',(-45.805095386722,-13.2959337131846,-31.5176630410747));
#26337=CARTESIAN_POINT('Ctrl Pts',(-45.6932984645427,-13.3325299785125,
-31.7445365241682));
#26338=CARTESIAN_POINT('Ctrl Pts',(-45.5252381517553,-13.5169045823054,
-31.689118544074));
#26339=CARTESIAN_POINT('Ctrl Pts',(-46.45221964492,-14.4544045595336,-31.994791198634));
#26340=CARTESIAN_POINT('Ctrl Pts',(-46.4816446151428,-14.4645898091214,
-32.0044940986644));
#26341=CARTESIAN_POINT('Ctrl Pts',(-46.5113244534831,-14.4747854410082,
-32.0132766896869));
#26342=CARTESIAN_POINT('Ctrl Pts',(-46.5412186258095,-14.4849571274434,
-32.0211162927955));
#26343=CARTESIAN_POINT('Ctrl Pts',(-46.5691103832093,-14.4944474791848,
-32.0284307722073));
#26344=CARTESIAN_POINT('Ctrl Pts',(-46.5971900557739,-14.5039154723653,
-32.0349249639908));
#26345=CARTESIAN_POINT('Ctrl Pts',(-46.6254440592878,-14.513327931455,-32.040538038467));
#26346=CARTESIAN_POINT('Ctrl Pts',(-46.6523812355758,-14.5223017064346,
-32.0458895057948));
#26347=CARTESIAN_POINT('Ctrl Pts',(-46.6794781232448,-14.5312237762472,
-32.0504400452471));
#26348=CARTESIAN_POINT('Ctrl Pts',(-46.7067229940643,-14.5400795913945,
-32.054093202545));
#26349=CARTESIAN_POINT('Ctrl Pts',(-46.7320468275605,-14.548310982534,-32.0574887755232));
#26350=CARTESIAN_POINT('Ctrl Pts',(-46.7574994914588,-14.5564843935861,
-32.0601083525393));
#26351=CARTESIAN_POINT('Ctrl Pts',(-46.7830561411086,-14.5646141114386,
-32.0618415033403));
#26352=CARTESIAN_POINT('Ctrl Pts',(-46.7938944251968,-14.5680618322021,
-32.0625765128586));
#26353=CARTESIAN_POINT('Ctrl Pts',(-46.8047511303372,-14.5715020908807,
-32.0631517327013));
#26354=CARTESIAN_POINT('Ctrl Pts',(-46.8156227743728,-14.5749379971502,
-32.0635573491533));
#26355=CARTESIAN_POINT('Ctrl Pts',(-46.8348797214202,-14.5810240191793,
-32.0642758177227));
#26356=CARTESIAN_POINT('Ctrl Pts',(-46.8541789969005,-14.587111545562,-32.0644726060865));
#26357=CARTESIAN_POINT('Ctrl Pts',(-46.8734909509673,-14.5931215908451,
-32.0640314432956));
#26358=CARTESIAN_POINT('Ctrl Pts',(-46.8920891917075,-14.5989095224366,
-32.0636065845909));
#26359=CARTESIAN_POINT('Ctrl Pts',(-46.9106999302976,-14.6046251025895,
-32.0625893261362));
#26360=CARTESIAN_POINT('Ctrl Pts',(-46.9292727569436,-14.6102297042048,
-32.0608503486169));
#26361=CARTESIAN_POINT('Ctrl Pts',(-46.946858713788,-14.6155365045112,-32.0592037719169));
#26362=CARTESIAN_POINT('Ctrl Pts',(-46.9644111583127,-14.6207436431621,
-32.0569091901701));
#26363=CARTESIAN_POINT('Ctrl Pts',(-46.9818569474271,-14.6258519573889,
-32.0538455697298));
#26364=CARTESIAN_POINT('Ctrl Pts',(-46.9884617944842,-14.62778592747,-32.0526857056321));
#26365=CARTESIAN_POINT('Ctrl Pts',(-46.9950509954036,-14.6297061021637,
-32.051415567437));
#26366=CARTESIAN_POINT('Ctrl Pts',(-47.0016191535238,-14.6316139267952,
-32.0500286163118));
#26367=CARTESIAN_POINT('Ctrl Pts',(-47.0143605766674,-14.6353148731592,
-32.0473381008213));
#26368=CARTESIAN_POINT('Ctrl Pts',(-47.027091438687,-14.6390800656574,-32.0442661993923));
#26369=CARTESIAN_POINT('Ctrl Pts',(-47.0397058401586,-14.6427512671777,
-32.0406480116584));
#26370=CARTESIAN_POINT('Ctrl Pts',(-47.0517158141394,-14.6462465606196,
-32.0372031918119));
#26371=CARTESIAN_POINT('Ctrl Pts',(-47.0636206116162,-14.6496565428155,
-32.0332623412524));
#26372=CARTESIAN_POINT('Ctrl Pts',(-47.075298133029,-14.6528783603918,-32.0286727207447));
#26373=CARTESIAN_POINT('Ctrl Pts',(-47.0864623275873,-14.6559585515542,
-32.0242848532781));
#26374=CARTESIAN_POINT('Ctrl Pts',(-47.0974190452162,-14.6588667966838,
-32.0193031007959));
#26375=CARTESIAN_POINT('Ctrl Pts',(-47.10802817365,-14.6615453756124,-32.0135965587108));
#26376=CARTESIAN_POINT('Ctrl Pts',(-47.118301340523,-14.6641391314037,-32.0080707269261));
#26377=CARTESIAN_POINT('Ctrl Pts',(-47.1282486966118,-14.6665177507384,
-32.0018642831368));
#26378=CARTESIAN_POINT('Ctrl Pts',(-47.1377081632209,-14.6686579758303,
-31.9948745418285));
#26379=CARTESIAN_POINT('Ctrl Pts',(-47.1467984820774,-14.6707146804327,
-31.9881575693139));
#26380=CARTESIAN_POINT('Ctrl Pts',(-47.155438026338,-14.6725517512547,-31.9807163227433));
#26381=CARTESIAN_POINT('Ctrl Pts',(-47.1634510955046,-14.6741705573044,
-31.9724887075062));
#26382=CARTESIAN_POINT('Ctrl Pts',(-47.1655096976883,-14.6745864376119,
-31.9703749872398));
#26383=CARTESIAN_POINT('Ctrl Pts',(-47.1675267947758,-14.6749880046777,
-31.9682095601077));
#26384=CARTESIAN_POINT('Ctrl Pts',(-47.1694990908454,-14.6753754514118,
-31.9659918126594));
#26385=CARTESIAN_POINT('Origin',(4.96196078618764,-13.5169045823054,-14.7118854886012));
#26386=CARTESIAN_POINT('Origin',(-38.9085015017574,-13.5169045823054,-29.1781944313494));
#26387=CARTESIAN_POINT('Origin',(0.0835265683620477,-12.8919045823054,0.0824317919394229));
#26388=CARTESIAN_POINT('Ctrl Pts',(-38.5307586915594,-12.8919045823054,
-29.1601464137424));
#26389=CARTESIAN_POINT('Ctrl Pts',(-38.5307586915594,-12.9139187960387,
-29.1601464137424));
#26390=CARTESIAN_POINT('Ctrl Pts',(-38.5337445953841,-12.9356278245207,
-29.1602796388799));
#26391=CARTESIAN_POINT('Ctrl Pts',(-38.5392655962948,-12.9566097073211,
-29.1605287235832));
#26392=CARTESIAN_POINT('Ctrl Pts',(-38.5446601059366,-12.9771108756598,
-29.160772101524));
#26393=CARTESIAN_POINT('Ctrl Pts',(-38.5524746087403,-12.9969176625741,
-29.1611260778435));
#26394=CARTESIAN_POINT('Ctrl Pts',(-38.5623024668082,-13.0156824718616,
-29.1615748389679));
#26395=CARTESIAN_POINT('Ctrl Pts',(-38.5724342229867,-13.0350275286508,
-29.1620374767332));
#26396=CARTESIAN_POINT('Ctrl Pts',(-38.5847053607061,-13.0532645768204,
-29.1626008360293));
#26397=CARTESIAN_POINT('Ctrl Pts',(-38.5986906617097,-13.0700686738439,
-29.1632482299304));
#26398=CARTESIAN_POINT('Ctrl Pts',(-38.6117491326753,-13.0857591343516,
-29.1638527199202));
#26399=CARTESIAN_POINT('Ctrl Pts',(-38.6263021044288,-13.1002006435705,
-29.1645304749228));
#26400=CARTESIAN_POINT('Ctrl Pts',(-38.6420231546125,-13.1131767225593,
-29.1652685557058));
#26401=CARTESIAN_POINT('Ctrl Pts',(-38.6431389622425,-13.1140977047949,
-29.1653209412755));
#26402=CARTESIAN_POINT('Ctrl Pts',(-38.6442606627878,-13.1150113249631,
-29.1653736310233));
#26403=CARTESIAN_POINT('Ctrl Pts',(-38.6453881435972,-13.1159175149051,
-29.1654266204564));
#26404=CARTESIAN_POINT('Ctrl Pts',(-38.6482835083063,-13.1182446058459,
-29.1655626970383));
#26405=CARTESIAN_POINT('Ctrl Pts',(-38.6512164926939,-13.1205242789863,
-29.1657007960921));
#26406=CARTESIAN_POINT('Ctrl Pts',(-38.6541844981536,-13.1227565895721,
-29.1658408010566));
#26407=CARTESIAN_POINT('Ctrl Pts',(-38.6686039641446,-13.1336018279015,
-29.1665209874148));
#26408=CARTESIAN_POINT('Ctrl Pts',(-38.6838415011964,-13.143325954299,-29.167242672684));
#26409=CARTESIAN_POINT('Ctrl Pts',(-38.6996821390438,-13.1519718238994,
-29.1679966343372));
#26410=CARTESIAN_POINT('Ctrl Pts',(-38.7169622638872,-13.161403369997,-29.1688191107818));
#26411=CARTESIAN_POINT('Ctrl Pts',(-38.7349606742429,-13.1695524259116,
-29.1696800142245));
#26412=CARTESIAN_POINT('Ctrl Pts',(-38.7534545213138,-13.1764446443681,
-29.1705703361828));
#26413=CARTESIAN_POINT('Ctrl Pts',(-38.7727096512048,-13.1836205748875,
-29.1714973074553));
#26414=CARTESIAN_POINT('Ctrl Pts',(-38.7925031927513,-13.1894346380336,
-29.1724562261581));
#26415=CARTESIAN_POINT('Ctrl Pts',(-38.812625947123,-13.1938753423331,-29.1734393751561));
#26416=CARTESIAN_POINT('Ctrl Pts',(-38.8328614137049,-13.1983409200464,
-29.1744280309994));
#26417=CARTESIAN_POINT('Ctrl Pts',(-38.8534314395746,-13.2014181302604,
-29.1754412664497));
#26418=CARTESIAN_POINT('Ctrl Pts',(-38.8741419834054,-13.2030479859155,
-29.1764726165817));
#26419=CARTESIAN_POINT('Ctrl Pts',(-38.8855632109547,-13.2039468011499,
-29.1770413744393));
#26420=CARTESIAN_POINT('Ctrl Pts',(-38.897027358863,-13.2044045823054,-29.177615659075));
#26421=CARTESIAN_POINT('Ctrl Pts',(-38.9085015017574,-13.2044045823054,
-29.1781944313494));
#26422=CARTESIAN_POINT('Origin',(-33.5252021444999,-14.7669045823054,-34.3627272192373));
#26423=CARTESIAN_POINT('Origin',(-33.5252021444999,-11.3294045823054,-34.3627272192373));
#26424=CARTESIAN_POINT('Origin',(6.83612114566777,-11.3294045823054,-20.3954556167886));
#26425=CARTESIAN_POINT('Ctrl Pts',(-34.0238404855175,-11.0169045823054,
-33.869050320804));
#26426=CARTESIAN_POINT('Ctrl Pts',(-34.001815058166,-11.0169045823054,-33.8801197224743));
#26427=CARTESIAN_POINT('Ctrl Pts',(-33.9800079311155,-11.0183080822726,
-33.8910410032133));
#26428=CARTESIAN_POINT('Ctrl Pts',(-33.9583457631457,-11.0211596046316,
-33.9018512749977));
#26429=CARTESIAN_POINT('Ctrl Pts',(-33.9370471546751,-11.023963269452,-33.912480116327));
#26430=CARTESIAN_POINT('Ctrl Pts',(-33.9158885755623,-11.0281667153259,
-33.9230016547809));
#26431=CARTESIAN_POINT('Ctrl Pts',(-33.8948092427032,-11.0338614984686,
-33.9334452009051));
#26432=CARTESIAN_POINT('Ctrl Pts',(-33.8894330516898,-11.0353139278296,
-33.9361087813512));
#26433=CARTESIAN_POINT('Ctrl Pts',(-33.884062065986,-11.0368636220457,-33.9387672573208));
#26434=CARTESIAN_POINT('Ctrl Pts',(-33.878695385463,-11.0385126341271,-33.9414210499132));
#26435=CARTESIAN_POINT('Ctrl Pts',(-33.8589867794304,-11.0445684687008,
-33.9511668420231));
#26436=CARTESIAN_POINT('Ctrl Pts',(-33.8397948590732,-11.0518127318511,
-33.9606228528326));
#26437=CARTESIAN_POINT('Ctrl Pts',(-33.8211446482646,-11.0604015318982,
-33.9697802594569));
#26438=CARTESIAN_POINT('Ctrl Pts',(-33.802494437456,-11.0689903319452,-33.9789376660811));
#26439=CARTESIAN_POINT('Ctrl Pts',(-33.7843855638675,-11.0789231726624,
-33.9877965998101));
#26440=CARTESIAN_POINT('Ctrl Pts',(-33.7668743980404,-11.0904031558603,
-33.9963333935331));
#26441=CARTESIAN_POINT('Ctrl Pts',(-33.7611096994568,-11.0941823812718,
-33.9991437171386));
#26442=CARTESIAN_POINT('Ctrl Pts',(-33.755434798592,-11.0981143207712,-34.0019084815749));
#26443=CARTESIAN_POINT('Ctrl Pts',(-33.7498350694776,-11.1022159367836,
-34.0046347500796));
#26444=CARTESIAN_POINT('Ctrl Pts',(-33.7402458756978,-11.1092397034604,
-34.0093033182287));
#26445=CARTESIAN_POINT('Ctrl Pts',(-33.7310218705821,-11.116663053783,-34.0137885684103));
#26446=CARTESIAN_POINT('Ctrl Pts',(-33.722142970915,-11.1245727500517,-34.0181002904555));
#26447=CARTESIAN_POINT('Ctrl Pts',(-33.7187799860189,-11.1275686380651,
-34.0197334045414));
#26448=CARTESIAN_POINT('Ctrl Pts',(-33.7154669091464,-11.1306345602644,
-34.0213414284975));
#26449=CARTESIAN_POINT('Ctrl Pts',(-33.712204213352,-11.133776202165,-34.0229241322475));
#26450=CARTESIAN_POINT('Ctrl Pts',(-33.7037506457484,-11.1419161219939,
-34.0270248802151));
#26451=CARTESIAN_POINT('Ctrl Pts',(-33.6956687991695,-11.1505315993466,
-34.0309393829992));
#26452=CARTESIAN_POINT('Ctrl Pts',(-33.6880349165851,-11.1596598005335,
-34.0346338552862));
#26453=CARTESIAN_POINT('Ctrl Pts',(-33.6804010340008,-11.1687880017203,
-34.0383283275731));
#26454=CARTESIAN_POINT('Ctrl Pts',(-33.6732197547124,-11.1784304387767,
-34.0418051487081));
#26455=CARTESIAN_POINT('Ctrl Pts',(-33.6665631119894,-11.18862206557,-34.0450152174752));
#26456=CARTESIAN_POINT('Ctrl Pts',(-33.6633982723472,-11.19346758092,-34.0465414151864));
#26457=CARTESIAN_POINT('Ctrl Pts',(-33.6603504947342,-11.1984446423577,
-34.0480104432143));
#26458=CARTESIAN_POINT('Ctrl Pts',(-33.6574354435571,-11.2035509891889,
-34.049414947688));
#26459=CARTESIAN_POINT('Ctrl Pts',(-33.6506402480387,-11.2154542536581,
-34.0526889493864));
#26460=CARTESIAN_POINT('Ctrl Pts',(-33.6446840759846,-11.2278803704208,
-34.0555560984262));
#26461=CARTESIAN_POINT('Ctrl Pts',(-33.6397392256017,-11.240725680505,-34.0579348223755));
#26462=CARTESIAN_POINT('Ctrl Pts',(-33.634908566084,-11.2532743553102,-34.0602586147242));
#26463=CARTESIAN_POINT('Ctrl Pts',(-33.6310434307528,-11.2662226779423,
-34.0621161155791));
#26464=CARTESIAN_POINT('Ctrl Pts',(-33.6282635085628,-11.2794553416036,
-34.0634513323074));
#26465=CARTESIAN_POINT('Ctrl Pts',(-33.6255593642006,-11.2923272964251,
-34.0647501523971));
#26466=CARTESIAN_POINT('Ctrl Pts',(-33.6238822840565,-11.3054678991102,
-34.0655546880424));
#26467=CARTESIAN_POINT('Ctrl Pts',(-33.6232990879972,-11.3187590936903,
-34.0658343883027));
#26468=CARTESIAN_POINT('Ctrl Pts',(-33.6231438180531,-11.3222977373521,
-34.0659088556161));
#26469=CARTESIAN_POINT('Ctrl Pts',(-33.6230658340261,-11.3258470068808,
-34.0659462422992));
#26470=CARTESIAN_POINT('Ctrl Pts',(-33.6230658340261,-11.3294045823054,
-34.0659462422992));
#26471=CARTESIAN_POINT('Origin',(0.0835265683620477,-11.3294045823054,0.0824317919394229));
#26472=CARTESIAN_POINT('Origin',(9.92432302202933,-11.3294045823054,19.2683675629017));
#26473=CARTESIAN_POINT('Origin',(10.2095634989472,-11.0169045823054,19.8244816432194));
#26474=CARTESIAN_POINT('Origin',(10.2095634989472,-11.3294045823054,19.8244816432194));
#26475=CARTESIAN_POINT('Origin',(-4.79490764946355,-13.5169045823054,14.87674907248));
#26476=CARTESIAN_POINT('Origin',(39.0755546384815,-13.5169045823054,29.3430580152282));
#26477=CARTESIAN_POINT('Origin',(0.0835265683620477,-12.8919045823054,0.0824317919394229));
#26478=CARTESIAN_POINT('Ctrl Pts',(38.6978118282835,-12.8919045823054,29.3250099976212));
#26479=CARTESIAN_POINT('Ctrl Pts',(38.6978118282835,-12.9139187960388,29.3250099976212));
#26480=CARTESIAN_POINT('Ctrl Pts',(38.7007977321083,-12.9356278245209,29.3251432227588));
#26481=CARTESIAN_POINT('Ctrl Pts',(38.7063187330191,-12.9566097073213,29.325392307462));
#26482=CARTESIAN_POINT('Ctrl Pts',(38.711713242661,-12.9771108756606,29.3256356854028));
#26483=CARTESIAN_POINT('Ctrl Pts',(38.7195277454651,-12.9969176625753,29.3259896617223));
#26484=CARTESIAN_POINT('Ctrl Pts',(38.7293556035333,-13.0156824718633,29.3264384228467));
#26485=CARTESIAN_POINT('Ctrl Pts',(38.7394873597118,-13.0350275286521,29.326901060612));
#26486=CARTESIAN_POINT('Ctrl Pts',(38.7517584974311,-13.0532645768214,29.3274644199081));
#26487=CARTESIAN_POINT('Ctrl Pts',(38.7657437984346,-13.0700686738447,29.3281118138092));
#26488=CARTESIAN_POINT('Ctrl Pts',(38.7788022694006,-13.0857591343528,29.328716303799));
#26489=CARTESIAN_POINT('Ctrl Pts',(38.7933552411545,-13.100200643572,29.3293940588016));
#26490=CARTESIAN_POINT('Ctrl Pts',(38.8090762913388,-13.1131767225611,29.3301321395847));
#26491=CARTESIAN_POINT('Ctrl Pts',(38.8101920989681,-13.114097704796,29.3301845251543));
#26492=CARTESIAN_POINT('Ctrl Pts',(38.8113137995126,-13.1150113249637,29.3302372149021));
#26493=CARTESIAN_POINT('Ctrl Pts',(38.8124412803214,-13.115917514905,29.3302902043352));
#26494=CARTESIAN_POINT('Ctrl Pts',(38.8153366450305,-13.1182446058459,29.3304262809171));
#26495=CARTESIAN_POINT('Ctrl Pts',(38.818269629418,-13.1205242789863,29.3305643799709));
#26496=CARTESIAN_POINT('Ctrl Pts',(38.8212376348777,-13.1227565895721,29.3307043849354));
#26497=CARTESIAN_POINT('Ctrl Pts',(38.8356571008678,-13.1336018279008,29.3313845712936));
#26498=CARTESIAN_POINT('Ctrl Pts',(38.8508946379186,-13.1433259542978,29.3321062565627));
#26499=CARTESIAN_POINT('Ctrl Pts',(38.8667352757648,-13.1519718238976,29.3328602182159));
#26500=CARTESIAN_POINT('Ctrl Pts',(38.8840154006071,-13.1614033699948,29.3336826946604));
#26501=CARTESIAN_POINT('Ctrl Pts',(38.9020138109617,-13.1695524259092,29.3345435981031));
#26502=CARTESIAN_POINT('Ctrl Pts',(38.9205076580314,-13.1764446443656,29.3354339200614));
#26503=CARTESIAN_POINT('Ctrl Pts',(38.9397627879212,-13.1836205748849,29.3363608913338));
#26504=CARTESIAN_POINT('Ctrl Pts',(38.9595563294665,-13.1894346380311,29.3373198100366));
#26505=CARTESIAN_POINT('Ctrl Pts',(38.9796790838369,-13.1938753423308,29.3383029590345));
#26506=CARTESIAN_POINT('Ctrl Pts',(38.9999145504174,-13.1983409200443,29.3392916148777));
#26507=CARTESIAN_POINT('Ctrl Pts',(39.0204845762857,-13.2014181302587,29.3403048503279));
#26508=CARTESIAN_POINT('Ctrl Pts',(39.0411951201151,-13.2030479859143,29.3413362004598));
#26509=CARTESIAN_POINT('Ctrl Pts',(39.0526163476692,-13.2039468011495,29.3419049583177));
#26510=CARTESIAN_POINT('Ctrl Pts',(39.0640804955822,-13.2044045823054,29.3424792429536));
#26511=CARTESIAN_POINT('Ctrl Pts',(39.0755546384815,-13.2044045823054,29.3430580152282));
#26512=CARTESIAN_POINT('Origin',(0.0835265683620477,-5.88746284406389,0.0824317919394229));
#26513=CARTESIAN_POINT('Origin',(-36.4579813137992,-5.88746284406388,32.3513131127716));
#26514=CARTESIAN_POINT('Ctrl Pts',(-38.3808256972991,-13.5144022830795,
39.8924656416407));
#26515=CARTESIAN_POINT('Ctrl Pts',(-38.4711302762978,-13.1933434688295,
40.1663228945616));
#26516=CARTESIAN_POINT('Ctrl Pts',(-38.8323465692944,-13.2935409679816,
39.9525013588595));
#26517=CARTESIAN_POINT('Ctrl Pts',(-37.4650940302067,-10.8876753972538,
37.115421979291));
#26518=CARTESIAN_POINT('Ctrl Pts',(-37.5465445455966,-10.5315615515785,
37.3624284395829));
#26519=CARTESIAN_POINT('Ctrl Pts',(-37.9202835812346,-10.666849201302,37.1719078497633));
#26520=CARTESIAN_POINT('Ctrl Pts',(-36.5421507433461,-8.28316552043086,
34.3165083918393));
#26521=CARTESIAN_POINT('Ctrl Pts',(-36.6205153658898,-7.90880842130267,
34.5541565874725));
#26522=CARTESIAN_POINT('Ctrl Pts',(-37.0014278556075,-8.0623563845108,34.3687899544871));
#26523=CARTESIAN_POINT('Ctrl Pts',(-35.6087810892669,-5.72100919352294,
31.485975850882));
#26524=CARTESIAN_POINT('Ctrl Pts',(-35.7020590377777,-5.37442444069083,
31.7688501306084));
#26525=CARTESIAN_POINT('Ctrl Pts',(-36.0726730777933,-5.50017071946578,
31.5328901029015));
#26526=CARTESIAN_POINT('Origin',(-38.4603055734906,-12.8919045823054,39.1356156285706));
#26527=CARTESIAN_POINT('Ctrl Pts',(-36.101076272966,-7.07886051013274,32.9789079716315));
#26528=CARTESIAN_POINT('Ctrl Pts',(-36.0899132796569,-6.97591157388736,
32.9450525778012));
#26529=CARTESIAN_POINT('Ctrl Pts',(-36.0884195965777,-6.87711064623164,
32.898798434336));
#26530=CARTESIAN_POINT('Ctrl Pts',(-36.0959936162844,-6.68740381001555,
32.7941789389639));
#26531=CARTESIAN_POINT('Ctrl Pts',(-36.1053616074735,-6.59673597566757,
32.7354819475306));
#26532=CARTESIAN_POINT('Ctrl Pts',(-36.1345672829262,-6.42451466437637,
32.6062788880432));
#26533=CARTESIAN_POINT('Ctrl Pts',(-36.1540093300512,-6.34396835910597,
32.5368889705491));
#26534=CARTESIAN_POINT('Ctrl Pts',(-36.1942336893731,-6.23614184370368,
32.4215531154926));
#26535=CARTESIAN_POINT('Ctrl Pts',(-36.2094997401739,-6.2025085626214,32.3812785420796));
#26536=CARTESIAN_POINT('Ctrl Pts',(-36.245538447344,-6.14483638321708,32.2965923390849));
#26537=CARTESIAN_POINT('Ctrl Pts',(-36.2661556687914,-6.11985717446073,
32.2519654539084));
#26538=CARTESIAN_POINT('Ctrl Pts',(-36.2923483136821,-6.10843371318468,
32.2050467999301));
#26539=CARTESIAN_POINT('Origin',(0.0835265683620477,-14.4544045823054,0.0824317919394229));
#26540=CARTESIAN_POINT('Origin',(-37.6790715732587,-14.4544045823054,43.2010819542467));
#26541=CARTESIAN_POINT('Origin',(-11.548656164376,-14.4544045823054,-33.4956062992654));
#26542=CARTESIAN_POINT('Origin',(-20.394360840366,-14.4544045823054,-6.6701627853663));
#26543=CARTESIAN_POINT('Origin',(-36.6439262383654,-14.4544045823054,42.6081948668641));
#26544=CARTESIAN_POINT('Ctrl Pts',(-46.3756986917116,-14.426701821065,-31.967386032015));
#26545=CARTESIAN_POINT('Ctrl Pts',(-46.3877592862997,-14.7669045823054,
-31.9392629591333));
#26546=CARTESIAN_POINT('Ctrl Pts',(-46.2541665130207,-14.7669045823054,
-32.2540056786749));
#26547=CARTESIAN_POINT('Ctrl Pts',(-46.5262167757777,-14.4797609665103,
-32.0258294594699));
#26548=CARTESIAN_POINT('Ctrl Pts',(-46.4971544532193,-14.7669045823055,
-32.0448734520714));
#26549=CARTESIAN_POINT('Ctrl Pts',(-46.4502337580146,-14.7669045823054,
-32.3366490875369));
#26550=CARTESIAN_POINT('Ctrl Pts',(-46.6937109365492,-14.5360769750864,
-32.0634681128903));
#26551=CARTESIAN_POINT('Ctrl Pts',(-46.6746692672182,-14.7669045823052,
-32.1327773356701));
#26552=CARTESIAN_POINT('Ctrl Pts',(-46.6742499978977,-14.7669045823054,
-32.3756703660879));
#26553=CARTESIAN_POINT('Ctrl Pts',(-47.0039073691806,-14.6333609973518,
-32.0644095936465));
#26554=CARTESIAN_POINT('Ctrl Pts',(-47.0271134517325,-14.7669045823056,
-32.1591547728184));
#26555=CARTESIAN_POINT('Ctrl Pts',(-47.1033317152047,-14.7669045823054,
-32.3146159839169));
#26556=CARTESIAN_POINT('Ctrl Pts',(-47.1546671567785,-14.6768299128525,
-32.0274598660431));
#26557=CARTESIAN_POINT('Ctrl Pts',(-47.2215585124842,-14.7669045823053,
-32.109304007213));
#26558=CARTESIAN_POINT('Ctrl Pts',(-47.3201303649606,-14.7669045823054,
-32.2117463895627));
#26559=CARTESIAN_POINT('Ctrl Pts',(-47.2003152129085,-14.6796363815825,
-31.9161588440568));
#26560=CARTESIAN_POINT('Ctrl Pts',(-47.2868308580741,-14.7669045823054,
-31.9448707178761));
#26561=CARTESIAN_POINT('Ctrl Pts',(-47.4053176024544,-14.7669045823054,
-31.9879994785672));
#26562=CARTESIAN_POINT('Origin',(-46.3543559346078,-14.4544045823054,-32.2915721687179));
#26563=CARTESIAN_POINT('Ctrl Pts',(-38.1837705810014,-12.8919045823054,
-29.2682655958051));
#26564=CARTESIAN_POINT('Ctrl Pts',(-38.3959057211593,-12.8919045823054,
-29.3382172743398));
#26565=CARTESIAN_POINT('Ctrl Pts',(-38.5307586915594,-12.8919045823054,
-29.1601464137424));
#26566=CARTESIAN_POINT('Ctrl Pts',(-38.183770659511,-13.0608832998915,-29.2682656216937));
#26567=CARTESIAN_POINT('Ctrl Pts',(-38.3959057800757,-12.9975414109163,
-29.3382172937695));
#26568=CARTESIAN_POINT('Ctrl Pts',(-38.5307587078212,-12.9763939382003,
-29.1601463922689));
#26569=CARTESIAN_POINT('Ctrl Pts',(-38.2565492552502,-13.2263898891533,
-29.2922644034588));
#26570=CARTESIAN_POINT('Ctrl Pts',(-38.4533226892664,-13.1003236725306,
-29.3571505509882));
#26571=CARTESIAN_POINT('Ctrl Pts',(-38.574755077224,-13.0591472399314,-29.1621091252889));
#26572=CARTESIAN_POINT('Ctrl Pts',(-38.4907620671097,-13.453458690012,-29.3694962063167));
#26573=CARTESIAN_POINT('Ctrl Pts',(-38.6179212721247,-13.2166231342359,
-29.4114270237444));
#26574=CARTESIAN_POINT('Ctrl Pts',(-38.7160379547609,-13.1726816319567,
-29.1687114403196));
#26575=CARTESIAN_POINT('Ctrl Pts',(-38.6517584445698,-13.5169045492971,
-29.4225848498718));
#26576=CARTESIAN_POINT('Ctrl Pts',(-38.7263955296224,-13.2287751252084,
-29.4471964695062));
#26577=CARTESIAN_POINT('Ctrl Pts',(-38.8130299365641,-13.2044045823054,
-29.1733787082547));
#26578=CARTESIAN_POINT('Ctrl Pts',(-38.8106378122312,-13.5169045823054,
-29.4749754082874));
#26579=CARTESIAN_POINT('Ctrl Pts',(-38.8106378122312,-13.2044045823054,
-29.4749754082874));
#26580=CARTESIAN_POINT('Ctrl Pts',(-38.9085015017574,-13.2044045823054,
-29.1781944313494));
#26581=CARTESIAN_POINT('Ctrl Pts',(-34.2453168949582,-10.7044045823054,
-34.0895144903673));
#26582=CARTESIAN_POINT('Ctrl Pts',(-34.2453168949582,-11.0169045823054,
-34.0895144903673));
#26583=CARTESIAN_POINT('Ctrl Pts',(-34.0238404855175,-11.0169045823054,
-33.869050320804));
#26584=CARTESIAN_POINT('Ctrl Pts',(-34.1831061101228,-10.7044046073823,
-34.1520109099947));
#26585=CARTESIAN_POINT('Ctrl Pts',(-34.2067524199087,-11.0349449313269,
-34.1282560290212));
#26586=CARTESIAN_POINT('Ctrl Pts',(-33.9742956506306,-11.0169045823054,
-33.8939502540348));
#26587=CARTESIAN_POINT('Ctrl Pts',(-34.1223018123232,-10.7186506766711,
-34.2127522663462));
#26588=CARTESIAN_POINT('Ctrl Pts',(-34.174388313845,-11.0630714156278,-34.160693357711));
#26589=CARTESIAN_POINT('Ctrl Pts',(-33.9258201978111,-11.0240276257398,
-33.9181007183444));
#26590=CARTESIAN_POINT('Ctrl Pts',(-34.0041449959219,-10.7765752156549,
-34.3301965896023));
#26591=CARTESIAN_POINT('Ctrl Pts',(-34.1234350039619,-11.1314870357705,
-34.2119315641541));
#26592=CARTESIAN_POINT('Ctrl Pts',(-33.8315341822154,-11.0529899027286,
-33.9647086119291));
#26593=CARTESIAN_POINT('Ctrl Pts',(-33.9500964242875,-10.8185639645428,
-34.3836165482575));
#26594=CARTESIAN_POINT('Ctrl Pts',(-34.107426121419,-11.1704305366376,-34.2281661619454));
#26595=CARTESIAN_POINT('Ctrl Pts',(-33.7883601256341,-11.0739842709864,
-33.985863384623));
#26596=CARTESIAN_POINT('Ctrl Pts',(-33.853696255335,-10.9314866347395,-34.4785417072161));
#26597=CARTESIAN_POINT('Ctrl Pts',(-34.0922214904,-11.2441510617713,-34.2442295368161));
#26598=CARTESIAN_POINT('Ctrl Pts',(-33.7113032982434,-11.1304456109602,
-34.0234016807259));
#26599=CARTESIAN_POINT('Ctrl Pts',(-33.8143209924547,-10.9992937157271,
-34.5171182906613));
#26600=CARTESIAN_POINT('Ctrl Pts',(-34.0948903060196,-11.275032611406,-34.2421982080992));
#26601=CARTESIAN_POINT('Ctrl Pts',(-33.6797999541619,-11.1643491474262,
-34.0386274161058));
#26602=CARTESIAN_POINT('Ctrl Pts',(-33.7584154529392,-11.1560957480195,
-34.571801649325));
#26603=CARTESIAN_POINT('Ctrl Pts',(-34.1052494433068,-11.3160025899705,
-34.2330567165343));
#26604=CARTESIAN_POINT('Ctrl Pts',(-33.6350580487545,-11.2427501667525,
-34.0601969961866));
#26605=CARTESIAN_POINT('Ctrl Pts',(-33.7434406299571,-11.2411599901508,
-34.5863970953167));
#26606=CARTESIAN_POINT('Ctrl Pts',(-34.111705002517,-11.3235538600013,-34.2270752707322));
#26607=CARTESIAN_POINT('Ctrl Pts',(-33.6230658263241,-11.2852822850309,
-34.0659462397595));
#26608=CARTESIAN_POINT('Ctrl Pts',(-33.7434406426353,-11.3294045823054,
-34.5863970829463));
#26609=CARTESIAN_POINT('Ctrl Pts',(-34.1117049987155,-11.3294045823054,
-34.2270752742097));
#26610=CARTESIAN_POINT('Ctrl Pts',(-33.6230658340261,-11.3294045823054,
-34.0659462422992));
#26611=CARTESIAN_POINT('Origin',(-34.0238404855175,-10.7044045823054,-33.869050320804));
#26612=CARTESIAN_POINT('Origin',(10.2095634989472,-11.3294045823054,19.8244816432194));
#26613=CARTESIAN_POINT('Ctrl Pts',(38.3508237177255,-12.8919045823054,29.4331291796839));
#26614=CARTESIAN_POINT('Ctrl Pts',(38.5629588578834,-12.8919045823054,29.5030808582187));
#26615=CARTESIAN_POINT('Ctrl Pts',(38.6978118282835,-12.8919045823054,29.3250099976212));
#26616=CARTESIAN_POINT('Ctrl Pts',(38.350823796233,-13.0608832998915,29.4331292055718));
#26617=CARTESIAN_POINT('Ctrl Pts',(38.5629589167962,-12.9975414109165,29.5030808776454));
#26618=CARTESIAN_POINT('Ctrl Pts',(38.6978118445448,-12.9763939382002,29.3250099761484));
#26619=CARTESIAN_POINT('Ctrl Pts',(38.4236023919749,-13.2263898891533,29.4571279873378));
#26620=CARTESIAN_POINT('Ctrl Pts',(38.620375825991,-13.1003236725305,29.5220141348676));
#26621=CARTESIAN_POINT('Ctrl Pts',(38.7418082139485,-13.0591472399316,29.3269727091676));
#26622=CARTESIAN_POINT('Ctrl Pts',(38.6578152038332,-13.453458690012,29.5343597901954));
#26623=CARTESIAN_POINT('Ctrl Pts',(38.7849744088482,-13.2166231342361,29.5762906076227));
#26624=CARTESIAN_POINT('Ctrl Pts',(38.8830910914846,-13.1726816319565,29.3335750241986));
#26625=CARTESIAN_POINT('Ctrl Pts',(38.8188115812943,-13.5169045492971,29.5874484337508));
#26626=CARTESIAN_POINT('Ctrl Pts',(38.8934486663472,-13.2287751252085,29.6120600533846));
#26627=CARTESIAN_POINT('Ctrl Pts',(38.9800830732885,-13.2044045823054,29.3382422921337));
#26628=CARTESIAN_POINT('Ctrl Pts',(38.9776909489554,-13.5169045823054,29.6398389921663));
#26629=CARTESIAN_POINT('Ctrl Pts',(38.9776909489554,-13.2044045823054,29.6398389921663));
#26630=CARTESIAN_POINT('Ctrl Pts',(39.0755546384815,-13.2044045823054,29.3430580152282));
#26631=CARTESIAN_POINT('Origin',(38.4486874072517,-12.8919045823054,29.1363482027458));
#26632=CARTESIAN_POINT('Ctrl Pts',(-36.1113722880935,-7.15534954836531,
33.0016931755516));
#26633=CARTESIAN_POINT('Ctrl Pts',(-35.9763481816599,-7.11664814652194,
32.4278063923816));
#26634=CARTESIAN_POINT('Ctrl Pts',(-35.5783817078538,-7.18677502450287,
32.8607815258895));
#26635=CARTESIAN_POINT('Ctrl Pts',(-36.0918388255004,-7.0323813740435,32.9705852224084));
#26636=CARTESIAN_POINT('Ctrl Pts',(-35.9090565323606,-7.08021162564815,
32.5013078276263));
#26637=CARTESIAN_POINT('Ctrl Pts',(-35.564706282625,-7.01162141061937,32.8756284637236));
#26638=CARTESIAN_POINT('Ctrl Pts',(-36.0873692866412,-6.90078625143554,
32.9127559686128));
#26639=CARTESIAN_POINT('Ctrl Pts',(-35.8673102683238,-6.94927177587728,
32.5462760319206));
#26640=CARTESIAN_POINT('Ctrl Pts',(-35.585966365718,-6.83269992246867,32.8525765797321));
#26641=CARTESIAN_POINT('Ctrl Pts',(-36.0969671734838,-6.67697195553551,
32.7883008612393));
#26642=CARTESIAN_POINT('Ctrl Pts',(-35.8606408249945,-6.69622936404145,
32.5523589912722));
#26643=CARTESIAN_POINT('Ctrl Pts',(-35.6598372587195,-6.53795985193932,
32.7719667293062));
#26644=CARTESIAN_POINT('Ctrl Pts',(-36.1074306592358,-6.58104909157621,
32.7253234355767));
#26645=CARTESIAN_POINT('Ctrl Pts',(-35.8746421662079,-6.57996991861085,
32.5365087108499));
#26646=CARTESIAN_POINT('Ctrl Pts',(-35.7054143329339,-6.41511471179787,
32.7221349900562));
#26647=CARTESIAN_POINT('Ctrl Pts',(-36.1398197461798,-6.40173475569592,
32.587610085579));
#26648=CARTESIAN_POINT('Ctrl Pts',(-35.9337948307645,-6.36383534698761,
32.4703146792546));
#26649=CARTESIAN_POINT('Ctrl Pts',(-35.8188321691327,-6.19278444406303,
32.597338416161));
#26650=CARTESIAN_POINT('Ctrl Pts',(-36.161056277475,-6.32050524456483,32.5150029822516));
#26651=CARTESIAN_POINT('Ctrl Pts',(-35.9753922140543,-6.26307762141936,
32.4239108003766));
#26652=CARTESIAN_POINT('Ctrl Pts',(-35.8846472105432,-6.0958003221978,32.5246216325155));
#26653=CARTESIAN_POINT('Ctrl Pts',(-36.2247954239019,-6.1637311406174,32.3388151446257));
#26654=CARTESIAN_POINT('Ctrl Pts',(-36.0984890197755,-6.07811517886866,
32.2859259488243));
#26655=CARTESIAN_POINT('Ctrl Pts',(-36.0617904772832,-5.92198390396995,
32.3272652323252));
#26656=CARTESIAN_POINT('Ctrl Pts',(-36.2697309116477,-6.09886182624416,
32.2364305893108));
#26657=CARTESIAN_POINT('Ctrl Pts',(-36.1863184857959,-6.00005797774074,
32.1870934995707));
#26658=CARTESIAN_POINT('Ctrl Pts',(-36.1766072923992,-5.86097989286269,
32.1982982661301));
#26659=CARTESIAN_POINT('Ctrl Pts',(-36.3252333085416,-6.10268725738925,
32.1504346278648));
#26660=CARTESIAN_POINT('Ctrl Pts',(-36.2789940619947,-6.01584203958864,
32.0817863832517));
#26661=CARTESIAN_POINT('Ctrl Pts',(-36.2968040480299,-5.898811532747,32.0615249766501));
#26662=CARTESIAN_POINT('Ctrl Pts',(-38.5771295391607,-12.5761796977906,
39.1976374646442));
#26663=CARTESIAN_POINT('Ctrl Pts',(-38.1814665062544,-12.4966730216623,
39.4769498488669));
#26664=CARTESIAN_POINT('Ctrl Pts',(-38.1281921118528,-12.8445798972105,
39.1371073079634));
#26665=CARTESIAN_POINT('Ctrl Pts',(-38.6656700537214,-12.7679658886679,
39.3797570567454));
#26666=CARTESIAN_POINT('Ctrl Pts',(-38.3164513392329,-12.6138199372472,
39.5074230596676));
#26667=CARTESIAN_POINT('Ctrl Pts',(-38.2040132293918,-12.9405865508062,
39.3235687157183));
#26668=CARTESIAN_POINT('Ctrl Pts',(-38.6835395010857,-12.9477999797135,
39.6148827885762));
#26669=CARTESIAN_POINT('Ctrl Pts',(-38.4171318344341,-12.8036087634358,
39.6739467335942));
#26670=CARTESIAN_POINT('Ctrl Pts',(-38.2488933633745,-13.0304169137555,
39.5493551304408));
#26671=CARTESIAN_POINT('Ctrl Pts',(-38.6136496865685,-13.1418528526573,
39.9537410970356));
#26672=CARTESIAN_POINT('Ctrl Pts',(-38.4275839700741,-13.0167291165574,
39.9599051875636));
#26673=CARTESIAN_POINT('Ctrl Pts',(-38.2612346165967,-13.1274080636024,
39.8605733849698));
#26674=CARTESIAN_POINT('Ctrl Pts',(-38.5809055860187,-13.1924895597096,
40.0560225836614));
#26675=CARTESIAN_POINT('Ctrl Pts',(-38.4187069710969,-13.0721360087909,
40.0454055866277));
#26676=CARTESIAN_POINT('Ctrl Pts',(-38.2585765398713,-13.1527155106484,
39.9527626777571));
#26677=CARTESIAN_POINT('Ctrl Pts',(-38.4632970463556,-13.2848578326183,
40.2976226616114));
#26678=CARTESIAN_POINT('Ctrl Pts',(-38.3591702059311,-13.1766908654361,
40.2474509195671));
#26679=CARTESIAN_POINT('Ctrl Pts',(-38.2302344992928,-13.1988763557094,
40.1644744741364));
#26680=CARTESIAN_POINT('Ctrl Pts',(-38.3630673365025,-13.3151873395653,
40.4354786226433));
#26681=CARTESIAN_POINT('Ctrl Pts',(-38.2948355383256,-13.2202535090903,
40.3691988363216));
#26682=CARTESIAN_POINT('Ctrl Pts',(-38.1960676382616,-13.2140287022007,
40.2800075145154));
#26683=CARTESIAN_POINT('Ctrl Pts',(-38.2173764537126,-13.2823030560807,
40.5281034214334));
#26684=CARTESIAN_POINT('Ctrl Pts',(-38.187738902338,-13.2034487358311,40.4475707889938));
#26685=CARTESIAN_POINT('Ctrl Pts',(-38.1297266991476,-13.1975864244367,
40.346688751385));
#26686=CARTESIAN_POINT('Ctrl Pts',(-38.1790905589799,-13.2044045823054,
40.2785649063406));
#26687=CARTESIAN_POINT('Ctrl Pts',(-38.1856818137954,-13.2044045823054,
40.2663278736349));
#26688=CARTESIAN_POINT('Ctrl Pts',(-38.1915975569677,-13.2039200465849,
40.2538279098479));
#26689=CARTESIAN_POINT('Ctrl Pts',(-38.1969375577795,-13.2030865921358,
40.2411359927187));
#26690=CARTESIAN_POINT('Ctrl Pts',(-38.2024977186271,-13.2022187756393,
40.2279208073302));
#26691=CARTESIAN_POINT('Ctrl Pts',(-38.2074344665983,-13.2009724747263,
40.2144972565484));
#26692=CARTESIAN_POINT('Ctrl Pts',(-38.2118784236692,-13.199446062585,40.2009395294364));
#26693=CARTESIAN_POINT('Ctrl Pts',(-38.2165642026475,-13.1978365893588,
40.1866440464508));
#26694=CARTESIAN_POINT('Ctrl Pts',(-38.2207027909829,-13.1959155151288,
40.1721991593937));
#26695=CARTESIAN_POINT('Ctrl Pts',(-38.2244552324016,-13.1937414656796,
40.157689229008));
#26696=CARTESIAN_POINT('Ctrl Pts',(-38.2252951287549,-13.1932548554969,
40.1544415200478));
#26697=CARTESIAN_POINT('Ctrl Pts',(-38.226115686824,-13.1927553638524,40.1511905502003));
#26698=CARTESIAN_POINT('Ctrl Pts',(-38.2269187125116,-13.1922433006301,
40.1479372654108));
#26699=CARTESIAN_POINT('Ctrl Pts',(-38.2314857089357,-13.1893310763501,
40.1294350677485));
#26700=CARTESIAN_POINT('Ctrl Pts',(-38.2354089008154,-13.1860397456251,
40.1108869668906));
#26701=CARTESIAN_POINT('Ctrl Pts',(-38.2387936588154,-13.1824628010599,
40.09230074261));
#26702=CARTESIAN_POINT('Ctrl Pts',(-38.2423548715809,-13.1786993826273,
40.0727455782024));
#26703=CARTESIAN_POINT('Ctrl Pts',(-38.2453207997392,-13.1746195596086,
40.0531479638576));
#26704=CARTESIAN_POINT('Ctrl Pts',(-38.247815409911,-13.1702746943006,40.0335165509597));
#26705=CARTESIAN_POINT('Ctrl Pts',(-38.2486922977607,-13.1687474177584,
40.0266158545555));
#26706=CARTESIAN_POINT('Ctrl Pts',(-38.2495109068342,-13.1671869117775,
40.019710995831));
#26707=CARTESIAN_POINT('Ctrl Pts',(-38.2502764087794,-13.1655939279676,
40.0128024206661));
#26708=CARTESIAN_POINT('Ctrl Pts',(-38.2531564049936,-13.1596007526788,
39.9868107554002));
#26709=CARTESIAN_POINT('Ctrl Pts',(-38.2552721004159,-13.1531817886309,
39.9609037786925));
#26710=CARTESIAN_POINT('Ctrl Pts',(-38.2567195588292,-13.1464435609449,
39.9350831105545));
#26711=CARTESIAN_POINT('Ctrl Pts',(-38.2582169555115,-13.1394728599642,
39.9083716123535));
#26712=CARTESIAN_POINT('Ctrl Pts',(-38.2590000580469,-13.1321600180536,
39.8817522013977));
#26713=CARTESIAN_POINT('Ctrl Pts',(-38.2591711854353,-13.1245659628583,
39.8552280016203));
#26714=CARTESIAN_POINT('Ctrl Pts',(-38.2593494923536,-13.1166533043877,
39.8275909975895));
#26715=CARTESIAN_POINT('Ctrl Pts',(-38.2588642050127,-13.1084348255795,
39.8000570949086));
#26716=CARTESIAN_POINT('Ctrl Pts',(-38.2578137673921,-13.0999262547331,
39.7726355324511));
#26717=CARTESIAN_POINT('Ctrl Pts',(-38.2574542693167,-13.0970143113833,
39.763250873396));
#26718=CARTESIAN_POINT('Ctrl Pts',(-38.2570283786661,-13.094067983939,39.753879437865));
#26719=CARTESIAN_POINT('Ctrl Pts',(-38.2565393565581,-13.0910867263844,
39.744521822069));
#26720=CARTESIAN_POINT('Ctrl Pts',(-38.254737729453,-13.0801033488869,39.7100470325268));
#26721=CARTESIAN_POINT('Ctrl Pts',(-38.2520429901721,-13.0686901791307,
39.6757525940363));
#26722=CARTESIAN_POINT('Ctrl Pts',(-38.2485217298626,-13.0568974025755,
39.6416630585085));
#26723=CARTESIAN_POINT('Ctrl Pts',(-38.244892138822,-13.0447418240704,39.6065247665745));
#26724=CARTESIAN_POINT('Ctrl Pts',(-38.2403853064657,-13.0321818870426,
39.5716038765946));
#26725=CARTESIAN_POINT('Ctrl Pts',(-38.2350383815156,-13.0192318837648,
39.5369390751942));
#26726=CARTESIAN_POINT('Ctrl Pts',(-38.229762434248,-13.0064537851295,39.5027344312285));
#26727=CARTESIAN_POINT('Ctrl Pts',(-38.2236689920591,-12.9932945861615,
39.4687789762929));
#26728=CARTESIAN_POINT('Ctrl Pts',(-38.2167496847683,-12.9797471343051,
39.4351244052383));
#26729=CARTESIAN_POINT('Ctrl Pts',(-38.2096907485999,-12.9659263002422,
39.4007906982848));
#26730=CARTESIAN_POINT('Ctrl Pts',(-38.2017728575461,-12.9516999140197,
39.3667699506476));
#26731=CARTESIAN_POINT('Ctrl Pts',(-38.1929328601229,-12.9370593466235,
39.333134943979));
#26732=CARTESIAN_POINT('Ctrl Pts',(-38.1848265223924,-12.923633846796,39.3022914142165));
#26733=CARTESIAN_POINT('Ctrl Pts',(-38.1759442687234,-12.9098590019422,
39.2717724245339));
#26734=CARTESIAN_POINT('Ctrl Pts',(-38.1661935582769,-12.8957449858576,
39.241648555329));
#26735=CARTESIAN_POINT('Ctrl Pts',(-38.1653110755248,-12.894467604499,39.2389222109108));
#26736=CARTESIAN_POINT('Ctrl Pts',(-38.1644214502429,-12.8931874634454,
39.2361991124934));
#26737=CARTESIAN_POINT('Ctrl Pts',(-38.1635245965525,-12.8919045823054,
39.2334793180968));
#26738=CARTESIAN_POINT('Origin',(-38.1790905589799,-13.5169045823054,40.2785649063406));
#26739=CARTESIAN_POINT('Ctrl Pts',(-37.571637427794,-14.6563598281178,42.9623413980297));
#26740=CARTESIAN_POINT('Ctrl Pts',(-37.6481685929094,-14.766904582306,43.0141807834233));
#26741=CARTESIAN_POINT('Ctrl Pts',(-37.7683428080284,-14.7669045823054,
43.0948662445537));
#26742=CARTESIAN_POINT('Ctrl Pts',(-37.5504823732842,-14.6732979129414,
43.0240609128249));
#26743=CARTESIAN_POINT('Ctrl Pts',(-37.620400171357,-14.7669045823051,43.088122727466));
#26744=CARTESIAN_POINT('Ctrl Pts',(-37.7152507551813,-14.7669045823054,
43.1831284322925));
#26745=CARTESIAN_POINT('Ctrl Pts',(-37.5105015173806,-14.6836226395025,
43.0705954951548));
#26746=CARTESIAN_POINT('Ctrl Pts',(-37.5601429670254,-14.7669045823055,
43.1488125001359));
#26747=CARTESIAN_POINT('Ctrl Pts',(-37.6278053714458,-14.7669045823054,
43.2554532213409));
#26748=CARTESIAN_POINT('Ctrl Pts',(-37.4326597803442,-14.683707174412,43.0965368861083));
#26749=CARTESIAN_POINT('Ctrl Pts',(-37.4491318676269,-14.7669045823053,
43.1857463359048));
#26750=CARTESIAN_POINT('Ctrl Pts',(-37.4715757338329,-14.7669045823054,
43.3073250486046));
#26751=CARTESIAN_POINT('Ctrl Pts',(-37.4019081671593,-14.6805726740677,
43.0965521057182));
#26752=CARTESIAN_POINT('Ctrl Pts',(-37.4057521162803,-14.7669045823054,
43.1877618665153));
#26753=CARTESIAN_POINT('Ctrl Pts',(-37.4120037026109,-14.7669045823054,
43.313802830833));
#26754=CARTESIAN_POINT('Ctrl Pts',(-37.308677175366,-14.6635276241073,43.0722215122081));
#26755=CARTESIAN_POINT('Ctrl Pts',(-37.2781492406654,-14.7669045823054,
43.1635368742967));
#26756=CARTESIAN_POINT('Ctrl Pts',(-37.2365609420744,-14.7669045823054,
43.3000505843005));
#26757=CARTESIAN_POINT('Ctrl Pts',(-37.2461501425878,-14.6424796666936,
43.0248183412419));
#26758=CARTESIAN_POINT('Ctrl Pts',(-37.1977923649815,-14.7669045823054,
43.1070361827516));
#26759=CARTESIAN_POINT('Ctrl Pts',(-37.1254898316105,-14.7669045823054,
43.2482346286421));
#26760=CARTESIAN_POINT('Ctrl Pts',(-37.0594384684801,-14.5607785229691,
42.822087643319));
#26761=CARTESIAN_POINT('Ctrl Pts',(-36.9754363879768,-14.7669045823054,
42.8589117372199));
#26762=CARTESIAN_POINT('Ctrl Pts',(-36.8069422637988,-14.7669045823054,
43.0097426982014));
#26763=CARTESIAN_POINT('Ctrl Pts',(-36.9640663188338,-14.4859905466075,
42.6111924580297));
#26764=CARTESIAN_POINT('Ctrl Pts',(-36.9195590626158,-14.7669045823054,
42.5868389181748));
#26765=CARTESIAN_POINT('Ctrl Pts',(-36.667453837466,-14.7669045823054,42.7409248107066));
#26766=CARTESIAN_POINT('Ctrl Pts',(-36.9104618122751,-14.4183787521222,
42.408858845907));
#26767=CARTESIAN_POINT('Ctrl Pts',(-36.9508214922036,-14.7669045823054,
42.4006555962426));
#26768=CARTESIAN_POINT('Ctrl Pts',(-36.6071448023002,-14.7669045823054,
42.4758120956255));
#26769=CARTESIAN_POINT('Ctrl Pts',(-36.9407072321466,-14.4544045238109,
42.5103312284163));
#26770=CARTESIAN_POINT('Ctrl Pts',(-36.9503813816065,-14.4643868520269,
42.5396690097907));
#26771=CARTESIAN_POINT('Ctrl Pts',(-36.9608880608343,-14.474401186739,42.568722463887));
#26772=CARTESIAN_POINT('Ctrl Pts',(-36.9722124826523,-14.48440991971,42.5974253617278));
#26773=CARTESIAN_POINT('Ctrl Pts',(-36.9833401708954,-14.4942447759172,
42.6256296183318));
#26774=CARTESIAN_POINT('Ctrl Pts',(-36.9952567764507,-14.5040728389243,
42.6534969499852));
#26775=CARTESIAN_POINT('Ctrl Pts',(-37.0079962202933,-14.5138432176011,
42.6809634158137));
#26776=CARTESIAN_POINT('Ctrl Pts',(-37.0196774642178,-14.5228020212953,
42.7061483839371));
#26777=CARTESIAN_POINT('Ctrl Pts',(-37.0320511295469,-14.5317110776814,
42.7309973259379));
#26778=CARTESIAN_POINT('Ctrl Pts',(-37.0451828697107,-14.5405368969067,
42.7554423470322));
#26779=CARTESIAN_POINT('Ctrl Pts',(-37.0576149177858,-14.5488924543227,
42.7785848760231));
#26780=CARTESIAN_POINT('Ctrl Pts',(-37.0707272229527,-14.5571724059614,
42.8013660847167));
#26781=CARTESIAN_POINT('Ctrl Pts',(-37.0846026821019,-14.5653692837006,
42.8236990877515));
#26782=CARTESIAN_POINT('Ctrl Pts',(-37.0974382804467,-14.5729518673982,
42.8443584009825));
#26783=CARTESIAN_POINT('Ctrl Pts',(-37.1109279894093,-14.5804628051681,
42.864634363072));
#26784=CARTESIAN_POINT('Ctrl Pts',(-37.1251480886583,-14.5879251019716,
42.8844266395982));
#26785=CARTESIAN_POINT('Ctrl Pts',(-37.1324432310159,-14.5917533816863,
42.8945803995904));
#26786=CARTESIAN_POINT('Ctrl Pts',(-37.1399306955635,-14.5955693937985,
42.9046063116132));
#26787=CARTESIAN_POINT('Ctrl Pts',(-37.1476204401308,-14.5993802185554,
42.9144870863799));
#26788=CARTESIAN_POINT('Ctrl Pts',(-37.157835260641,-14.6044424011217,42.9276124041145));
#26789=CARTESIAN_POINT('Ctrl Pts',(-37.1683738566588,-14.6095732512801,
42.940512250732));
#26790=CARTESIAN_POINT('Ctrl Pts',(-37.1793254324901,-14.6146451518329,
42.9530852762723));
#26791=CARTESIAN_POINT('Ctrl Pts',(-37.189587205736,-14.619397590587,42.9648663696143));
#26792=CARTESIAN_POINT('Ctrl Pts',(-37.2002124359805,-14.624097891655,42.976360600664));
#26793=CARTESIAN_POINT('Ctrl Pts',(-37.2112872605342,-14.6286695523061,
42.9874527708991));
#26794=CARTESIAN_POINT('Ctrl Pts',(-37.2219162798294,-14.6330571856303,
42.9980984376436));
#26795=CARTESIAN_POINT('Ctrl Pts',(-37.2329603033943,-14.6373259480376,
43.0083738395466));
#26796=CARTESIAN_POINT('Ctrl Pts',(-37.2444954462343,-14.6414408657884,
43.0181454813071));
#26797=CARTESIAN_POINT('Ctrl Pts',(-37.2557075809083,-14.6454405572214,
43.0276434966264));
#26798=CARTESIAN_POINT('Ctrl Pts',(-37.2673847753206,-14.6492945993133,
43.0366655113334));
#26799=CARTESIAN_POINT('Ctrl Pts',(-37.2795829118597,-14.6530074411929,
43.045058089822));
#26800=CARTESIAN_POINT('Ctrl Pts',(-37.2910154425439,-14.6564872496521,
43.0529239151293));
#26801=CARTESIAN_POINT('Ctrl Pts',(-37.3029064669486,-14.6598432010014,
43.0602363732956));
#26802=CARTESIAN_POINT('Ctrl Pts',(-37.3152758152603,-14.6631120254243,
43.0668456988466));
#26803=CARTESIAN_POINT('Ctrl Pts',(-37.316104157274,-14.6633309298109,43.0672883076161));
#26804=CARTESIAN_POINT('Ctrl Pts',(-37.3169346310621,-14.6635494557759,
43.067727755555));
#26805=CARTESIAN_POINT('Ctrl Pts',(-37.3177672364761,-14.6637676196426,
43.0681639945637));
#26806=CARTESIAN_POINT('Ctrl Pts',(-37.3288904156748,-14.6666821764584,
43.0739919228776));
#26807=CARTESIAN_POINT('Ctrl Pts',(-37.3404597867255,-14.6694736866496,
43.0792128120357));
#26808=CARTESIAN_POINT('Ctrl Pts',(-37.3523931238171,-14.6719975663698,
43.0834732187685));
#26809=CARTESIAN_POINT('Ctrl Pts',(-37.363947582839,-14.6744413140473,43.0875983595094));
#26810=CARTESIAN_POINT('Ctrl Pts',(-37.3758439124062,-14.6766346712664,
43.0908223244708));
#26811=CARTESIAN_POINT('Ctrl Pts',(-37.3879640412811,-14.6784666962726,
43.0928188912063));
#26812=CARTESIAN_POINT('Ctrl Pts',(-37.3996182825084,-14.6802282997653,
43.0947387115814));
#26813=CARTESIAN_POINT('Ctrl Pts',(-37.411479676887,-14.6816565741044,43.0955228683507));
#26814=CARTESIAN_POINT('Ctrl Pts',(-37.4233961687224,-14.6826626743679,
43.0948873632353));
#26815=CARTESIAN_POINT('Ctrl Pts',(-37.4263170846554,-14.6829092850592,
43.0947315911304));
#26816=CARTESIAN_POINT('Ctrl Pts',(-37.4292410753172,-14.6831305465446,
43.0944905860586));
#26817=CARTESIAN_POINT('Ctrl Pts',(-37.4321654362444,-14.6833251552392,
43.094160314464));
#26818=CARTESIAN_POINT('Ctrl Pts',(-37.4416164879093,-14.6839540984074,
43.0930929312029));
#26819=CARTESIAN_POINT('Ctrl Pts',(-37.4508975843209,-14.6841943737355,
43.090998399424));
#26820=CARTESIAN_POINT('Ctrl Pts',(-37.4598652509752,-14.6841331258666,
43.0879880811904));
#26821=CARTESIAN_POINT('Ctrl Pts',(-37.4689847795451,-14.6840708408026,
43.0849267850702));
#26822=CARTESIAN_POINT('Ctrl Pts',(-37.4777791878974,-14.6836965195602,
43.0809189561397));
#26823=CARTESIAN_POINT('Ctrl Pts',(-37.4861222057687,-14.6830632794737,
43.0761109723373));
#26824=CARTESIAN_POINT('Ctrl Pts',(-37.4946188905762,-14.682418375974,43.0712144320734));
#26825=CARTESIAN_POINT('Ctrl Pts',(-37.5026467486571,-14.6815043446902,
43.0654887721282));
#26826=CARTESIAN_POINT('Ctrl Pts',(-37.5101105739052,-14.680343837413,43.0591084748772));
#26827=CARTESIAN_POINT('Ctrl Pts',(-37.5178759953978,-14.6791364366697,
43.0524703642896));
#26828=CARTESIAN_POINT('Ctrl Pts',(-37.5250305556585,-14.6776614503336,
43.0451245148125));
#26829=CARTESIAN_POINT('Ctrl Pts',(-37.5315160929354,-14.6759191474477,
43.0372757278879));
#26830=CARTESIAN_POINT('Ctrl Pts',(-37.5321802112215,-14.6757407358286,
43.0364720129916));
#26831=CARTESIAN_POINT('Ctrl Pts',(-37.5328373566078,-14.6755595065434,
43.0356630246841));
#26832=CARTESIAN_POINT('Ctrl Pts',(-37.5334874951132,-14.6753754510087,
43.0348489820804));
#26833=CARTESIAN_POINT('Origin',(0.0835265683620477,-14.4544045823054,0.0824317919394229));
#26834=CARTESIAN_POINT('Origin',(-9.75726988530523,-14.4544045823054,-19.1035039790228));
#26835=CARTESIAN_POINT('Origin',(5.15768816523998,-14.4544045823054,-15.3054474424773));
#26836=CARTESIAN_POINT('Origin',(-9.84678298317079,-14.4544045823054,-20.2531800132168));
#26837=CARTESIAN_POINT('Origin',(0.0835265683620477,-10.7044045823054,0.0824317919394229));
#26838=CARTESIAN_POINT('Origin',(-37.87826784707,-10.7044045823054,-29.4965774842428));
#26839=CARTESIAN_POINT('Origin',(-4.99063502851588,-11.3294045823054,15.4703110263562));
#26840=CARTESIAN_POINT('Origin',(18.7518431265311,-11.3294045823054,23.2994061884498));
#26841=CARTESIAN_POINT('Ctrl Pts',(38.3508237177256,-11.3294045823054,29.4331291796839));
#26842=CARTESIAN_POINT('Ctrl Pts',(38.3508237177256,-11.3124780874426,29.4331291796839));
#26843=CARTESIAN_POINT('Ctrl Pts',(38.3494530102577,-11.2956902155653,29.4341292951345));
#26844=CARTESIAN_POINT('Ctrl Pts',(38.3468401936668,-11.2792729854166,29.4360772676558));
#26845=CARTESIAN_POINT('Ctrl Pts',(38.3442080910596,-11.2627345745579,29.4380396187715));
#26846=CARTESIAN_POINT('Ctrl Pts',(38.3403156398042,-11.2465729047032,29.4409633712592));
#26847=CARTESIAN_POINT('Ctrl Pts',(38.3353075372331,-11.230993405314,29.444754978997));
#26848=CARTESIAN_POINT('Ctrl Pts',(38.3302312794146,-11.2152018845814,29.448598186709));
#26849=CARTESIAN_POINT('Ctrl Pts',(38.3240089967403,-11.2000089946043,29.4533324285803));
#26850=CARTESIAN_POINT('Ctrl Pts',(38.3168021619072,-11.1855875760929,29.4588275743199));
#26851=CARTESIAN_POINT('Ctrl Pts',(38.309537501841,-11.1710504449412,29.4643668112716));
#26852=CARTESIAN_POINT('Ctrl Pts',(38.3012726649942,-11.1572975033337,29.4706784891979));
#26853=CARTESIAN_POINT('Ctrl Pts',(38.2921805812085,-11.1444582968067,29.4776064573043));
#26854=CARTESIAN_POINT('Ctrl Pts',(38.2829617933224,-11.1314401675872,29.4846309711517));
#26855=CARTESIAN_POINT('Ctrl Pts',(38.2728927915826,-11.1193615571096,29.4922883129586));
#26856=CARTESIAN_POINT('Ctrl Pts',(38.2621578342495,-11.1083055247257,29.5004035894501));
#26857=CARTESIAN_POINT('Ctrl Pts',(38.2586229712668,-11.1046649364685,29.5030758302028));
#26858=CARTESIAN_POINT('Ctrl Pts',(38.2550159150995,-11.1011348042002,29.5057976770622));
#26859=CARTESIAN_POINT('Ctrl Pts',(38.251343266964,-11.0977168667273,29.5085628175253));
#26860=CARTESIAN_POINT('Ctrl Pts',(38.237970490606,-11.0852715379768,29.5186311942514));
#26861=CARTESIAN_POINT('Ctrl Pts',(38.2237563987941,-11.0742682117852,29.5293337237824));
#26862=CARTESIAN_POINT('Ctrl Pts',(38.2089071620523,-11.0647125800551,29.5404697723536));
#26863=CARTESIAN_POINT('Ctrl Pts',(38.1922829478517,-11.054014732653,29.5529369489509));
#26864=CARTESIAN_POINT('Ctrl Pts',(38.1748627193941,-11.0451301475312,29.5659473342625));
#26865=CARTESIAN_POINT('Ctrl Pts',(38.1569165881815,-11.0380420023619,29.5792775735416));
#26866=CARTESIAN_POINT('Ctrl Pts',(38.136953098194,-11.0301570653,29.5941062903957));
#26867=CARTESIAN_POINT('Ctrl Pts',(38.116338530399,-11.0244934293336,29.6093317055714));
#26868=CARTESIAN_POINT('Ctrl Pts',(38.0954239674044,-11.0210242012062,29.6247092634801));
#26869=CARTESIAN_POINT('Ctrl Pts',(38.0788552940599,-11.0182758527174,29.6368914799525));
#26870=CARTESIAN_POINT('Ctrl Pts',(38.0620977574343,-11.0169045823054,29.6491709647271));
#26871=CARTESIAN_POINT('Ctrl Pts',(38.0453209837941,-11.0169045823054,29.6614410681217));
#26872=CARTESIAN_POINT('Origin',(38.4486874072517,-14.7669045823054,29.1363482027458));
#26873=CARTESIAN_POINT('Origin',(38.4486874072517,-11.3294045823054,29.1363482027458));
#26874=CARTESIAN_POINT('Origin',(-22.4718276789325,-12.8919045823054,-7.35520861204973));
#26875=CARTESIAN_POINT('Origin',(-35.8042963200226,-12.8919045823054,33.0767747666364));
#26876=CARTESIAN_POINT('Origin',(0.0835265683620477,-13.5169045823054,0.0824317919394229));
#26877=CARTESIAN_POINT('Origin',(-36.9176881394302,-13.5169045823054,41.4426433113705));
#26878=CARTESIAN_POINT('Ctrl Pts',(-37.1002562688466,-14.9232028613467,
42.9941789068619));
#26879=CARTESIAN_POINT('Ctrl Pts',(-37.1882368306857,-14.6181128259927,
43.2609883560109));
#26880=CARTESIAN_POINT('Ctrl Pts',(-37.5425880812871,-14.7022319922259,
43.0625772974519));
#26881=CARTESIAN_POINT('Ctrl Pts',(-36.9406416502711,-14.45386212998,42.510132345121));
#26882=CARTESIAN_POINT('Ctrl Pts',(-37.0285175912917,-14.147074607213,42.7766245216622));
#26883=CARTESIAN_POINT('Ctrl Pts',(-37.3835541595816,-14.232891259592,42.5780223744643));
#26884=CARTESIAN_POINT('Ctrl Pts',(-36.7808584715544,-13.9850662226631,
42.0255746086673));
#26885=CARTESIAN_POINT('Ctrl Pts',(-36.8688690141397,-13.6772499732338,
42.2924749773334));
#26886=CARTESIAN_POINT('Ctrl Pts',(-37.2243639950202,-13.7640953522129,
42.0929401326293));
#26887=CARTESIAN_POINT('Ctrl Pts',(-36.6209071624921,-13.5169045823054,
41.5405070008967));
#26888=CARTESIAN_POINT('Ctrl Pts',(-36.7093350047365,-13.2088427643879,
41.8086728705558));
#26889=CARTESIAN_POINT('Ctrl Pts',(-37.0650186795419,-13.2959337131846,
41.6073303993598));
#26890=CARTESIAN_POINT('Origin',(-36.9176881394302,-13.5169045823054,41.4426433113705));
#26891=CARTESIAN_POINT('Origin',(-10.0425103622231,-14.4544045823054,-19.6596180593406));
#26892=CARTESIAN_POINT('Origin',(-10.0425103622231,-14.4544045823054,-19.6596180593406));
#26893=CARTESIAN_POINT('Ctrl Pts',(-38.5307586915594,-11.3294045823054,
-29.1601464137424));
#26894=CARTESIAN_POINT('Ctrl Pts',(-38.3959057211593,-11.3294045823054,
-29.3382172743398));
#26895=CARTESIAN_POINT('Ctrl Pts',(-38.1837705810015,-11.3294045823054,
-29.2682655958051));
#26896=CARTESIAN_POINT('Ctrl Pts',(-38.530758641258,-11.1601003758277,-29.1601464801644));
#26897=CARTESIAN_POINT('Ctrl Pts',(-38.3959056833756,-11.2236230318997,
-29.3382173235993));
#26898=CARTESIAN_POINT('Ctrl Pts',(-38.1837705555596,-11.2447524820092,
-29.2682655874156));
#26899=CARTESIAN_POINT('Ctrl Pts',(-38.4840830247557,-10.9943058431436,
-29.2219436452516));
#26900=CARTESIAN_POINT('Ctrl Pts',(-38.3590718330862,-11.120480985332,-29.3862883502537));
#26901=CARTESIAN_POINT('Ctrl Pts',(-38.148800374239,-11.1618552084332,-29.2950794305781));
#26902=CARTESIAN_POINT('Ctrl Pts',(-38.3328185949133,-10.7673610427476,
-29.4199639376802));
#26903=CARTESIAN_POINT('Ctrl Pts',(-38.2519922408775,-11.0035905561212,
-29.5250467467008));
#26904=CARTESIAN_POINT('Ctrl Pts',(-38.0351381216391,-11.0483828168177,
-29.3807494825232));
#26905=CARTESIAN_POINT('Ctrl Pts',(-38.2284284200153,-10.7044046130696,
-29.5556172851081));
#26906=CARTESIAN_POINT('Ctrl Pts',(-38.180551033523,-10.9913613137611,-29.6170632772379));
#26907=CARTESIAN_POINT('Ctrl Pts',(-37.9565673174692,-11.0169045823054,
-29.4393112525611));
#26908=CARTESIAN_POINT('Ctrl Pts',(-38.1247730056117,-10.7044045823054,
-29.6886489730492));
#26909=CARTESIAN_POINT('Ctrl Pts',(-38.1247730056117,-11.0169045823054,
-29.6886489730492));
#26910=CARTESIAN_POINT('Ctrl Pts',(-37.87826784707,-11.0169045823054,-29.4965774842428));
#26911=CARTESIAN_POINT('Ctrl Pts',(-37.87826784707,-11.0169045823054,-29.4965774842428));
#26912=CARTESIAN_POINT('Ctrl Pts',(-37.8972057124971,-11.0169045823054,
-29.4827268135568));
#26913=CARTESIAN_POINT('Ctrl Pts',(-37.9161246770386,-11.0187415076311,
-29.468841193656));
#26914=CARTESIAN_POINT('Ctrl Pts',(-37.9347738006665,-11.0223262068999,
-29.4551060632967));
#26915=CARTESIAN_POINT('Ctrl Pts',(-37.9525585139756,-11.0257447508523,
-29.4420075734922));
#26916=CARTESIAN_POINT('Ctrl Pts',(-37.9700990191786,-11.0307535195289,
-29.4290449639884));
#26917=CARTESIAN_POINT('Ctrl Pts',(-37.9871678607578,-11.0373176231361,
-29.4163864282423));
#26918=CARTESIAN_POINT('Ctrl Pts',(-38.0016526834004,-11.0428879997851,
-29.4056442437568));
#26919=CARTESIAN_POINT('Ctrl Pts',(-38.0158017303236,-11.0495814926574,
-29.3951108985677));
#26920=CARTESIAN_POINT('Ctrl Pts',(-38.0294827462888,-11.0574216164515,
-29.3848835313139));
#26921=CARTESIAN_POINT('Ctrl Pts',(-38.0323151592383,-11.0590447757414,
-29.3827661353894));
#26922=CARTESIAN_POINT('Ctrl Pts',(-38.035127405604,-11.0607171987449,-29.380661935915));
#26923=CARTESIAN_POINT('Ctrl Pts',(-38.0379181304706,-11.0624392724587,
-29.3785719346032));
#26924=CARTESIAN_POINT('Ctrl Pts',(-38.0505386215989,-11.0702270039859,
-29.369120324618));
#26925=CARTESIAN_POINT('Ctrl Pts',(-38.0627212545858,-11.0790298901558,
-29.3599545277751));
#26926=CARTESIAN_POINT('Ctrl Pts',(-38.0743506094951,-11.0888942095793,
-29.3511988246088));
#26927=CARTESIAN_POINT('Ctrl Pts',(-38.0777138589611,-11.0917470047078,
-29.3486666451176));
#26928=CARTESIAN_POINT('Ctrl Pts',(-38.0810305830642,-11.0946887229259,
-29.3461689091715));
#26929=CARTESIAN_POINT('Ctrl Pts',(-38.0842973331891,-11.0977208509785,
-29.3437090106853));
#26930=CARTESIAN_POINT('Ctrl Pts',(-38.0868926890118,-11.1001298051059,
-29.3417546794339));
#26931=CARTESIAN_POINT('Ctrl Pts',(-38.0894544429346,-11.1025951245287,
-29.3398243956254));
#26932=CARTESIAN_POINT('Ctrl Pts',(-38.0919798954887,-11.1051169477604,
-29.3379202081949));
#26933=CARTESIAN_POINT('Ctrl Pts',(-38.1045664389756,-11.117685403153,-29.3284299733211));
#26934=CARTESIAN_POINT('Ctrl Pts',(-38.1162463847602,-11.1317057213303,
-29.3196014738052));
#26935=CARTESIAN_POINT('Ctrl Pts',(-38.1267717929096,-11.1469740767481,
-29.3116302992635));
#26936=CARTESIAN_POINT('Ctrl Pts',(-38.1376151029358,-11.1627035866192,
-29.3034183690845));
#26937=CARTESIAN_POINT('Ctrl Pts',(-38.1472329395675,-11.1797576681432,
-29.296116441489));
#26938=CARTESIAN_POINT('Ctrl Pts',(-38.155340711547,-11.1978608317538,-29.2899503483155));
#26939=CARTESIAN_POINT('Ctrl Pts',(-38.1636385340936,-11.2163883433257,
-29.2836397185779));
#26940=CARTESIAN_POINT('Ctrl Pts',(-38.1703544452564,-11.2360145397413,
-29.2785189731724));
#26941=CARTESIAN_POINT('Ctrl Pts',(-38.1751722595047,-11.2563909917677,
-29.2748403601573));
#26942=CARTESIAN_POINT('Ctrl Pts',(-38.1801949750669,-11.2776340529195,
-29.2710052959796));
#26943=CARTESIAN_POINT('Ctrl Pts',(-38.1831544089492,-11.2996924044415,
-29.268737876305));
#26944=CARTESIAN_POINT('Ctrl Pts',(-38.1836843650225,-11.3221161967233,
-29.2683316856799));
#26945=CARTESIAN_POINT('Ctrl Pts',(-38.1837416869597,-11.3245416339992,
-29.2682877506545));
#26946=CARTESIAN_POINT('Ctrl Pts',(-38.1837705810015,-11.3269712973028,
-29.2682655958051));
#26947=CARTESIAN_POINT('Ctrl Pts',(-38.1837705810015,-11.3294045823054,
-29.2682655958051));
#26948=CARTESIAN_POINT('Ctrl Pts',(38.6963701433757,-11.3806731536973,29.3269198996342));
#26949=CARTESIAN_POINT('Ctrl Pts',(38.5618177595307,-11.3615458683564,29.5045706843909));
#26950=CARTESIAN_POINT('Ctrl Pts',(38.3497262416573,-11.3550383295792,29.4339522003598));
#26951=CARTESIAN_POINT('Ctrl Pts',(38.706929772342,-11.1940655928605,29.3129266693747));
#26952=CARTESIAN_POINT('Ctrl Pts',(38.5701244778425,-11.2445867749092,29.4937245996208));
#26953=CARTESIAN_POINT('Ctrl Pts',(38.3576357632337,-11.2617365126274,29.4278794464172));
#26954=CARTESIAN_POINT('Ctrl Pts',(38.6587619695313,-11.0057469829272,29.3768242824327));
#26955=CARTESIAN_POINT('Ctrl Pts',(38.5312471098703,-11.1260887992138,29.5445145967177));
#26956=CARTESIAN_POINT('Ctrl Pts',(38.3215665264224,-11.1675791668517,29.4556168052334));
#26957=CARTESIAN_POINT('Ctrl Pts',(38.4922459235859,-10.755919902964,29.5948104682567));
#26958=CARTESIAN_POINT('Ctrl Pts',(38.4133590232755,-10.9974050091189,29.6972789722255));
#26959=CARTESIAN_POINT('Ctrl Pts',(38.1964443230947,-11.0426657521647,29.5499206069573));
#26960=CARTESIAN_POINT('Ctrl Pts',(38.374138394728,-10.6922226875528,29.7482085696384));
#26961=CARTESIAN_POINT('Ctrl Pts',(38.3324029890132,-10.989329898887,29.8015013235227));
#26962=CARTESIAN_POINT('Ctrl Pts',(38.1075385459645,-11.0108152118554,29.6161302248789));
#26963=CARTESIAN_POINT('Ctrl Pts',(38.2605248298428,-10.7063374044318,29.8936321146768));
#26964=CARTESIAN_POINT('Ctrl Pts',(38.2746985341136,-11.0262754940985,29.8754832605275));
#26965=CARTESIAN_POINT('Ctrl Pts',(38.0216496713564,-11.0178704045121,29.6786922008474));
#26966=CARTESIAN_POINT('Origin',(38.0453209837941,-10.7044045823054,29.6614410681217));
#26967=CARTESIAN_POINT('Origin',(-35.8042963200226,-12.8919045823054,33.0767747666364));
#26968=CARTESIAN_POINT('Origin',(-35.8042963200226,-12.8919045823054,33.0767747666364));
#26969=CARTESIAN_POINT('Origin',(-36.9176881394302,-13.5169045823054,41.4426433113705));
#26970=CARTESIAN_POINT('Origin',(-36.9176881394301,-13.5169045823054,41.4426433113705));
#26971=CARTESIAN_POINT('Origin',(-10.0425103622231,-11.0169045823054,-19.6596180593406));
#26972=CARTESIAN_POINT('Origin',(-10.0425103622231,-11.3294045823054,-19.6596180593406));
#26973=CARTESIAN_POINT('Origin',(5.15768816523998,-11.3294045823054,-15.3054474424773));
#26974=CARTESIAN_POINT('Origin',(-9.84678298317079,-11.3294045823054,-20.2531800132168));
#26975=CARTESIAN_POINT('Origin',(0.0835265683620477,-10.7044045823054,0.0824317919394229));
#26976=CARTESIAN_POINT('Origin',(34.1908936222416,-10.7044045823054,34.0339139046828));
#26977=CARTESIAN_POINT('Origin',(33.692255281224,-14.7669045823054,34.5275908031162));
#26978=CARTESIAN_POINT('Origin',(33.692255281224,-11.3294045823054,34.5275908031162));
#26979=CARTESIAN_POINT('Origin',(33.692255281224,-12.8919045823054,34.5275908031162));
#26980=CARTESIAN_POINT('Origin',(-6.86479538799601,-13.5169045823054,21.1538811545436));
#26981=CARTESIAN_POINT('Origin',(34.3599945679822,-13.5169045823054,34.7477781982718));
#26982=CARTESIAN_POINT('Origin',(41.4437380877936,-13.5169045823054,37.0836464997312));
#26983=CARTESIAN_POINT('Ctrl Pts',(34.4578582575083,-13.5169045823054,34.4509972213337));
#26984=CARTESIAN_POINT('Ctrl Pts',(34.4578582575083,-13.2044045823054,34.4509972213337));
#26985=CARTESIAN_POINT('Ctrl Pts',(34.3599945679822,-13.2044045823054,34.7477781982718));
#26986=CARTESIAN_POINT('Ctrl Pts',(34.3745296971238,-13.5169045582439,34.4235195829545));
#26987=CARTESIAN_POINT('Ctrl Pts',(34.4061312136231,-13.1861191316369,34.43394020031));
#26988=CARTESIAN_POINT('Ctrl Pts',(34.3041321680135,-13.2044045823054,34.7480782775218));
#26989=CARTESIAN_POINT('Ctrl Pts',(34.2933711160147,-13.5027466839947,34.3967574964286));
#26990=CARTESIAN_POINT('Ctrl Pts',(34.3629706115748,-13.1578432798925,34.4197079681703));
#26991=CARTESIAN_POINT('Ctrl Pts',(34.2496387413663,-13.1973256316196,34.7484206608821));
#26992=CARTESIAN_POINT('Ctrl Pts',(34.1358739983332,-13.4449866817213,34.3448227357001));
#26993=CARTESIAN_POINT('Ctrl Pts',(34.2950839932164,-13.0892356355758,34.397322318623));
#26994=CARTESIAN_POINT('Ctrl Pts',(34.1437376255259,-13.1684456335483,34.7491725375223));
#26995=CARTESIAN_POINT('Ctrl Pts',(34.064061118804,-13.4031153721667,34.3211423993836));
#26996=CARTESIAN_POINT('Ctrl Pts',(34.2738703798607,-13.0503322093643,34.390327118012));
#26997=CARTESIAN_POINT('Ctrl Pts',(34.0953731108843,-13.1475099673761,34.7495603170485));
#26998=CARTESIAN_POINT('Ctrl Pts',(33.9360538509793,-13.2902331116008,34.2789319327805));
#26999=CARTESIAN_POINT('Ctrl Pts',(34.253604081193,-12.9767617731724,34.3836442949382));
#27000=CARTESIAN_POINT('Ctrl Pts',(34.0090703956612,-13.0910688568131,34.750304648432));
#27001=CARTESIAN_POINT('Ctrl Pts',(33.8839249013386,-13.222452827101,34.2617423831146));
#27002=CARTESIAN_POINT('Ctrl Pts',(34.2570256950654,-12.9460615526393,34.3847725739844));
#27003=CARTESIAN_POINT('Ctrl Pts',(33.9738736850488,-13.0571787063092,34.7506372725395));
#27004=CARTESIAN_POINT('Ctrl Pts',(33.8098868212263,-13.0654169357612,34.2373282856884));
#27005=CARTESIAN_POINT('Ctrl Pts',(34.2704028238453,-12.9052920386068,34.389183689519));
#27006=CARTESIAN_POINT('Ctrl Pts',(33.9238607907023,-12.9786607574272,34.7511230809577));
#27007=CARTESIAN_POINT('Ctrl Pts',(33.7901189534223,-12.9802875861308,34.2308098204642));
#27008=CARTESIAN_POINT('Ctrl Pts',(34.2787581405614,-12.8977806170664,34.3919388597773));
#27009=CARTESIAN_POINT('Ctrl Pts',(33.9104937733009,-12.9360960854268,34.7512606727365));
#27010=CARTESIAN_POINT('Ctrl Pts',(33.7901189707501,-12.8919045823054,34.2308098261781));
#27011=CARTESIAN_POINT('Ctrl Pts',(34.2787581354395,-12.8919045823054,34.3919388580886));
#27012=CARTESIAN_POINT('Ctrl Pts',(33.9104937793594,-12.8919045823054,34.7512606668251));
#27013=CARTESIAN_POINT('Ctrl Pts',(33.9104937793594,-12.8919045823054,34.7512606668251));
#27014=CARTESIAN_POINT('Ctrl Pts',(33.9104937793594,-12.9051774018388,34.7512606668251));
#27015=CARTESIAN_POINT('Ctrl Pts',(33.9117040823358,-12.9183340038153,34.7512482101544));
#27016=CARTESIAN_POINT('Ctrl Pts',(33.9140678651876,-12.9312552225994,34.7512241292996));
#27017=CARTESIAN_POINT('Ctrl Pts',(33.9164761535976,-12.9444197234828,34.7511995950479));
#27018=CARTESIAN_POINT('Ctrl Pts',(33.9200814988752,-12.9573395068935,34.7511630014824));
#27019=CARTESIAN_POINT('Ctrl Pts',(33.9247701430341,-12.9698996728684,34.7511157321652));
#27020=CARTESIAN_POINT('Ctrl Pts',(33.9296145840165,-12.9828771948836,34.7510668921574));
#27021=CARTESIAN_POINT('Ctrl Pts',(33.9356152049093,-12.9954703520459,34.7510066623665));
#27022=CARTESIAN_POINT('Ctrl Pts',(33.9425940244808,-13.0075707507672,34.7509369943112));
#27023=CARTESIAN_POINT('Ctrl Pts',(33.9446073176688,-13.0110615488982,34.7509168960382));
#27024=CARTESIAN_POINT('Ctrl Pts',(33.9467017142206,-13.0145114746282,34.7508960145068));
#27025=CARTESIAN_POINT('Ctrl Pts',(33.9488722314559,-13.0179182754031,34.7508744014892));
#27026=CARTESIAN_POINT('Ctrl Pts',(33.9522032468625,-13.0231465710756,34.7508412327616));
#27027=CARTESIAN_POINT('Ctrl Pts',(33.9556878747932,-13.0282366579925,34.7508066183155));
#27028=CARTESIAN_POINT('Ctrl Pts',(33.9593070766984,-13.0331862397833,34.7507707786108));
#27029=CARTESIAN_POINT('Ctrl Pts',(33.9667645107392,-13.0433849467635,34.7506969302207));
#27030=CARTESIAN_POINT('Ctrl Pts',(33.9748160481855,-13.0530328316013,34.7506263796451));
#27031=CARTESIAN_POINT('Ctrl Pts',(33.9833730071236,-13.0621635675362,34.7505475422118));
#27032=CARTESIAN_POINT('Ctrl Pts',(33.9928680087852,-13.0722952455658,34.7504600623531));
#27033=CARTESIAN_POINT('Ctrl Pts',(34.0029431003418,-13.0817557997662,34.7503681518668));
#27034=CARTESIAN_POINT('Ctrl Pts',(34.0135255597351,-13.0906427434663,34.7502724193904));
#27035=CARTESIAN_POINT('Ctrl Pts',(34.0246022815835,-13.099944759169,34.75017221565));
#27036=CARTESIAN_POINT('Ctrl Pts',(34.0362351994585,-13.1086184489897,34.7500678136454));
#27037=CARTESIAN_POINT('Ctrl Pts',(34.0483916685675,-13.1167513951577,34.7499593789485));
#27038=CARTESIAN_POINT('Ctrl Pts',(34.0496640078893,-13.1176026182488,34.7499480297872));
#27039=CARTESIAN_POINT('Ctrl Pts',(34.0509421236522,-13.1184478958543,34.7499366360809));
#27040=CARTESIAN_POINT('Ctrl Pts',(34.0522260065119,-13.119287313057,34.7499251977801));
#27041=CARTESIAN_POINT('Ctrl Pts',(34.0586407621694,-13.1234813531983,34.7498680477804));
#27042=CARTESIAN_POINT('Ctrl Pts',(34.0651387821861,-13.1274936111504,34.7498103139349));
#27043=CARTESIAN_POINT('Ctrl Pts',(34.0717272061634,-13.1313379140666,34.7497518934144));
#27044=CARTESIAN_POINT('Ctrl Pts',(34.0912832509352,-13.1427487401161,34.7495784871006));
#27045=CARTESIAN_POINT('Ctrl Pts',(34.1115096164517,-13.1526155242428,34.7494099515472));
#27046=CARTESIAN_POINT('Ctrl Pts',(34.1323508455064,-13.1611451738774,34.7492466433572));
#27047=CARTESIAN_POINT('Ctrl Pts',(34.1531920745612,-13.1696748235119,34.7490833351672));
#27048=CARTESIAN_POINT('Ctrl Pts',(34.1746485137788,-13.1768668275904,34.7489252300396));
#27049=CARTESIAN_POINT('Ctrl Pts',(34.1966978194881,-13.1828814286543,34.7487720524465));
#27050=CARTESIAN_POINT('Ctrl Pts',(34.2203748666754,-13.1893400444075,34.7486075668547));
#27051=CARTESIAN_POINT('Ctrl Pts',(34.2441289381238,-13.19426816731,34.7484530498353));
#27052=CARTESIAN_POINT('Ctrl Pts',(34.268032456907,-13.1977771930991,34.7483060606209));
#27053=CARTESIAN_POINT('Ctrl Pts',(34.2923821257301,-13.201351713513,34.7481563279091));
#27054=CARTESIAN_POINT('Ctrl Pts',(34.3168869206479,-13.2034535833856,34.7480143798219));
#27055=CARTESIAN_POINT('Ctrl Pts',(34.3416346865736,-13.2041479208638,34.7478780637107));
#27056=CARTESIAN_POINT('Ctrl Pts',(34.3477393394683,-13.2043191964977,34.7478444379465));
#27057=CARTESIAN_POINT('Ctrl Pts',(34.3538588277594,-13.2044045823054,34.74781115797));
#27058=CARTESIAN_POINT('Ctrl Pts',(34.3599945679822,-13.2044045823054,34.7477781982718));
#27059=CARTESIAN_POINT('Origin',(0.0835265683620477,-12.8919045823054,0.0824317919394229));
#27060=CARTESIAN_POINT('Ctrl Pts',(-34.5818198379706,-13.2044045823054,
34.3588997915592));
#27061=CARTESIAN_POINT('Ctrl Pts',(-34.5819536007302,-13.2044045823054,
34.3339986672398));
#27062=CARTESIAN_POINT('Ctrl Pts',(-34.5820925794552,-13.2030022087212,
34.3093644005129));
#27063=CARTESIAN_POINT('Ctrl Pts',(-34.5822388280734,-13.2001447338013,
34.2849062065081));
#27064=CARTESIAN_POINT('Ctrl Pts',(-34.5823824111376,-13.1973393397405,
34.2608937920094));
#27065=CARTESIAN_POINT('Ctrl Pts',(-34.5825330278843,-13.1931314656529,
34.2370510471072));
#27066=CARTESIAN_POINT('Ctrl Pts',(-34.5826931179797,-13.1874220362842,
34.2133024907471));
#27067=CARTESIAN_POINT('Ctrl Pts',(-34.5827329267351,-13.1860023027453,
34.207397063114));
#27068=CARTESIAN_POINT('Ctrl Pts',(-34.5827733226246,-13.1844894768729,
34.2014975126608));
#27069=CARTESIAN_POINT('Ctrl Pts',(-34.5828143450745,-13.1828815404475,
34.1956027867627));
#27070=CARTESIAN_POINT('Ctrl Pts',(-34.582967790943,-13.1768669995857,34.1735533641464));
#27071=CARTESIAN_POINT('Ctrl Pts',(-34.5831262740765,-13.1696750914266,
34.1520967504123));
#27072=CARTESIAN_POINT('Ctrl Pts',(-34.5832901051238,-13.1611455958502,
34.1312552352812));
#27073=CARTESIAN_POINT('Ctrl Pts',(-34.5834539361711,-13.1526161002738,
34.11041372015));
#27074=CARTESIAN_POINT('Ctrl Pts',(-34.5836231397398,-13.1427495299604,
34.0901869574092));
#27075=CARTESIAN_POINT('Ctrl Pts',(-34.5837973809619,-13.1313389816383,
34.0706303230888));
#27076=CARTESIAN_POINT('Ctrl Pts',(-34.5838561693646,-13.1274891009823,
34.0640319803939));
#27077=CARTESIAN_POINT('Ctrl Pts',(-34.5839137704652,-13.1234784566375,
34.0575374938193));
#27078=CARTESIAN_POINT('Ctrl Pts',(-34.5839705894707,-13.1192883941035,
34.0511290395554));
#27079=CARTESIAN_POINT('Ctrl Pts',(-34.5840653300571,-13.1123018412983,
34.0404435178594));
#27080=CARTESIAN_POINT('Ctrl Pts',(-34.5841564572897,-13.1049166125572,
34.0301624181513));
#27081=CARTESIAN_POINT('Ctrl Pts',(-34.5842452183515,-13.097044387883,34.0202632237194));
#27082=CARTESIAN_POINT('Ctrl Pts',(-34.5842782571648,-13.0941141732637,
34.0165785265156));
#27083=CARTESIAN_POINT('Ctrl Pts',(-34.5843109641004,-13.0911162306685,
34.0129471746141));
#27084=CARTESIAN_POINT('Ctrl Pts',(-34.5843433867853,-13.088045086031,34.009369649718));
#27085=CARTESIAN_POINT('Ctrl Pts',(-34.5844292711082,-13.0799099430592,
33.9998931580673));
#27086=CARTESIAN_POINT('Ctrl Pts',(-34.5845127940359,-13.0712950250751,
33.9908333807281));
#27087=CARTESIAN_POINT('Ctrl Pts',(-34.5845904021225,-13.0621639241565,
33.9822773142586));
#27088=CARTESIAN_POINT('Ctrl Pts',(-34.5846680102091,-13.053032823238,33.973721247789));
#27089=CARTESIAN_POINT('Ctrl Pts',(-34.5847385699196,-13.0433849467635,
33.9656697343162));
#27090=CARTESIAN_POINT('Ctrl Pts',(-34.5848124183096,-13.0331862397832,
33.9582123002755));
#27091=CARTESIAN_POINT('Ctrl Pts',(-34.5848482580143,-13.0282366579925,
33.9545930983703));
#27092=CARTESIAN_POINT('Ctrl Pts',(-34.5848828724605,-13.0231465710756,
33.9511084704396));
#27093=CARTESIAN_POINT('Ctrl Pts',(-34.5849160411879,-13.0179182754031,
33.9477774550331));
#27094=CARTESIAN_POINT('Ctrl Pts',(-34.5849905800164,-13.0061689239906,
33.9402917899096));
#27095=CARTESIAN_POINT('Ctrl Pts',(-34.5850563954841,-12.9939049176357,
33.933714890177));
#27096=CARTESIAN_POINT('Ctrl Pts',(-34.5851114686253,-12.981226713366,33.9282355973367));
#27097=CARTESIAN_POINT('Ctrl Pts',(-34.5851652658616,-12.9688422309119,
33.922883245805));
#27098=CARTESIAN_POINT('Ctrl Pts',(-34.5852088052819,-12.9560629035317,
33.9185786270626));
#27099=CARTESIAN_POINT('Ctrl Pts',(-34.5852405562661,-12.9430006092193,
33.9154520648799));
#27100=CARTESIAN_POINT('Ctrl Pts',(-34.5852714506247,-12.9302907290071,
33.912409855765));
#27101=CARTESIAN_POINT('Ctrl Pts',(-34.585291178121,-12.9173133257082,33.9104832101191));
#27102=CARTESIAN_POINT('Ctrl Pts',(-34.585298762369,-12.9041833323897,33.9097440507805));
#27103=CARTESIAN_POINT('Ctrl Pts',(-34.585301118774,-12.9001038795348,33.9095143960046));
#27104=CARTESIAN_POINT('Ctrl Pts',(-34.585302306524,-12.8960097626081,33.9093990029364));
#27105=CARTESIAN_POINT('Ctrl Pts',(-34.585302306524,-12.8919045823054,33.9093990029364));
#27106=CARTESIAN_POINT('Origin',(-20.9879227942421,-13.5169045823054,-6.86589016441886));
#27107=CARTESIAN_POINT('Origin',(-34.5818198379706,-13.5169045823054,34.3588997915592));
#27108=CARTESIAN_POINT('Origin',(-10.0425103622231,-11.3294045823054,-19.6596180593406));
#27109=CARTESIAN_POINT('Origin',(-9.75726988530523,-11.3294045823054,-19.1035039790228));
#27110=CARTESIAN_POINT('Ctrl Pts',(34.4123700316823,-10.7044045823054,34.2543780742461));
#27111=CARTESIAN_POINT('Ctrl Pts',(34.4123700316823,-11.0169045823054,34.2543780742461));
#27112=CARTESIAN_POINT('Ctrl Pts',(34.1908936222416,-11.0169045823054,34.0339139046828));
#27113=CARTESIAN_POINT('Ctrl Pts',(34.3501592468467,-10.7044046073823,34.3168744938738));
#27114=CARTESIAN_POINT('Ctrl Pts',(34.3738055566337,-11.034944931328,34.2931196129008));
#27115=CARTESIAN_POINT('Ctrl Pts',(34.1413487873541,-11.0169045823054,34.058813837913));
#27116=CARTESIAN_POINT('Ctrl Pts',(34.2893549490476,-10.718650676671,34.3776158502248));
#27117=CARTESIAN_POINT('Ctrl Pts',(34.3414414505694,-11.0630714156275,34.3255569415899));
#27118=CARTESIAN_POINT('Ctrl Pts',(34.0928733345355,-11.0240276257398,34.0829643022232));
#27119=CARTESIAN_POINT('Ctrl Pts',(34.1711981326456,-10.7765752156551,34.4950601734815));
#27120=CARTESIAN_POINT('Ctrl Pts',(34.2904881406856,-11.1314870357709,34.376795148033));
#27121=CARTESIAN_POINT('Ctrl Pts',(33.9985873189392,-11.0529899027286,34.1295721958079));
#27122=CARTESIAN_POINT('Ctrl Pts',(34.1171495610117,-10.8185639645426,34.5484801321362));
#27123=CARTESIAN_POINT('Ctrl Pts',(34.2744792581431,-11.1704305366374,34.3930297458242));
#27124=CARTESIAN_POINT('Ctrl Pts',(33.9554132623581,-11.0739842709862,34.1507269685016));
#27125=CARTESIAN_POINT('Ctrl Pts',(34.0207493920589,-10.9314866347397,34.6434052910951));
#27126=CARTESIAN_POINT('Ctrl Pts',(34.2592746271241,-11.2441510617714,34.4090931206949));
#27127=CARTESIAN_POINT('Ctrl Pts',(33.8783564349675,-11.1304456109604,34.188265264605));
#27128=CARTESIAN_POINT('Ctrl Pts',(33.981374129179,-10.9992937157271,34.68198187454));
#27129=CARTESIAN_POINT('Ctrl Pts',(34.2619434427441,-11.2750326114056,34.4070617919781));
#27130=CARTESIAN_POINT('Ctrl Pts',(33.8468530908865,-11.1643491474262,34.2034909999848));
#27131=CARTESIAN_POINT('Ctrl Pts',(33.9254685896631,-11.1560957480194,34.736665233204));
#27132=CARTESIAN_POINT('Ctrl Pts',(34.2723025800306,-11.3160025899709,34.3979203004132));
#27133=CARTESIAN_POINT('Ctrl Pts',(33.802111185478,-11.2427501667525,34.2250605800652));
#27134=CARTESIAN_POINT('Ctrl Pts',(33.9104937666812,-11.2411599901508,34.7512606791955));
#27135=CARTESIAN_POINT('Ctrl Pts',(34.2787581392411,-11.3235538600011,34.3919388546111));
#27136=CARTESIAN_POINT('Ctrl Pts',(33.7901189630482,-11.2852822850309,34.2308098236384));
#27137=CARTESIAN_POINT('Ctrl Pts',(33.9104937793594,-11.3294045823054,34.7512606668251));
#27138=CARTESIAN_POINT('Ctrl Pts',(34.2787581354396,-11.3294045823054,34.3919388580886));
#27139=CARTESIAN_POINT('Ctrl Pts',(33.7901189707501,-11.3294045823054,34.2308098261781));
#27140=CARTESIAN_POINT('Ctrl Pts',(33.7901189707501,-11.3294045823054,34.2308098261781));
#27141=CARTESIAN_POINT('Ctrl Pts',(33.7901189707501,-11.3159760597524,34.2308098261781));
#27142=CARTESIAN_POINT('Ctrl Pts',(33.7912338216707,-11.3026664608401,34.2302753470968));
#27143=CARTESIAN_POINT('Ctrl Pts',(33.7934081164331,-11.2895978753989,34.2292314243157));
#27144=CARTESIAN_POINT('Ctrl Pts',(33.79562435048,-11.2762772141433,34.228167365638));
#27145=CARTESIAN_POINT('Ctrl Pts',(33.7989410334812,-11.2632073639008,34.2265741308302));
#27146=CARTESIAN_POINT('Ctrl Pts',(33.8032512127749,-11.250506246618,34.2245015446458));
#27147=CARTESIAN_POINT('Ctrl Pts',(33.8077029487296,-11.2373879940767,34.2223608897432));
#27148=CARTESIAN_POINT('Ctrl Pts',(33.8132142064821,-11.2246635682845,34.2197090098756));
#27149=CARTESIAN_POINT('Ctrl Pts',(33.8196203282791,-11.212443933042,34.2166236619276));
#27150=CARTESIAN_POINT('Ctrl Pts',(33.8211904549206,-11.2094489267884,34.2158674497973));
#27151=CARTESIAN_POINT('Ctrl Pts',(33.8228141381246,-11.2064841392023,34.2150852966479));
#27152=CARTESIAN_POINT('Ctrl Pts',(33.8244885802811,-11.2035509891888,34.2142785315667));
#27153=CARTESIAN_POINT('Ctrl Pts',(33.8274036314582,-11.1984446423577,34.2128740270931));
#27154=CARTESIAN_POINT('Ctrl Pts',(33.8304514090713,-11.1934675809199,34.2114049990652));
#27155=CARTESIAN_POINT('Ctrl Pts',(33.8336162487135,-11.18862206557,34.209878801354));
#27156=CARTESIAN_POINT('Ctrl Pts',(33.8402728914365,-11.1784304387767,34.206668732587));
#27157=CARTESIAN_POINT('Ctrl Pts',(33.8474541808265,-11.1687879968701,34.2031919007031));
#27158=CARTESIAN_POINT('Ctrl Pts',(33.8550888482703,-11.1596600078883,34.1994978425559));
#27159=CARTESIAN_POINT('Ctrl Pts',(33.8635475329149,-11.1495468260368,34.1954050810629));
#27160=CARTESIAN_POINT('Ctrl Pts',(33.8725221968181,-11.1400969285544,34.1910570289537));
#27161=CARTESIAN_POINT('Ctrl Pts',(33.8819480720297,-11.1312146907196,34.1864836245605));
#27162=CARTESIAN_POINT('Ctrl Pts',(33.8918181729339,-11.1219138479102,34.1816946832872));
#27163=CARTESIAN_POINT('Ctrl Pts',(33.9021833303367,-11.1132352948843,34.1766585236442));
#27164=CARTESIAN_POINT('Ctrl Pts',(33.913015050167,-11.1050933657985,34.1713874544776));
#27165=CARTESIAN_POINT('Ctrl Pts',(33.9143006425789,-11.1041270185873,34.1707618431592));
#27166=CARTESIAN_POINT('Ctrl Pts',(33.9155928549205,-11.1031682588508,34.1701328995634));
#27167=CARTESIAN_POINT('Ctrl Pts',(33.916891676798,-11.1022169660873,34.1695006260756));
#27168=CARTESIAN_POINT('Ctrl Pts',(33.9224967875947,-11.0981116292185,34.1667720279404));
#27169=CARTESIAN_POINT('Ctrl Pts',(33.9281745502422,-11.0941782436166,34.1640059611718));
#27170=CARTESIAN_POINT('Ctrl Pts',(33.9339309727463,-11.0904041712721,34.1611993802633));
#27171=CARTESIAN_POINT('Ctrl Pts',(33.9514412782026,-11.0789239229899,34.152662117934));
#27172=CARTESIAN_POINT('Ctrl Pts',(33.969549527539,-11.0689908784592,34.1438027788335));
#27173=CARTESIAN_POINT('Ctrl Pts',(33.9881992711126,-11.0604019317832,34.1346450450658));
#27174=CARTESIAN_POINT('Ctrl Pts',(34.0068490146862,-11.0518129851073,34.1254873112982));
#27175=CARTESIAN_POINT('Ctrl Pts',(34.0260406250709,-11.0445686309469,34.1160310511287));
#27176=CARTESIAN_POINT('Ctrl Pts',(34.045749017185,-11.0385127393807,34.1062850795439));
#27177=CARTESIAN_POINT('Ctrl Pts',(34.0667664671036,-11.0320546073846,34.0958917674714));
#27178=CARTESIAN_POINT('Ctrl Pts',(34.0878492419839,-11.0271158190915,34.0854271901211));
#27179=CARTESIAN_POINT('Ctrl Pts',(34.1090552865085,-11.0235921824189,34.0748636859948));
#27180=CARTESIAN_POINT('Ctrl Pts',(34.1306266089857,-11.0200078504674,34.0641182235992));
#27181=CARTESIAN_POINT('Ctrl Pts',(34.1523255949182,-11.0178879088435,34.0532703834115));
#27182=CARTESIAN_POINT('Ctrl Pts',(34.1742231261325,-11.0171750715253,34.0422846764148));
#27183=CARTESIAN_POINT('Ctrl Pts',(34.1797667772391,-11.0169946072826,34.0395034986577));
#27184=CARTESIAN_POINT('Ctrl Pts',(34.1853231974622,-11.0169045823054,34.0367134539662));
#27185=CARTESIAN_POINT('Ctrl Pts',(34.1908936222416,-11.0169045823054,34.0339139046828));
#27186=CARTESIAN_POINT('Origin',(41.4437380877936,-13.5169045823054,37.0836464997312));
#27187=CARTESIAN_POINT('Origin',(41.4437380877936,-13.5169045823054,37.0836464997312));
#27188=CARTESIAN_POINT('Origin',(41.4437380877936,-13.5169045823054,37.0836464997312));
#27189=CARTESIAN_POINT('Origin',(0.0835265683620477,-13.5169045823054,0.0824317919394229));
#27190=CARTESIAN_POINT('Origin',(40.2796596827637,-13.5169045823054,38.3450489192809));
#27191=CARTESIAN_POINT('Origin',(-7.35411383562686,-12.8919045823054,22.6377860392341));
#27192=CARTESIAN_POINT('Origin',(33.0778695430594,-12.8919045823054,35.9702546803237));
#27193=CARTESIAN_POINT('Ctrl Pts',(39.2345740945198,-12.8919045823054,38.3294829568536));
#27194=CARTESIAN_POINT('Ctrl Pts',(39.264809323272,-12.9061660297064,38.3394530400775));
#27195=CARTESIAN_POINT('Ctrl Pts',(39.2954516743711,-12.920086395132,38.3485334458199));
#27196=CARTESIAN_POINT('Ctrl Pts',(39.3264280099796,-12.9336529684133,38.3568222284112));
#27197=CARTESIAN_POINT('Ctrl Pts',(39.3601265408272,-12.9484117699059,38.3658394278429));
#27198=CARTESIAN_POINT('Ctrl Pts',(39.3942201310872,-12.9627531581661,38.3739203780609));
#27199=CARTESIAN_POINT('Ctrl Pts',(39.4286337339504,-12.9766849821654,38.3811333480185));
#27200=CARTESIAN_POINT('Ctrl Pts',(39.4624584084797,-12.9903783874809,38.3882228806715));
#27201=CARTESIAN_POINT('Ctrl Pts',(39.4965924126089,-13.0036776000038,38.3944733524844));
#27202=CARTESIAN_POINT('Ctrl Pts',(39.5309818914864,-13.0165906742131,38.399896805926));
#27203=CARTESIAN_POINT('Ctrl Pts',(39.5662695137509,-13.0298409966909,38.4054619026551));
#27204=CARTESIAN_POINT('Ctrl Pts',(39.6018262535649,-13.0426862586666,38.4101558421804));
#27205=CARTESIAN_POINT('Ctrl Pts',(39.6376103185495,-13.0551132414191,38.4139419214656));
#27206=CARTESIAN_POINT('Ctrl Pts',(39.6715407016172,-13.0668964830757,38.4175318747179));
#27207=CARTESIAN_POINT('Ctrl Pts',(39.7056757961189,-13.0783045133849,38.4203045946093));
#27208=CARTESIAN_POINT('Ctrl Pts',(39.7399908862156,-13.0892900686274,38.4221956986995));
#27209=CARTESIAN_POINT('Ctrl Pts',(39.7418655854155,-13.0898902305843,38.4222990133437));
#27210=CARTESIAN_POINT('Ctrl Pts',(39.7437408239533,-13.0904891204199,38.4223996902635));
#27211=CARTESIAN_POINT('Ctrl Pts',(39.745616598492,-13.0910867263844,38.4224977168591));
#27212=CARTESIAN_POINT('Ctrl Pts',(39.7728375717412,-13.0997590991245,38.4239202648684));
#27213=CARTESIAN_POINT('Ctrl Pts',(39.8001748601324,-13.1081389493477,38.4248104957089));
#27214=CARTESIAN_POINT('Ctrl Pts',(39.8276166222947,-13.1162261892174,38.4250795370517));
#27215=CARTESIAN_POINT('Ctrl Pts',(39.8542746788235,-13.1240824666798,38.4253408948786));
#27216=CARTESIAN_POINT('Ctrl Pts',(39.8810315488655,-13.1316631802151,38.4250153647531));
#27217=CARTESIAN_POINT('Ctrl Pts',(39.9078825960307,-13.1389242143529,38.4240026130721));
#27218=CARTESIAN_POINT('Ctrl Pts',(39.9334074955964,-13.1458266329428,38.4230398802303));
#27219=CARTESIAN_POINT('Ctrl Pts',(39.9590177371494,-13.1524404698811,38.421455410863));
#27220=CARTESIAN_POINT('Ctrl Pts',(39.9847117520737,-13.1586815279054,38.4191556941318));
#27221=CARTESIAN_POINT('Ctrl Pts',(39.9944282810576,-13.1610416659127,38.4182860260656));
#27222=CARTESIAN_POINT('Ctrl Pts',(40.0041567975574,-13.1633479802309,38.4173140502073));
#27223=CARTESIAN_POINT('Ctrl Pts',(40.0138971970891,-13.1655939279677,38.4162347690805));
#27224=CARTESIAN_POINT('Ctrl Pts',(40.0336369972984,-13.1701455440958,38.414047508307));
#27225=CARTESIAN_POINT('Ctrl Pts',(40.0533462534983,-13.174435676212,38.4114272898243));
#27226=CARTESIAN_POINT('Ctrl Pts',(40.0730154951905,-13.1784305895997,38.4082506512823));
#27227=CARTESIAN_POINT('Ctrl Pts',(40.0916995992408,-13.1822254170047,38.4052331152746));
#27228=CARTESIAN_POINT('Ctrl Pts',(40.1103478051953,-13.1857540666263,38.4017128678585));
#27229=CARTESIAN_POINT('Ctrl Pts',(40.1289527638623,-13.1889407631081,38.397581753751));
#27230=CARTESIAN_POINT('Ctrl Pts',(40.1356516054506,-13.1900881547956,38.3960943180902));
#27231=CARTESIAN_POINT('Ctrl Pts',(40.1423448327474,-13.1911907417383,38.3945277124038));
#27232=CARTESIAN_POINT('Ctrl Pts',(40.1490320418338,-13.1922433006301,38.3928770728127));
#27233=CARTESIAN_POINT('Ctrl Pts',(40.1634532674053,-13.1945131846744,38.3893174045603));
#27234=CARTESIAN_POINT('Ctrl Pts',(40.1778289941368,-13.1965398886054,38.3854132586859));
#27235=CARTESIAN_POINT('Ctrl Pts',(40.1920769307064,-13.1982777342415,38.3810070154518));
#27236=CARTESIAN_POINT('Ctrl Pts',(40.2057841542068,-13.1999496281629,38.3767679903472));
#27237=CARTESIAN_POINT('Ctrl Pts',(40.2193732995346,-13.201354438406,38.3720636577237));
#27238=CARTESIAN_POINT('Ctrl Pts',(40.232769573981,-13.2024042504876,38.3667582778887));
#27239=CARTESIAN_POINT('Ctrl Pts',(40.2453986452936,-13.2033939399492,38.3617567365613));
#27240=CARTESIAN_POINT('Ctrl Pts',(40.2578565021756,-13.2040681761667,38.3562204211069));
#27241=CARTESIAN_POINT('Ctrl Pts',(40.270076341403,-13.204308494197,38.3500481542611));
#27242=CARTESIAN_POINT('Ctrl Pts',(40.2732876902366,-13.2043716492854,38.3484260951188));
#27243=CARTESIAN_POINT('Ctrl Pts',(40.276482568374,-13.2044045823054,38.3467602140877));
#27244=CARTESIAN_POINT('Ctrl Pts',(40.2796596827637,-13.2044045823054,38.3450489192809));
#27245=CARTESIAN_POINT('Origin',(0.0835265683620477,-12.8919045823054,0.0824317919394229));
#27246=CARTESIAN_POINT('Origin',(33.0778695430594,-12.8919045823054,35.9702546803237));
#27247=CARTESIAN_POINT('Ctrl Pts',(-34.2850388610326,-13.5169045823054,
34.4567634810853));
#27248=CARTESIAN_POINT('Ctrl Pts',(-34.2850388610326,-13.2044045823054,
34.4567634810853));
#27249=CARTESIAN_POINT('Ctrl Pts',(-34.5818198379706,-13.2044045823054,
34.3588997915592));
#27250=CARTESIAN_POINT('Ctrl Pts',(-34.2575612226533,-13.5169045582439,
34.3734349207008));
#27251=CARTESIAN_POINT('Ctrl Pts',(-34.2679818400087,-13.1861191316367,
34.4050364372002));
#27252=CARTESIAN_POINT('Ctrl Pts',(-34.5821199172207,-13.2044045823054,
34.3030373915905));
#27253=CARTESIAN_POINT('Ctrl Pts',(-34.2307991361275,-13.5027466839949,
34.2922763395917));
#27254=CARTESIAN_POINT('Ctrl Pts',(-34.2537496078692,-13.1578432798927,
34.3618758351519));
#27255=CARTESIAN_POINT('Ctrl Pts',(-34.582462300581,-13.1973256316196,34.2485439649434));
#27256=CARTESIAN_POINT('Ctrl Pts',(-34.178864375399,-13.4449866817212,34.1347792219102));
#27257=CARTESIAN_POINT('Ctrl Pts',(-34.2313639583219,-13.0892356355756,
34.2939892167934));
#27258=CARTESIAN_POINT('Ctrl Pts',(-34.5832141772212,-13.1684456335483,
34.1426428491029));
#27259=CARTESIAN_POINT('Ctrl Pts',(-34.1551840390824,-13.4031153721666,
34.0629663423807));
#27260=CARTESIAN_POINT('Ctrl Pts',(-34.2243687577112,-13.0503322093644,
34.2727756034371));
#27261=CARTESIAN_POINT('Ctrl Pts',(-34.5836019567474,-13.1475099673759,
34.0942783344611));
#27262=CARTESIAN_POINT('Ctrl Pts',(-34.1129735724795,-13.2902331116009,
33.9349590745566));
#27263=CARTESIAN_POINT('Ctrl Pts',(-34.2176859346367,-12.9767617731723,
34.2525093047707));
#27264=CARTESIAN_POINT('Ctrl Pts',(-34.5843462881308,-13.0910688568132,
34.0079756192384));
#27265=CARTESIAN_POINT('Ctrl Pts',(-34.0957840228135,-13.2224528271012,
33.8828301249157));
#27266=CARTESIAN_POINT('Ctrl Pts',(-34.2188142136836,-12.9460615526393,
34.255930918643));
#27267=CARTESIAN_POINT('Ctrl Pts',(-34.5846789122388,-13.0571787063095,
33.9727789086256));
#27268=CARTESIAN_POINT('Ctrl Pts',(-34.0713699253873,-13.0654169357609,
33.8087920448033));
#27269=CARTESIAN_POINT('Ctrl Pts',(-34.2232253292175,-12.9052920386068,
34.2693080474217));
#27270=CARTESIAN_POINT('Ctrl Pts',(-34.5851647206562,-12.9786607574269,
33.9227660142796));
#27271=CARTESIAN_POINT('Ctrl Pts',(-34.0648514601626,-12.9802875861309,
33.7890241769979));
#27272=CARTESIAN_POINT('Ctrl Pts',(-34.2259804994776,-12.8977806170664,
34.2776633641381));
#27273=CARTESIAN_POINT('Ctrl Pts',(-34.5853023124368,-12.936096085427,33.9093989968765));
#27274=CARTESIAN_POINT('Ctrl Pts',(-34.064851465877,-12.8919045823054,33.7890241943272));
#27275=CARTESIAN_POINT('Ctrl Pts',(-34.2259804977875,-12.8919045823054,
34.2776633590166));
#27276=CARTESIAN_POINT('Ctrl Pts',(-34.585302306524,-12.8919045823054,33.9093990029364));
#27277=CARTESIAN_POINT('Origin',(-34.361632442815,-12.8919045823054,33.691160504801));
#27278=CARTESIAN_POINT('Origin',(0.0835265683620477,-11.3294045823054,0.0824317919394229));
#27279=CARTESIAN_POINT('Origin',(-20.394360840366,-11.3294045823054,-6.6701627853663));
#27280=CARTESIAN_POINT('Origin',(-6.66906800894368,-11.3294045823054,20.5603192006674));
#27281=CARTESIAN_POINT('Origin',(-6.66906800894368,-11.3294045823054,20.5603192006674));
#27282=CARTESIAN_POINT('Ctrl Pts',(42.9952736832849,-14.9232028613467,37.2662146291476));
#27283=CARTESIAN_POINT('Ctrl Pts',(43.262083132434,-14.6181128259928,37.3541951909867));
#27284=CARTESIAN_POINT('Ctrl Pts',(43.0636720738749,-14.7022319922259,37.7085464415881));
#27285=CARTESIAN_POINT('Ctrl Pts',(42.5112271215405,-14.4538621299839,37.106600010571));
#27286=CARTESIAN_POINT('Ctrl Pts',(42.7777192980699,-14.147074607234,37.1944759515764));
#27287=CARTESIAN_POINT('Ctrl Pts',(42.5791171508971,-14.2328912595879,37.5495125198651));
#27288=CARTESIAN_POINT('Ctrl Pts',(42.0266693850915,-13.9850662226618,36.9468168318559));
#27289=CARTESIAN_POINT('Ctrl Pts',(42.2935697537446,-13.6772499732431,37.0348273744504));
#27290=CARTESIAN_POINT('Ctrl Pts',(42.0940349090533,-13.7640953522125,37.3903223553195));
#27291=CARTESIAN_POINT('Ctrl Pts',(41.5416017773197,-13.5169045823054,36.7868655227931));
#27292=CARTESIAN_POINT('Ctrl Pts',(41.8097676469788,-13.2088427643879,36.8752933650375));
#27293=CARTESIAN_POINT('Ctrl Pts',(41.6084251757828,-13.2959337131846,37.2309770398429));
#27294=CARTESIAN_POINT('Ctrl Pts',(43.0359437585039,-14.6753754510085,37.6994458554132));
#27295=CARTESIAN_POINT('Ctrl Pts',(43.0437650201411,-14.6771438430878,37.6931993723333));
#27296=CARTESIAN_POINT('Ctrl Pts',(43.0511197893374,-14.6786525232815,37.6863023375307));
#27297=CARTESIAN_POINT('Ctrl Pts',(43.0578129301505,-14.6799030932779,37.678804973348));
#27298=CARTESIAN_POINT('Ctrl Pts',(43.0643231830576,-14.681119491854,37.6715124722146));
#27299=CARTESIAN_POINT('Ctrl Pts',(43.0702066967261,-14.6820924420366,37.6636521449987));
#27300=CARTESIAN_POINT('Ctrl Pts',(43.075289676931,-14.6828029998434,37.6553127292641));
#27301=CARTESIAN_POINT('Ctrl Pts',(43.0802767004004,-14.6835001437071,37.6471307454057));
#27302=CARTESIAN_POINT('Ctrl Pts',(43.0844923876095,-14.6839452832804,37.6384881509309));
#27303=CARTESIAN_POINT('Ctrl Pts',(43.0877895089784,-14.6840907481788,37.6295050829525));
#27304=CARTESIAN_POINT('Ctrl Pts',(43.0910495157316,-14.6842345756264,37.6206231344291));
#27305=CARTESIAN_POINT('Ctrl Pts',(43.0934109488286,-14.6840857258448,37.6114092174673));
#27306=CARTESIAN_POINT('Ctrl Pts',(43.0947580631468,-14.6835622048232,37.6020045512144));
#27307=CARTESIAN_POINT('Ctrl Pts',(43.0949428628685,-14.683490387207,37.6007144010897));
#27308=CARTESIAN_POINT('Ctrl Pts',(43.0951086225669,-14.6834114599927,37.5994206874669));
#27309=CARTESIAN_POINT('Ctrl Pts',(43.095255090887,-14.6833251552391,37.5981237965455));
#27310=CARTESIAN_POINT('Ctrl Pts',(43.0966138582008,-14.6825245174079,37.5860927102892));
#27311=CARTESIAN_POINT('Ctrl Pts',(43.0964603511804,-14.6812727698323,37.5740720224458));
#27312=CARTESIAN_POINT('Ctrl Pts',(43.0950823298483,-14.679660389819,37.5622300656422));
#27313=CARTESIAN_POINT('Ctrl Pts',(43.093667437698,-14.6780048684051,37.5500712613228));
#27314=CARTESIAN_POINT('Ctrl Pts',(43.090962564536,-14.6759682812647,37.5381006221555));
#27315=CARTESIAN_POINT('Ctrl Pts',(43.0872892963239,-14.6736566051529,37.526446083814));
#27316=CARTESIAN_POINT('Ctrl Pts',(43.0834525783029,-14.6712420661416,37.5142729522322));
#27317=CARTESIAN_POINT('Ctrl Pts',(43.0785602210309,-14.6685267231679,37.5024441163509));
#27318=CARTESIAN_POINT('Ctrl Pts',(43.0729753261427,-14.6656525103353,37.4910532094055));
#27319=CARTESIAN_POINT('Ctrl Pts',(43.0717676935356,-14.6650310137439,37.4885901315988));
#27320=CARTESIAN_POINT('Ctrl Pts',(43.0705276424938,-14.6644021844316,37.486147363895));
#27321=CARTESIAN_POINT('Ctrl Pts',(43.0692587709865,-14.6637676196428,37.4837255967772));
#27322=CARTESIAN_POINT('Ctrl Pts',(43.0626898910944,-14.6604825116884,37.4711882380042));
#27323=CARTESIAN_POINT('Ctrl Pts',(43.0553951151393,-14.6571124630582,37.4591373845352));
#27324=CARTESIAN_POINT('Ctrl Pts',(43.0475293371387,-14.6536176840779,37.4475549388437));
#27325=CARTESIAN_POINT('Ctrl Pts',(43.0393170978584,-14.6499689717425,37.4354623250598));
#27326=CARTESIAN_POINT('Ctrl Pts',(43.0304828845192,-14.6461842219896,37.4238791913252));
#27327=CARTESIAN_POINT('Ctrl Pts',(43.0211759207055,-14.6422568272867,37.4127532083216));
#27328=CARTESIAN_POINT('Ctrl Pts',(43.0112246040603,-14.6380575256604,37.400856935587));
#27329=CARTESIAN_POINT('Ctrl Pts',(43.000733118812,-14.633695204416,37.3894821905549));
#27330=CARTESIAN_POINT('Ctrl Pts',(42.9898473507829,-14.6292054571919,37.3785473267842));
#27331=CARTESIAN_POINT('Ctrl Pts',(42.9781990027406,-14.624401189992,37.3668464436992));
#27332=CARTESIAN_POINT('Ctrl Pts',(42.9660992717873,-14.6194513461048,37.355648033558));
#27333=CARTESIAN_POINT('Ctrl Pts',(42.9536832408992,-14.6144447802759,37.3448514158025));
#27334=CARTESIAN_POINT('Ctrl Pts',(42.941267210011,-14.6094382144471,37.334054798047));
#27335=CARTESIAN_POINT('Ctrl Pts',(42.9285343617696,-14.6043757482479,37.3236591241839));
#27336=CARTESIAN_POINT('Ctrl Pts',(42.9155818628024,-14.5993802185557,37.3135788004322));
#27337=CARTESIAN_POINT('Ctrl Pts',(42.8962894060687,-14.591939489111,37.2985643842694));
#27338=CARTESIAN_POINT('Ctrl Pts',(42.8764459695827,-14.5844764296233,37.2843215640082));
#27339=CARTESIAN_POINT('Ctrl Pts',(42.856170967152,-14.5769485180958,37.2707744162756));
#27340=CARTESIAN_POINT('Ctrl Pts',(42.834697130939,-14.5689754912259,37.2564262438126));
#27341=CARTESIAN_POINT('Ctrl Pts',(42.8127390058597,-14.5609303686276,37.2428570639408));
#27342=CARTESIAN_POINT('Ctrl Pts',(42.7903962775658,-14.5528049305382,37.229980197936));
#27343=CARTESIAN_POINT('Ctrl Pts',(42.7658972710589,-14.5438953131449,37.2158605962522));
#27344=CARTESIAN_POINT('Ctrl Pts',(42.7409353913648,-14.5348900830952,37.2025719529671));
#27345=CARTESIAN_POINT('Ctrl Pts',(42.7155973478082,-14.5258150805526,37.1900277465265));
#27346=CARTESIAN_POINT('Ctrl Pts',(42.6891346188931,-14.5163372638596,37.1769267376128));
#27347=CARTESIAN_POINT('Ctrl Pts',(42.6622603264008,-14.5067848826421,37.1646370305515));
#27348=CARTESIAN_POINT('Ctrl Pts',(42.6350409751707,-14.4972049637156,37.153106204072));
#27349=CARTESIAN_POINT('Ctrl Pts',(42.6066694342357,-14.487219528733,37.1410872800091));
#27350=CARTESIAN_POINT('Ctrl Pts',(42.5779214158317,-14.4772057790315,37.1298929502604));
#27351=CARTESIAN_POINT('Ctrl Pts',(42.5488605293239,-14.4672106594487,37.1195178237689));
#27352=CARTESIAN_POINT('Ctrl Pts',(42.5364377106081,-14.462937990114,37.1150827107684));
#27353=CARTESIAN_POINT('Ctrl Pts',(42.5239577230844,-14.4586685042083,37.1107979333954));
#27354=CARTESIAN_POINT('Ctrl Pts',(42.5114260048381,-14.4544045238124,37.1066655924472));
#27355=CARTESIAN_POINT('Ctrl Pts',(39.1987322410677,-12.5761796977903,38.7430878994609));
#27356=CARTESIAN_POINT('Ctrl Pts',(39.4780446252898,-12.4966730216635,38.3474248665547));
#27357=CARTESIAN_POINT('Ctrl Pts',(39.1382020843858,-12.8445798972105,38.2941504721537));
#27358=CARTESIAN_POINT('Ctrl Pts',(39.3808518331676,-12.7679658886685,38.831628414024));
#27359=CARTESIAN_POINT('Ctrl Pts',(39.5085178360912,-12.6138199372454,38.4824096995347));
#27360=CARTESIAN_POINT('Ctrl Pts',(39.3246634921425,-12.9405865508064,38.3699715896931));
#27361=CARTESIAN_POINT('Ctrl Pts',(39.6159775649996,-12.9477999797133,38.8494978613861));
#27362=CARTESIAN_POINT('Ctrl Pts',(39.6750415100163,-12.8036087634362,38.5830901947362));
#27363=CARTESIAN_POINT('Ctrl Pts',(39.5504499068629,-13.0304169137554,38.4148517236754));
#27364=CARTESIAN_POINT('Ctrl Pts',(39.9548358734585,-13.1418528526574,38.7796080468698));
#27365=CARTESIAN_POINT('Ctrl Pts',(39.960999963987,-13.0167291165573,38.5935423303748));
#27366=CARTESIAN_POINT('Ctrl Pts',(39.8616681613932,-13.1274080636025,38.4271929768978));
#27367=CARTESIAN_POINT('Ctrl Pts',(40.0571173600845,-13.1924895597094,38.7468639463194));
#27368=CARTESIAN_POINT('Ctrl Pts',(40.0465003630512,-13.072136008791,38.5846653313979));
#27369=CARTESIAN_POINT('Ctrl Pts',(39.9538574541801,-13.1527155106484,38.4245349001724));
#27370=CARTESIAN_POINT('Ctrl Pts',(40.2987174380344,-13.2848578326186,38.6292554066571));
#27371=CARTESIAN_POINT('Ctrl Pts',(40.2485456959896,-13.176690865436,38.5251285662321));
#27372=CARTESIAN_POINT('Ctrl Pts',(40.1655692505595,-13.1988763557094,38.3961928595937));
#27373=CARTESIAN_POINT('Ctrl Pts',(40.4365733990678,-13.3151873395665,38.5290256968038));
#27374=CARTESIAN_POINT('Ctrl Pts',(40.3702936127468,-13.2202535090894,38.460793898628));
#27375=CARTESIAN_POINT('Ctrl Pts',(40.2811022909383,-13.2140287022007,38.3620259985628));
#27376=CARTESIAN_POINT('Ctrl Pts',(40.5291981978548,-13.2823030560792,38.3833348140131));
#27377=CARTESIAN_POINT('Ctrl Pts',(40.4486655654144,-13.2034487358322,38.3536972626374));
#27378=CARTESIAN_POINT('Ctrl Pts',(40.3477835278082,-13.1975864244367,38.2956850594486));
#27379=CARTESIAN_POINT('Origin',(39.1367104049936,-12.8919045823054,38.6262639337916));
#27380=CARTESIAN_POINT('Origin',(33.0778695430594,-12.8919045823054,35.9702546803237));
#27381=CARTESIAN_POINT('Origin',(33.0778695430594,-12.8919045823054,35.9702546803237));
#27382=CARTESIAN_POINT('Origin',(-34.361632442815,-14.7669045823054,33.691160504801));
#27383=CARTESIAN_POINT('Origin',(-34.361632442815,-11.3294045823054,33.691160504801));
#27384=CARTESIAN_POINT('Origin',(-20.3943608403659,-11.3294045823054,-6.67016278536651));
#27385=CARTESIAN_POINT('Ctrl Pts',(-33.8679555443817,-11.0169045823054,
34.1897988458186));
#27386=CARTESIAN_POINT('Ctrl Pts',(-33.8790249460546,-11.0169045823054,
34.1677734184622));
#27387=CARTESIAN_POINT('Ctrl Pts',(-33.8899462267957,-11.0183080822731,
34.1459662914066));
#27388=CARTESIAN_POINT('Ctrl Pts',(-33.9007564985824,-11.0211596046334,
34.1243041234319));
#27389=CARTESIAN_POINT('Ctrl Pts',(-33.9113853399145,-11.0239632694552,
34.1030055149551));
#27390=CARTESIAN_POINT('Ctrl Pts',(-33.9219068783712,-11.0281667153314,
34.0818469358361));
#27391=CARTESIAN_POINT('Ctrl Pts',(-33.9323504244984,-11.0338614984773,
34.0607676029711));
#27392=CARTESIAN_POINT('Ctrl Pts',(-33.9350140049392,-11.0353139278358,
34.0553914119685));
#27393=CARTESIAN_POINT('Ctrl Pts',(-33.9376724809033,-11.0368636220489,
34.0500204262757));
#27394=CARTESIAN_POINT('Ctrl Pts',(-33.9403262734905,-11.038512634127,34.0446537457636));
#27395=CARTESIAN_POINT('Ctrl Pts',(-33.9500720656005,-11.0445684687007,
34.0249451397312));
#27396=CARTESIAN_POINT('Ctrl Pts',(-33.9595280764102,-11.0518127318511,
34.0057532193741));
#27397=CARTESIAN_POINT('Ctrl Pts',(-33.9686854830345,-11.0604015318982,
33.9871030085655));
#27398=CARTESIAN_POINT('Ctrl Pts',(-33.9778428896589,-11.0689903319452,
33.968452797757));
#27399=CARTESIAN_POINT('Ctrl Pts',(-33.9867018233878,-11.0789231726624,
33.9503439241685));
#27400=CARTESIAN_POINT('Ctrl Pts',(-33.9952386171108,-11.0904031558603,
33.9328327583415));
#27401=CARTESIAN_POINT('Ctrl Pts',(-33.9980489407163,-11.0941823812718,
33.9270680597579));
#27402=CARTESIAN_POINT('Ctrl Pts',(-34.0008137051527,-11.0981143207712,
33.9213931588931));
#27403=CARTESIAN_POINT('Ctrl Pts',(-34.0035399736574,-11.1022159367836,
33.9157934297787));
#27404=CARTESIAN_POINT('Ctrl Pts',(-34.0082085418066,-11.1092397034607,
33.9062042359987));
#27405=CARTESIAN_POINT('Ctrl Pts',(-34.0126937919884,-11.1166630537835,
33.8969802308828));
#27406=CARTESIAN_POINT('Ctrl Pts',(-34.0170055140338,-11.1245727500526,
33.8881013312154));
#27407=CARTESIAN_POINT('Ctrl Pts',(-34.0186386281196,-11.1275686380657,
33.8847383463196));
#27408=CARTESIAN_POINT('Ctrl Pts',(-34.0202466520755,-11.1306345602647,
33.8814252694475));
#27409=CARTESIAN_POINT('Ctrl Pts',(-34.0218293558254,-11.1337762021651,
33.8781625736533));
#27410=CARTESIAN_POINT('Ctrl Pts',(-34.0259301037929,-11.141916121994,33.8697090060497));
#27411=CARTESIAN_POINT('Ctrl Pts',(-34.029844606577,-11.1505315993467,33.8616271594708));
#27412=CARTESIAN_POINT('Ctrl Pts',(-34.033539078864,-11.1596598005335,33.8539932768864));
#27413=CARTESIAN_POINT('Ctrl Pts',(-34.0372335511508,-11.1687880017203,
33.8463593943019));
#27414=CARTESIAN_POINT('Ctrl Pts',(-34.0407103722858,-11.1784304387767,
33.8391781150135));
#27415=CARTESIAN_POINT('Ctrl Pts',(-34.0439204410529,-11.18862206557,33.8325214722905));
#27416=CARTESIAN_POINT('Ctrl Pts',(-34.0454466387641,-11.1934675809199,
33.8293566326483));
#27417=CARTESIAN_POINT('Ctrl Pts',(-34.046915666792,-11.1984446423577,33.8263088550353));
#27418=CARTESIAN_POINT('Ctrl Pts',(-34.0483201712657,-11.2035509891889,
33.8233938038582));
#27419=CARTESIAN_POINT('Ctrl Pts',(-34.051594172964,-11.2154542536579,33.8165986083399));
#27420=CARTESIAN_POINT('Ctrl Pts',(-34.0544613220038,-11.2278803704204,
33.8106424362858));
#27421=CARTESIAN_POINT('Ctrl Pts',(-34.056840045953,-11.2407256805043,33.805697585903));
#27422=CARTESIAN_POINT('Ctrl Pts',(-34.0591638383017,-11.2532743553093,
33.8008669263854));
#27423=CARTESIAN_POINT('Ctrl Pts',(-34.0610213391567,-11.2662226779411,
33.7970017910542));
#27424=CARTESIAN_POINT('Ctrl Pts',(-34.062356555885,-11.2794553416021,33.7942218688642));
#27425=CARTESIAN_POINT('Ctrl Pts',(-34.0636553759747,-11.2923272964232,
33.791517724502));
#27426=CARTESIAN_POINT('Ctrl Pts',(-34.06445991162,-11.3054678991079,33.7898406443579));
#27427=CARTESIAN_POINT('Ctrl Pts',(-34.0647396118803,-11.3187590936875,
33.7892574482984));
#27428=CARTESIAN_POINT('Ctrl Pts',(-34.0648140791939,-11.3222977373503,
33.7891021783543));
#27429=CARTESIAN_POINT('Ctrl Pts',(-34.064851465877,-11.3258470068799,33.7890241943272));
#27430=CARTESIAN_POINT('Ctrl Pts',(-34.064851465877,-11.3294045823054,33.7890241943272));
#27431=CARTESIAN_POINT('Origin',(0.0835265683620477,-11.3294045823054,0.0824317919394229));
#27432=CARTESIAN_POINT('Ctrl Pts',(42.9634361744535,-14.6563598281187,37.7375957880963));
#27433=CARTESIAN_POINT('Ctrl Pts',(43.0152755598457,-14.7669045823054,37.8141269532137));
#27434=CARTESIAN_POINT('Ctrl Pts',(43.0959610209804,-14.7669045823054,37.9343011683297));
#27435=CARTESIAN_POINT('Ctrl Pts',(43.0251556892479,-14.6732979129397,37.7164407335828));
#27436=CARTESIAN_POINT('Ctrl Pts',(43.0892175038907,-14.7669045823054,37.7863585316547));
#27437=CARTESIAN_POINT('Ctrl Pts',(43.1842232087159,-14.7669045823054,37.881209115481));
#27438=CARTESIAN_POINT('Ctrl Pts',(43.0716902715764,-14.6836226395009,37.6764598776803));
#27439=CARTESIAN_POINT('Ctrl Pts',(43.1499072765567,-14.7669045823054,37.7261013273251));
#27440=CARTESIAN_POINT('Ctrl Pts',(43.2565479977638,-14.7669045823054,37.7937637317459));
#27441=CARTESIAN_POINT('Ctrl Pts',(43.0976316625303,-14.6837071744111,37.5986181406452));
#27442=CARTESIAN_POINT('Ctrl Pts',(43.1868411123276,-14.7669045823054,37.6150902279279));
#27443=CARTESIAN_POINT('Ctrl Pts',(43.3084198250278,-14.7669045823054,37.6375340941341));
#27444=CARTESIAN_POINT('Ctrl Pts',(43.0976468821399,-14.6805726740665,37.5678665274605));
#27445=CARTESIAN_POINT('Ctrl Pts',(43.1888566429373,-14.7669045823055,37.5717104765813));
#27446=CARTESIAN_POINT('Ctrl Pts',(43.3148976072562,-14.7669045823054,37.5779620629119));
#27447=CARTESIAN_POINT('Ctrl Pts',(43.0733162886299,-14.6635276241059,37.474635535667));
#27448=CARTESIAN_POINT('Ctrl Pts',(43.1646316507186,-14.7669045823052,37.4441076009668));
#27449=CARTESIAN_POINT('Ctrl Pts',(43.3011453607231,-14.7669045823054,37.4025193023754));
#27450=CARTESIAN_POINT('Ctrl Pts',(43.0259131176636,-14.642479666692,37.4121085028892));
#27451=CARTESIAN_POINT('Ctrl Pts',(43.1081309591734,-14.7669045823054,37.3637507252828));
#27452=CARTESIAN_POINT('Ctrl Pts',(43.2493294050651,-14.7669045823054,37.2914481919115));
#27453=CARTESIAN_POINT('Ctrl Pts',(42.8231824197416,-14.5607785229662,37.2253968287826));
#27454=CARTESIAN_POINT('Ctrl Pts',(42.860006513641,-14.7669045823054,37.14139474828));
#27455=CARTESIAN_POINT('Ctrl Pts',(43.0108374746241,-14.7669045823054,36.9729006240994));
#27456=CARTESIAN_POINT('Ctrl Pts',(42.612287234451,-14.4859905466056,37.1300246791343));
#27457=CARTESIAN_POINT('Ctrl Pts',(42.5879336945949,-14.7669045823054,37.085517422922));
#27458=CARTESIAN_POINT('Ctrl Pts',(42.7420195871275,-14.7669045823054,36.8334121977696));
#27459=CARTESIAN_POINT('Ctrl Pts',(42.4099536223294,-14.4183787521173,37.0764201725757));
#27460=CARTESIAN_POINT('Ctrl Pts',(42.4017503726634,-14.7669045823054,37.1167798525067));
#27461=CARTESIAN_POINT('Ctrl Pts',(42.4769068720474,-14.7669045823054,36.7731031625989));
#27462=CARTESIAN_POINT('Origin',(42.6092896432871,-14.4544045823054,36.8098845986664));
#27463=CARTESIAN_POINT('Origin',(43.2021767306697,-14.4544045823054,37.8450299335598));
#27464=CARTESIAN_POINT('Origin',(0.0835265683620477,-14.4544045823054,0.0824317919394229));
#27465=CARTESIAN_POINT('Origin',(30.6299435607004,-14.4544045823054,48.5813824935285));
#27466=CARTESIAN_POINT('Ctrl Pts',(39.89356043033,-13.5144022946802,38.546784061645));
#27467=CARTESIAN_POINT('Ctrl Pts',(40.16741768324,-13.1933434804542,38.6370886406434));
#27468=CARTESIAN_POINT('Ctrl Pts',(39.9535961475603,-13.2935409795845,38.9983049336294));
#27469=CARTESIAN_POINT('Ctrl Pts',(37.1165167598647,-10.8876754010549,37.6310523918765));
#27470=CARTESIAN_POINT('Ctrl Pts',(37.3635232200226,-10.5315615552175,37.7125029072161));
#27471=CARTESIAN_POINT('Ctrl Pts',(37.1730026303393,-10.6668492051076,38.0862419429111));
#27472=CARTESIAN_POINT('Ctrl Pts',(34.317603164163,-8.28316551656738,36.7081091022954));
#27473=CARTESIAN_POINT('Ctrl Pts',(34.5552513595784,-7.90880841716609,36.7864737246854));
#27474=CARTESIAN_POINT('Ctrl Pts',(34.3698847268169,-8.06235638062368,37.1673862145963));
#27475=CARTESIAN_POINT('Ctrl Pts',(31.4870706148097,-5.72100918219894,35.7747394454477));
#27476=CARTESIAN_POINT('Ctrl Pts',(31.7699448945489,-5.37442442931235,35.8680173939828));
#27477=CARTESIAN_POINT('Ctrl Pts',(31.5339848667978,-5.50017070815072,36.2386314339953));
#27478=CARTESIAN_POINT('Ctrl Pts',(32.9800027480559,-7.07886051013688,36.2670346332676));
#27479=CARTESIAN_POINT('Ctrl Pts',(32.9461473542254,-6.97591157389001,36.2558716399581));
#27480=CARTESIAN_POINT('Ctrl Pts',(32.8998932107597,-6.87711064623292,36.2543779568787));
#27481=CARTESIAN_POINT('Ctrl Pts',(32.7952737153869,-6.68740381001556,36.2619519765855));
#27482=CARTESIAN_POINT('Ctrl Pts',(32.7365767239536,-6.59673597566759,36.2713199677746));
#27483=CARTESIAN_POINT('Ctrl Pts',(32.6073736644662,-6.42451466437639,36.3005256432273));
#27484=CARTESIAN_POINT('Ctrl Pts',(32.5379837469721,-6.34396835910597,36.3199676903523));
#27485=CARTESIAN_POINT('Ctrl Pts',(32.4226478919156,-6.23614184370368,36.3601920496742));
#27486=CARTESIAN_POINT('Ctrl Pts',(32.3823733185026,-6.20250856262141,36.375458100475));
#27487=CARTESIAN_POINT('Ctrl Pts',(32.2976871155079,-6.14483638321709,36.4114968076452));
#27488=CARTESIAN_POINT('Ctrl Pts',(32.2530602303314,-6.11985717446073,36.4321140290926));
#27489=CARTESIAN_POINT('Ctrl Pts',(32.2061415763531,-6.10843371318469,36.4583066739833));
#27490=CARTESIAN_POINT('Origin',(33.0778695430594,-14.7669045823054,35.9702546803237));
#27491=CARTESIAN_POINT('Origin',(33.0778695430594,-7.07886995352309,35.9702546803237));
#27492=CARTESIAN_POINT('Ctrl Pts',(-34.088419713945,-10.7044045823054,34.4112752552593));
#27493=CARTESIAN_POINT('Ctrl Pts',(-34.088419713945,-11.0169045823054,34.4112752552593));
#27494=CARTESIAN_POINT('Ctrl Pts',(-33.8679555443817,-11.0169045823054,
34.1897988458186));
#27495=CARTESIAN_POINT('Ctrl Pts',(-34.1509161335726,-10.7044046073822,
34.3490644704238));
#27496=CARTESIAN_POINT('Ctrl Pts',(-34.1271612526014,-11.0349449313272,
34.3727107802124));
#27497=CARTESIAN_POINT('Ctrl Pts',(-33.8928554776138,-11.0169045823054,
34.1402540109324));
#27498=CARTESIAN_POINT('Ctrl Pts',(-34.2116574899238,-10.718650676671,34.2882601726245));
#27499=CARTESIAN_POINT('Ctrl Pts',(-34.1595985812887,-11.0630714156278,
34.3403466741461));
#27500=CARTESIAN_POINT('Ctrl Pts',(-33.9170059419221,-11.0240276257398,
34.0917785581122));
#27501=CARTESIAN_POINT('Ctrl Pts',(-34.3291018131802,-10.7765752156551,
34.1701033562228));
#27502=CARTESIAN_POINT('Ctrl Pts',(-34.2108367877319,-11.1314870357705,
34.289393364263));
#27503=CARTESIAN_POINT('Ctrl Pts',(-33.9636138355068,-11.0529899027286,
33.9974925425165));
#27504=CARTESIAN_POINT('Ctrl Pts',(-34.3825217718355,-10.8185639645428,
34.1160547845883));
#27505=CARTESIAN_POINT('Ctrl Pts',(-34.2270713855228,-11.1704305366382,
34.2733844817198));
#27506=CARTESIAN_POINT('Ctrl Pts',(-33.9847686082005,-11.0739842709863,
33.9543184859346));
#27507=CARTESIAN_POINT('Ctrl Pts',(-34.4774469307935,-10.9314866347395,
34.0196546156364));
#27508=CARTESIAN_POINT('Ctrl Pts',(-34.2431347603941,-11.2441510617705,
34.2581798507015));
#27509=CARTESIAN_POINT('Ctrl Pts',(-34.0223069043039,-11.1304456109602,
33.8772616585451));
#27510=CARTESIAN_POINT('Ctrl Pts',(-34.516023514239,-10.999293715727,33.9802793527558));
#27511=CARTESIAN_POINT('Ctrl Pts',(-34.2411034316767,-11.2750326114057,
34.2608486663205));
#27512=CARTESIAN_POINT('Ctrl Pts',(-34.0375326396835,-11.1643491474262,
33.845758314463));
#27513=CARTESIAN_POINT('Ctrl Pts',(-34.5707068729028,-11.1560957480195,
33.9243738132403));
#27514=CARTESIAN_POINT('Ctrl Pts',(-34.2319619401124,-11.3160025899707,
34.2712078036082));
#27515=CARTESIAN_POINT('Ctrl Pts',(-34.0591022197643,-11.2427501667525,
33.8010164090556));
#27516=CARTESIAN_POINT('Ctrl Pts',(-34.5853023188946,-11.2411599901507,
33.909398990258));
#27517=CARTESIAN_POINT('Ctrl Pts',(-34.2259804943108,-11.3235538600013,
34.2776633628159));
#27518=CARTESIAN_POINT('Ctrl Pts',(-34.0648514633374,-11.2852822850309,
33.7890241866258));
#27519=CARTESIAN_POINT('Ctrl Pts',(-34.585302306524,-11.3294045823054,33.9093990029365));
#27520=CARTESIAN_POINT('Ctrl Pts',(-34.2259804977875,-11.3294045823054,
34.2776633590166));
#27521=CARTESIAN_POINT('Ctrl Pts',(-34.064851465877,-11.3294045823054,33.7890241943272));
#27522=CARTESIAN_POINT('Origin',(-33.8679555443817,-10.7044045823054,34.1897988458186));
#27523=CARTESIAN_POINT('Origin',(-59.8897726849335,-14.4544045823054,3.01076271456695));
#27524=CARTESIAN_POINT('Origin',(-6.66906800894368,-14.4544045823054,20.5603192006674));
#27525=CARTESIAN_POINT('Ctrl Pts',(29.4562490573973,-14.4313124010515,48.5189176227355));
#27526=CARTESIAN_POINT('Ctrl Pts',(29.457027776463,-14.7671408702893,48.4940514111173));
#27527=CARTESIAN_POINT('Ctrl Pts',(29.4442069949301,-14.7669045053135,48.830622722352));
#27528=CARTESIAN_POINT('Ctrl Pts',(29.6580315031289,-14.4776157931207,48.5229453229308));
#27529=CARTESIAN_POINT('Ctrl Pts',(29.6408602063225,-14.7670932226436,48.5472967386214));
#27530=CARTESIAN_POINT('Ctrl Pts',(29.6700944519785,-14.766904515933,48.8386638059359));
#27531=CARTESIAN_POINT('Ctrl Pts',(29.8559183695444,-14.5232222287052,48.5151507121236));
#27532=CARTESIAN_POINT('Ctrl Pts',(29.8496672956075,-14.7670538266229,48.575617303287));
#27533=CARTESIAN_POINT('Ctrl Pts',(29.8920282667238,-14.7669045263941,48.8230549709512));
#27534=CARTESIAN_POINT('Ctrl Pts',(30.2414866202549,-14.6124212350924,48.4696579185046));
#27535=CARTESIAN_POINT('Ctrl Pts',(30.2582336836672,-14.7669897766123,48.5617748098557));
#27536=CARTESIAN_POINT('Ctrl Pts',(30.3251881717043,-14.7669045468573,48.7320256532131));
#27537=CARTESIAN_POINT('Ctrl Pts',(30.4336015879291,-14.6570503433836,48.4332503467984));
#27538=CARTESIAN_POINT('Ctrl Pts',(30.469015311734,-14.7669625172365,48.5287063091267));
#27539=CARTESIAN_POINT('Ctrl Pts',(30.5422656826559,-14.766904557097,48.6586455548447));
#27540=CARTESIAN_POINT('Ctrl Pts',(30.5955174348047,-14.6947854519679,48.3612871498227));
#27541=CARTESIAN_POINT('Ctrl Pts',(30.6513166085568,-14.7669413153261,48.4283359008911));
#27542=CARTESIAN_POINT('Ctrl Pts',(30.7234018036246,-14.7669045657556,48.5155428809447));
#27543=CARTESIAN_POINT('Origin',(29.5568100599416,-14.4544045823054,48.8324317919394));
#27544=CARTESIAN_POINT('Ctrl Pts',(30.5121796307591,-14.6753754514261,48.3944071427343));
#27545=CARTESIAN_POINT('Ctrl Pts',(30.4827135809989,-14.6685167481303,48.4048602007603));
#27546=CARTESIAN_POINT('Ctrl Pts',(30.4529177837429,-14.6615856670199,48.4142233306906));
#27547=CARTESIAN_POINT('Ctrl Pts',(30.4229080014734,-14.654609080261,48.4226966921314));
#27548=CARTESIAN_POINT('Ctrl Pts',(30.3899725761781,-14.6469523485344,48.4319961185727));
#27549=CARTESIAN_POINT('Ctrl Pts',(30.3567792072589,-14.6392407575338,48.4402238158605));
#27550=CARTESIAN_POINT('Ctrl Pts',(30.3234353759554,-14.6314992383768,48.4475985057719));
#27551=CARTESIAN_POINT('Ctrl Pts',(30.2877811427954,-14.62322130755,48.4554841896691));
#27552=CARTESIAN_POINT('Ctrl Pts',(30.2519542200175,-14.6149090026934,48.462394188985));
#27553=CARTESIAN_POINT('Ctrl Pts',(30.2160434238487,-14.6065829337796,48.4685491967709));
#27554=CARTESIAN_POINT('Ctrl Pts',(30.1745971023505,-14.5969734300696,48.4756529777708));
#27555=CARTESIAN_POINT('Ctrl Pts',(30.1330381930019,-14.5873453832253,48.4817509213698));
#27556=CARTESIAN_POINT('Ctrl Pts',(30.0914599002124,-14.5777205278759,48.4871254258683));
#27557=CARTESIAN_POINT('Ctrl Pts',(30.0772090127902,-14.5744216254719,48.4889675279226));
#27558=CARTESIAN_POINT('Ctrl Pts',(30.0629555875867,-14.5711230389444,48.4907242246678));
#27559=CARTESIAN_POINT('Ctrl Pts',(30.0487027977647,-14.5678255143184,48.4924057571001));
#27560=CARTESIAN_POINT('Ctrl Pts',(30.0453826879077,-14.5670573738946,48.492797460933));
#27561=CARTESIAN_POINT('Ctrl Pts',(30.0420612970355,-14.566288983565,48.4931847014103));
#27562=CARTESIAN_POINT('Ctrl Pts',(30.0387385202705,-14.5655203189317,48.4935675089594));
#27563=CARTESIAN_POINT('Ctrl Pts',(29.9531991516571,-14.5457323247158,48.5034222534608));
#27564=CARTESIAN_POINT('Ctrl Pts',(29.8673665740185,-14.5259112556569,48.5102733066289));
#27565=CARTESIAN_POINT('Ctrl Pts',(29.7812847600966,-14.5060682995347,48.5145218129766));
#27566=CARTESIAN_POINT('Ctrl Pts',(29.7066446881537,-14.4888628108834,48.5182056203338));
#27567=CARTESIAN_POINT('Ctrl Pts',(29.6318168465408,-14.471640756376,48.5199316495389));
#27568=CARTESIAN_POINT('Ctrl Pts',(29.5568193301503,-14.4544067125516,48.5199317919306));
#27569=CARTESIAN_POINT('Ctrl Pts',(33.0027879519579,-7.15534954830154,36.2773306483844));
#27570=CARTESIAN_POINT('Ctrl Pts',(32.4289011688471,-7.11664814650066,36.1423065419147));
#27571=CARTESIAN_POINT('Ctrl Pts',(32.8618763023223,-7.18677502441217,35.7443400681459));
#27572=CARTESIAN_POINT('Ctrl Pts',(32.9716799988102,-7.03238137399795,36.2577971857996));
#27573=CARTESIAN_POINT('Ctrl Pts',(32.5024026040697,-7.0802116255979,36.0750148926511));
#27574=CARTESIAN_POINT('Ctrl Pts',(32.8767232401359,-7.01162141055725,35.7306646429359));
#27575=CARTESIAN_POINT('Ctrl Pts',(32.9138507450232,-6.90078625141428,36.2533276469428));
#27576=CARTESIAN_POINT('Ctrl Pts',(32.5473708083471,-6.94927177584817,36.0332686286228));
#27577=CARTESIAN_POINT('Ctrl Pts',(32.8536713561474,-6.83269992244044,35.7519247260262));
#27578=CARTESIAN_POINT('Ctrl Pts',(32.7893956376618,-6.6769719555354,36.2629255337844));
#27579=CARTESIAN_POINT('Ctrl Pts',(32.5534537676943,-6.69622936404116,36.0265991852956));
#27580=CARTESIAN_POINT('Ctrl Pts',(32.7730615057291,-6.5379598519392,35.8257956190207));
#27581=CARTESIAN_POINT('Ctrl Pts',(32.7264182119996,-6.58104909157649,36.2733890195365));
#27582=CARTESIAN_POINT('Ctrl Pts',(32.5376034872748,-6.57996991860998,36.0406005265092));
#27583=CARTESIAN_POINT('Ctrl Pts',(32.7232297664787,-6.41511471179781,35.8713726932354));
#27584=CARTESIAN_POINT('Ctrl Pts',(32.5887048620014,-6.40173475569555,36.3057781064803));
#27585=CARTESIAN_POINT('Ctrl Pts',(32.4714094556764,-6.36383534698751,36.099753191065));
#27586=CARTESIAN_POINT('Ctrl Pts',(32.5984331925844,-6.1927844440631,35.9847905294333));
#27587=CARTESIAN_POINT('Ctrl Pts',(32.5160977586742,-6.32050524456458,36.3270146377757));
#27588=CARTESIAN_POINT('Ctrl Pts',(32.4250055767998,-6.26307762141852,36.1413505743537));
#27589=CARTESIAN_POINT('Ctrl Pts',(32.5257164089387,-6.09580032219768,36.0506055708441));
#27590=CARTESIAN_POINT('Ctrl Pts',(32.3399099210657,-6.1637311406324,36.3907537841966));
#27591=CARTESIAN_POINT('Ctrl Pts',(32.2870207252597,-6.07811517888562,36.2644473800673));
#27592=CARTESIAN_POINT('Ctrl Pts',(32.328360008767,-5.92198390398685,36.2277488375675));
#27593=CARTESIAN_POINT('Ctrl Pts',(32.2375253657692,-6.09886182626739,36.4356892719343));
#27594=CARTESIAN_POINT('Ctrl Pts',(32.1881882760276,-6.00005797775949,36.3522768460648));
#27595=CARTESIAN_POINT('Ctrl Pts',(32.1993930425981,-5.86097989287912,36.3425656526602));
#27596=CARTESIAN_POINT('Ctrl Pts',(32.151529404332,-6.10268725738615,36.4911916688128));
#27597=CARTESIAN_POINT('Ctrl Pts',(32.0828811597279,-6.01584203958569,36.4449524222502));
#27598=CARTESIAN_POINT('Ctrl Pts',(32.0626197531438,-5.89881153273095,36.4627624082688));
#27599=CARTESIAN_POINT('Origin',(32.3524078891946,-5.88746284406389,36.6239396741003));
#27600=CARTESIAN_POINT('Origin',(0.0835265683620477,-10.7044045823054,0.0824317919394229));
#27601=CARTESIAN_POINT('Origin',(-29.4954827078206,-10.7044045823054,38.0442262073711));
#27602=CARTESIAN_POINT('Origin',(-15.3043526660546,-11.3294045823054,-4.99172980493867));
#27603=CARTESIAN_POINT('Ctrl Pts',(-29.2671708193829,-11.3294045823054,
38.3497289413026));
#27604=CARTESIAN_POINT('Ctrl Pts',(-29.2671708193829,-11.3124780874426,
38.3497289413026));
#27605=CARTESIAN_POINT('Ctrl Pts',(-29.2681709348334,-11.2956902155653,
38.3483582338347));
#27606=CARTESIAN_POINT('Ctrl Pts',(-29.2701189073547,-11.2792729854166,
38.3457454172439));
#27607=CARTESIAN_POINT('Ctrl Pts',(-29.2720812584704,-11.2627345745579,
38.3431133146366));
#27608=CARTESIAN_POINT('Ctrl Pts',(-29.2750050109582,-11.2465729047032,
38.3392208633812));
#27609=CARTESIAN_POINT('Ctrl Pts',(-29.2787966186959,-11.2309934053141,
38.3342127608102));
#27610=CARTESIAN_POINT('Ctrl Pts',(-29.2826398264079,-11.2152018845814,
38.3291365029917));
#27611=CARTESIAN_POINT('Ctrl Pts',(-29.2873740682792,-11.2000089946043,
38.3229142203174));
#27612=CARTESIAN_POINT('Ctrl Pts',(-29.2928692140188,-11.1855875760929,
38.3157073854842));
#27613=CARTESIAN_POINT('Ctrl Pts',(-29.2984084509705,-11.1710504449412,
38.3084427254181));
#27614=CARTESIAN_POINT('Ctrl Pts',(-29.3047201288968,-11.1572975033337,
38.3001778885712));
#27615=CARTESIAN_POINT('Ctrl Pts',(-29.3116480970033,-11.1444582968067,
38.2910858047855));
#27616=CARTESIAN_POINT('Ctrl Pts',(-29.3186726108507,-11.1314401675872,
38.2818670168995));
#27617=CARTESIAN_POINT('Ctrl Pts',(-29.3263299526575,-11.1193615571096,
38.2717980151597));
#27618=CARTESIAN_POINT('Ctrl Pts',(-29.3344452291491,-11.1083055247257,
38.2610630578265));
#27619=CARTESIAN_POINT('Ctrl Pts',(-29.3371174699017,-11.1046649364684,
38.2575281948438));
#27620=CARTESIAN_POINT('Ctrl Pts',(-29.3398393167612,-11.1011348042002,
38.2539211386765));
#27621=CARTESIAN_POINT('Ctrl Pts',(-29.3426044572242,-11.0977168667273,
38.2502484905411));
#27622=CARTESIAN_POINT('Ctrl Pts',(-29.3526728339503,-11.0852715379768,
38.236875714183));
#27623=CARTESIAN_POINT('Ctrl Pts',(-29.3633753634814,-11.0742682117852,
38.2226616223712));
#27624=CARTESIAN_POINT('Ctrl Pts',(-29.3745114120525,-11.0647125800551,
38.2078123856294));
#27625=CARTESIAN_POINT('Ctrl Pts',(-29.3869785886498,-11.054014732653,38.1911881714288));
#27626=CARTESIAN_POINT('Ctrl Pts',(-29.3999889739614,-11.0451301475312,
38.1737679429712));
#27627=CARTESIAN_POINT('Ctrl Pts',(-29.4133192132405,-11.038042002362,38.1558218117586));
#27628=CARTESIAN_POINT('Ctrl Pts',(-29.4281479300946,-11.0301570653,38.1358583217711));
#27629=CARTESIAN_POINT('Ctrl Pts',(-29.4433733452703,-11.0244934293336,
38.1152437539762));
#27630=CARTESIAN_POINT('Ctrl Pts',(-29.4587509031789,-11.0210242012062,
38.0943291909816));
#27631=CARTESIAN_POINT('Ctrl Pts',(-29.4709331196514,-11.0182758527174,
38.077760517637));
#27632=CARTESIAN_POINT('Ctrl Pts',(-29.483212604426,-11.0169045823054,38.0610029810114));
#27633=CARTESIAN_POINT('Ctrl Pts',(-29.4954827078206,-11.0169045823054,
38.0442262073711));
#27634=CARTESIAN_POINT('Origin',(0.0835265683620477,-14.4544045823054,0.0824317919394229));
#27635=CARTESIAN_POINT('Origin',(-19.1024092026003,-14.4544045823054,9.9232282456065));
#27636=CARTESIAN_POINT('Origin',(-44.291473431638,-14.4544045823054,48.8324317919394));
#27637=CARTESIAN_POINT('Origin',(-29.3897569232175,-14.4544045823054,48.8324317919394));
#27638=CARTESIAN_POINT('Ctrl Pts',(-30.3730808079888,-14.9741386829693,
48.5199317919394));
#27639=CARTESIAN_POINT('Ctrl Pts',(-30.4470643284216,-14.8357920829891,
48.5199317919394));
#27640=CARTESIAN_POINT('Ctrl Pts',(-30.4912615099722,-14.7531448966905,
48.3941168692887));
#27641=CARTESIAN_POINT('Ctrl Pts',(-28.3257761438679,-13.879302911696,48.5199317919394));
#27642=CARTESIAN_POINT('Ctrl Pts',(-28.4030221988792,-13.7458678866789,
48.5199317919394));
#27643=CARTESIAN_POINT('Ctrl Pts',(-28.4382824252071,-13.658307532674,48.3977071667607));
#27644=CARTESIAN_POINT('Ctrl Pts',(-26.2427249084523,-12.8434482903011,
48.5199317919394));
#27645=CARTESIAN_POINT('Ctrl Pts',(-26.3156315690958,-12.7103751542413,
48.5199317919394));
#27646=CARTESIAN_POINT('Ctrl Pts',(-26.3489689847425,-12.6224528665242,
48.401314352775));
#27647=CARTESIAN_POINT('Ctrl Pts',(-23.0464978220819,-11.4077451872917,
48.5199317919394));
#27648=CARTESIAN_POINT('Ctrl Pts',(-23.1068226074019,-11.2735898053156,
48.5199317919394));
#27649=CARTESIAN_POINT('Ctrl Pts',(-23.1422761975804,-11.1867499400309,
48.4065777408208));
#27650=CARTESIAN_POINT('Ctrl Pts',(-21.9690884615937,-10.9489604127228,
48.5199317919394));
#27651=CARTESIAN_POINT('Ctrl Pts',(-22.0269387797156,-10.8151504288072,
48.5199317919394));
#27652=CARTESIAN_POINT('Ctrl Pts',(-22.0611987595185,-10.727965027292,48.4083066876547));
#27653=CARTESIAN_POINT('Ctrl Pts',(-19.7863880449052,-10.0773547210577,
48.5199317919394));
#27654=CARTESIAN_POINT('Ctrl Pts',(-19.8391964327606,-9.94441815657253,
48.5199317919394));
#27655=CARTESIAN_POINT('Ctrl Pts',(-19.8707744411429,-9.85635900888291,
48.4116714313723));
#27656=CARTESIAN_POINT('Ctrl Pts',(-18.6820153475912,-9.66512413195019,
48.5199317919394));
#27657=CARTESIAN_POINT('Ctrl Pts',(-18.7320875059833,-9.53246556458702,
48.5199317919394));
#27658=CARTESIAN_POINT('Ctrl Pts',(-18.7623480724567,-9.44412830208715,
48.4133051537846));
#27659=CARTESIAN_POINT('Ctrl Pts',(-13.1435402678133,-7.75733423685904,
48.5199317919394));
#27660=CARTESIAN_POINT('Ctrl Pts',(-13.2048611762757,-7.63508483860035,
48.5199317919394));
#27661=CARTESIAN_POINT('Ctrl Pts',(-13.2028224703124,-7.53633525782087,
48.4210275580482));
#27662=CARTESIAN_POINT('Ctrl Pts',(-8.61498664508566,-6.70462823795387,
48.5199317919394));
#27663=CARTESIAN_POINT('Ctrl Pts',(-8.64606183255299,-6.57519149762604,
48.5199317919394));
#27664=CARTESIAN_POINT('Ctrl Pts',(-8.6547070114339,-6.48363668556085,48.4258275002683));
#27665=CARTESIAN_POINT('Ctrl Pts',(-3.94919441148868,-6.31501530004509,
48.5199317919394));
#27666=CARTESIAN_POINT('Ctrl Pts',(-3.9600208103548,-6.18536424665137,48.5199317919394));
#27667=CARTESIAN_POINT('Ctrl Pts',(-3.96764857725177,-6.09401826674954,
48.427604462906));
#27668=CARTESIAN_POINT('Ctrl Pts',(-30.3451264940348,-14.6753754514262,
48.3944071427339));
#27669=CARTESIAN_POINT('Ctrl Pts',(-30.3179204768622,-14.6690428075473,
48.4040584559733));
#27670=CARTESIAN_POINT('Ctrl Pts',(-30.2904148515138,-14.662644201776,48.4127711185442));
#27671=CARTESIAN_POINT('Ctrl Pts',(-30.2627186133094,-14.656204897716,48.4207135901973));
#27672=CARTESIAN_POINT('Ctrl Pts',(-30.233332298686,-14.6493726552408,48.4291407263725));
#27673=CARTESIAN_POINT('Ctrl Pts',(-30.2037309448942,-14.6424944891886,
48.4367006178514));
#27674=CARTESIAN_POINT('Ctrl Pts',(-30.1740000760399,-14.6355902170491,
48.4435574472146));
#27675=CARTESIAN_POINT('Ctrl Pts',(-30.1408726297333,-14.6278971722979,
48.4511976291304));
#27676=CARTESIAN_POINT('Ctrl Pts',(-30.1075839758143,-14.6201716175816,
48.4579649341589));
#27677=CARTESIAN_POINT('Ctrl Pts',(-30.0742050848433,-14.6124300278826,
48.4640429319486));
#27678=CARTESIAN_POINT('Ctrl Pts',(-30.0371113350464,-14.6038268483589,
48.4707973723365));
#27679=CARTESIAN_POINT('Ctrl Pts',(-29.9999050324531,-14.5952036013938,
48.476700265973));
#27680=CARTESIAN_POINT('Ctrl Pts',(-29.9626404188634,-14.586573014867,48.4819545588626));
#27681=CARTESIAN_POINT('Ctrl Pts',(-29.9352609645243,-14.5802318582854,
48.4858150489737));
#27682=CARTESIAN_POINT('Ctrl Pts',(-29.9078489587586,-14.5738864928743,
48.489324267419));
#27683=CARTESIAN_POINT('Ctrl Pts',(-29.880419746453,-14.5675406076309,48.4925504988627));
#27684=CARTESIAN_POINT('Ctrl Pts',(-29.8775679819405,-14.5668808376697,
48.4928859241836));
#27685=CARTESIAN_POINT('Ctrl Pts',(-29.874715080232,-14.5662208392319,48.4932180901505));
#27686=CARTESIAN_POINT('Ctrl Pts',(-29.8718609472941,-14.5655605905129,
48.4935470170228));
#27687=CARTESIAN_POINT('Ctrl Pts',(-29.7770689367495,-14.543632283427,48.5044713993929));
#27688=CARTESIAN_POINT('Ctrl Pts',(-29.6819707966549,-14.5216757688499,
48.5117080083146));
#27689=CARTESIAN_POINT('Ctrl Pts',(-29.5866135500324,-14.4997031659203,
48.5157983084356));
#27690=CARTESIAN_POINT('Ctrl Pts',(-29.5211163517266,-14.4846110362463,
48.5186077771193));
#27691=CARTESIAN_POINT('Ctrl Pts',(-29.4554966227567,-14.4695112274358,
48.5199316661313));
#27692=CARTESIAN_POINT('Ctrl Pts',(-29.3897662870071,-14.454406734056,48.5199317919305));
#27693=CARTESIAN_POINT('Ctrl Pts',(30.6582665472115,-14.7531486984913,48.3941518139883));
#27694=CARTESIAN_POINT('Ctrl Pts',(30.6140688077616,-14.8357969973016,48.5199317919394));
#27695=CARTESIAN_POINT('Ctrl Pts',(30.5400981996473,-14.974119567612,48.5199317919394));
#27696=CARTESIAN_POINT('Ctrl Pts',(28.6057879598596,-13.6585793127033,48.3977403664122));
#27697=CARTESIAN_POINT('Ctrl Pts',(28.5705202880773,-13.7461362596172,48.5199317919394));
#27698=CARTESIAN_POINT('Ctrl Pts',(28.4932902065677,-13.8795503180319,48.5199317919394));
#27699=CARTESIAN_POINT('Ctrl Pts',(26.5172528199154,-12.6231097579372,48.4013453007044));
#27700=CARTESIAN_POINT('Ctrl Pts',(26.4839031110322,-12.7110265271892,48.5199317919394));
#27701=CARTESIAN_POINT('Ctrl Pts',(26.4110144314125,-12.8440806269522,48.5199317919394));
#27702=CARTESIAN_POINT('Ctrl Pts',(23.3123676663596,-11.1881005852588,48.4066046257084));
#27703=CARTESIAN_POINT('Ctrl Pts',(23.2769083268454,-11.2749369500996,48.5199317919394));
#27704=CARTESIAN_POINT('Ctrl Pts',(23.2165890826852,-11.4090714544326,48.5199317919394));
#27705=CARTESIAN_POINT('Ctrl Pts',(22.2320010273984,-10.7295656511261,48.4083321070107));
#27706=CARTESIAN_POINT('Ctrl Pts',(22.1977338841284,-10.816746996713,48.5199317919394));
#27707=CARTESIAN_POINT('Ctrl Pts',(22.1398875138931,-10.9505365201866,48.5199317919394));
#27708=CARTESIAN_POINT('Ctrl Pts',(20.0432673812065,-9.85847188921382,48.4116937938316));
#27709=CARTESIAN_POINT('Ctrl Pts',(20.0116798199932,-9.9465258837596,48.5199317919394));
#27710=CARTESIAN_POINT('Ctrl Pts',(19.9588702805472,-10.0794427583948,48.5199317919394));
#27711=CARTESIAN_POINT('Ctrl Pts',(18.9337330064251,-9.44570717935327,48.4133290604129));
#27712=CARTESIAN_POINT('Ctrl Pts',(18.9034696740469,-9.534041625569,48.5199317919394));
#27713=CARTESIAN_POINT('Ctrl Pts',(18.8533926908108,-9.66667804843112,48.5199317919394));
#27714=CARTESIAN_POINT('Ctrl Pts',(13.3694457519523,-7.53595817693225,48.421057068387));
#27715=CARTESIAN_POINT('Ctrl Pts',(13.3715217464864,-7.63471881015203,48.5199317919394));
#27716=CARTESIAN_POINT('Ctrl Pts',(13.3101634587761,-7.75692904622486,48.5199317919394));
#27717=CARTESIAN_POINT('Ctrl Pts',(8.81975013992703,-6.48350292012916,48.4258551364495));
#27718=CARTESIAN_POINT('Ctrl Pts',(8.81109698109706,-6.57505277909527,48.5199317919394));
#27719=CARTESIAN_POINT('Ctrl Pts',(8.78004147867651,-6.70446830385567,48.5199317919394));
#27720=CARTESIAN_POINT('Ctrl Pts',(4.1347721482036,-6.09405046754032,48.4276308774903));
#27721=CARTESIAN_POINT('Ctrl Pts',(4.12714461181649,-6.18539206100947,48.5199317919394));
#27722=CARTESIAN_POINT('Ctrl Pts',(4.11631983879343,-6.31502133666111,48.5199317919394));
#27723=CARTESIAN_POINT('Origin',(0.0835265683620477,-5.88746284406389,0.0824317919394229));
#27724=CARTESIAN_POINT('Ctrl Pts',(-29.160961539262,-11.3806731527506,38.6952753670064));
#27725=CARTESIAN_POINT('Ctrl Pts',(-29.338612324035,-11.3615458677611,38.5607229831505));
#27726=CARTESIAN_POINT('Ctrl Pts',(-29.267993840028,-11.355038329106,38.3486314652747));
#27727=CARTESIAN_POINT('Ctrl Pts',(-29.1469683092902,-11.1940655922236,
38.7058349957559));
#27728=CARTESIAN_POINT('Ctrl Pts',(-29.3277662394871,-11.2445867745137,
38.5690297012891));
#27729=CARTESIAN_POINT('Ctrl Pts',(-29.2619210862101,-11.2617365123088,
38.3565409866893));
#27730=CARTESIAN_POINT('Ctrl Pts',(-29.2108659223156,-11.005746982716,38.6576671929678));
#27731=CARTESIAN_POINT('Ctrl Pts',(-29.3785562365388,-11.1260887991107,
38.5301523333543));
#27732=CARTESIAN_POINT('Ctrl Pts',(-29.2896584450123,-11.1675791667462,
38.3204717498946));
#27733=CARTESIAN_POINT('Ctrl Pts',(-29.4288521077717,-10.7559199031752,
38.4911511473035));
#27734=CARTESIAN_POINT('Ctrl Pts',(-29.531320611788,-10.9974050092333,38.4122642469566));
#27735=CARTESIAN_POINT('Ctrl Pts',(-29.3839622465767,-11.0426657522701,
38.1953495467773));
#27736=CARTESIAN_POINT('Ctrl Pts',(-29.5822502088183,-10.6922226877682,
38.3730436187048));
#27737=CARTESIAN_POINT('Ctrl Pts',(-29.6355429628529,-10.989329898915,38.3313082128754));
#27738=CARTESIAN_POINT('Ctrl Pts',(-29.4501718643539,-11.0108152119631,
38.1064437698431));
#27739=CARTESIAN_POINT('Ctrl Pts',(-29.7276737536381,-10.7063374043602,
38.2594300539962));
#27740=CARTESIAN_POINT('Ctrl Pts',(-29.7095248998334,-11.0262754939016,
38.2736037579977));
#27741=CARTESIAN_POINT('Ctrl Pts',(-29.5127338402293,-11.0178704044763,
38.0205548953693));
#27742=CARTESIAN_POINT('Origin',(-28.9703898424448,-11.3294045823054,38.4475926308288));
#27743=CARTESIAN_POINT('Origin',(-19.6585232829181,-14.4544045823054,10.2084687225244));
#27744=CARTESIAN_POINT('Origin',(-20.2520852367942,-14.4544045823054,10.012741343472));
#27745=CARTESIAN_POINT('Ctrl Pts',(-29.3897569232175,-14.7669045823054,
48.8324317919395));
#27746=CARTESIAN_POINT('Ctrl Pts',(-29.3897569232175,-14.7669045823054,
48.5199317919395));
#27747=CARTESIAN_POINT('Ctrl Pts',(-29.3897569232175,-14.4544045823054,
48.5199317919395));
#27748=CARTESIAN_POINT('Ctrl Pts',(-29.5753563162698,-14.7669045823054,
48.8324317903168));
#27749=CARTESIAN_POINT('Ctrl Pts',(-29.546032736532,-14.7669045823054,48.5558431486859));
#27750=CARTESIAN_POINT('Ctrl Pts',(-29.5554686170235,-14.4924842730195,
48.5199317919395));
#27751=CARTESIAN_POINT('Ctrl Pts',(-29.7590263505073,-14.7669045823054,
48.8155939483766));
#27752=CARTESIAN_POINT('Ctrl Pts',(-29.7181422659514,-14.7669045823057,
48.5742539860857));
#27753=CARTESIAN_POINT('Ctrl Pts',(-29.7192039348074,-14.5302415322824,
48.5115128647378));
#27754=CARTESIAN_POINT('Ctrl Pts',(-30.1212331836543,-14.7669045823054,
48.7397392940007));
#27755=CARTESIAN_POINT('Ctrl Pts',(-30.0594836612501,-14.7669045823051,
48.5629091789621));
#27756=CARTESIAN_POINT('Ctrl Pts',(-30.0416350168231,-14.6048328837018,
48.4735855483903));
#27757=CARTESIAN_POINT('Ctrl Pts',(-30.3036979301853,-14.7669045823054,
48.6816475550023));
#27758=CARTESIAN_POINT('Ctrl Pts',(-30.2357168106316,-14.7669045823056,
48.5381854201266));
#27759=CARTESIAN_POINT('Ctrl Pts',(-30.2033686385937,-14.6423789509996,
48.4446955724101));
#27760=CARTESIAN_POINT('Ctrl Pts',(-30.4628904239763,-14.7669045823054,
48.5813824935285));
#27761=CARTESIAN_POINT('Ctrl Pts',(-30.3939059109749,-14.7669045823054,
48.4718548688625));
#27762=CARTESIAN_POINT('Ctrl Pts',(-30.3451264940348,-14.6753754514262,
48.3944071427339));
#27763=CARTESIAN_POINT('Origin',(-30.4628904239763,-14.4544045823054,48.5813824935285));
#27764=CARTESIAN_POINT('Ctrl Pts',(0.0835265683815503,-6.00666333723547,
48.5199460669664));
#27765=CARTESIAN_POINT('Ctrl Pts',(0.0835265683810243,-5.9853111687807,
48.5199456014727));
#27766=CARTESIAN_POINT('Ctrl Pts',(0.0835265683704475,-5.96223275463529,
48.5195872927805));
#27767=CARTESIAN_POINT('Ctrl Pts',(0.0835265683683665,-5.92795641804995,
48.5154826407816));
#27768=CARTESIAN_POINT('Ctrl Pts',(0.0835265683679874,-5.90583775506839,
48.5199317919394));
#27769=CARTESIAN_POINT('Ctrl Pts',(0.0835265683620106,-5.88746284406389,
48.5199317919394));
#27770=CARTESIAN_POINT('Ctrl Pts',(-0.267518736492766,-6.00132529512186,
48.519945950593));
#27771=CARTESIAN_POINT('Ctrl Pts',(-0.189662915894568,-5.98270666392106,
48.5198859104319));
#27772=CARTESIAN_POINT('Ctrl Pts',(-0.172476876202251,-5.9624068608038,
48.5196215918924));
#27773=CARTESIAN_POINT('Ctrl Pts',(-0.194279273758627,-5.92787973562319,
48.5154600083357));
#27774=CARTESIAN_POINT('Ctrl Pts',(-0.233267711014883,-5.90583775506839,
48.5199317919395));
#27775=CARTESIAN_POINT('Ctrl Pts',(-0.267760844335869,-5.88746284406389,
48.5199317919394));
#27776=CARTESIAN_POINT('Ctrl Pts',(-0.61861597912618,-5.99973567328081,
48.5184885224508));
#27777=CARTESIAN_POINT('Ctrl Pts',(-0.485248141372782,-5.98152768121125,
48.5186918880749));
#27778=CARTESIAN_POINT('Ctrl Pts',(-0.459481328260318,-5.96239709811729,
48.51825758671));
#27779=CARTESIAN_POINT('Ctrl Pts',(-0.500506504809839,-5.92723732580309,
48.5133469044267));
#27780=CARTESIAN_POINT('Ctrl Pts',(-0.567298494478176,-5.90562906540035,
48.5168141308037));
#27781=CARTESIAN_POINT('Ctrl Pts',(-0.619048262304899,-5.88746284406389,
48.5161104362146));
#27782=CARTESIAN_POINT('Ctrl Pts',(-1.32094154226152,-5.99820579736984,
48.5087577021076));
#27783=CARTESIAN_POINT('Ctrl Pts',(-1.12790203317576,-5.97907559060225,
48.5103258779008));
#27784=CARTESIAN_POINT('Ctrl Pts',(-1.09571051581296,-5.96099214798813,
48.509167391218));
#27785=CARTESIAN_POINT('Ctrl Pts',(-1.16018842027523,-5.92511301754142,
48.502095049591));
#27786=CARTESIAN_POINT('Ctrl Pts',(-1.25685784210449,-5.9049506781467,48.5026532295389));
#27787=CARTESIAN_POINT('Ctrl Pts',(-1.32154021141508,-5.88746284406389,
48.50082319184));
#27788=CARTESIAN_POINT('Ctrl Pts',(-1.67216986276346,-5.99826554329992,
48.5004843099067));
#27789=CARTESIAN_POINT('Ctrl Pts',(-1.47497921394887,-5.97774718230281,
48.503027618363));
#27790=CARTESIAN_POINT('Ctrl Pts',(-1.44494172976745,-5.95954166014524,
48.501314877539));
#27791=CARTESIAN_POINT('Ctrl Pts',(-1.51364329257245,-5.92360346889973,
48.4928930594133));
#27792=CARTESIAN_POINT('Ctrl Pts',(-1.61238233956212,-5.90448098056108,
48.4916098859259));
#27793=CARTESIAN_POINT('Ctrl Pts',(-1.67274475309919,-5.88746284406389,
48.489357302818));
#27794=CARTESIAN_POINT('Ctrl Pts',(-2.37478478398615,-5.99418693015723,
48.4732202209247));
#27795=CARTESIAN_POINT('Ctrl Pts',(-2.22731576266703,-5.97194742955367,
48.4746917382575));
#27796=CARTESIAN_POINT('Ctrl Pts',(-2.20580868408144,-5.95413393118541,
48.4721918658702));
#27797=CARTESIAN_POINT('Ctrl Pts',(-2.25808685942607,-5.91998502842415,
48.4637155122428));
#27798=CARTESIAN_POINT('Ctrl Pts',(-2.33187211335798,-5.90343694889074,
48.4610292841225));
#27799=CARTESIAN_POINT('Ctrl Pts',(-2.37498775707879,-5.88746284406389,
48.4587755322629));
#27800=CARTESIAN_POINT('Ctrl Pts',(-2.72575170752853,-5.99381953117216,
48.4556040546437));
#27801=CARTESIAN_POINT('Ctrl Pts',(-2.60287727359779,-5.97081802552583,
48.4559496853464));
#27802=CARTESIAN_POINT('Ctrl Pts',(-2.5878494531497,-5.95257589046842,48.4528734062221));
#27803=CARTESIAN_POINT('Ctrl Pts',(-2.63432748026306,-5.91860436677926,
48.4445443128869));
#27804=CARTESIAN_POINT('Ctrl Pts',(-2.69583332782557,-5.90286261480602,
48.4414922321791));
#27805=CARTESIAN_POINT('Ctrl Pts',(-2.72602622991915,-5.88746284406389,
48.439659649984));
#27806=CARTESIAN_POINT('Ctrl Pts',(-3.42730927258553,-5.99717808806687,
48.4131737559685));
#27807=CARTESIAN_POINT('Ctrl Pts',(-3.35965513432601,-5.97321241327165,
48.40967665781));
#27808=CARTESIAN_POINT('Ctrl Pts',(-3.35545842699348,-5.9531419369947,48.4051808771911));
#27809=CARTESIAN_POINT('Ctrl Pts',(-3.38522478840966,-5.9173715840225,48.3973032871653));
#27810=CARTESIAN_POINT('Ctrl Pts',(-3.4191878571586,-5.90176568155595,48.3944770847015));
#27811=CARTESIAN_POINT('Ctrl Pts',(-3.42785327106268,-5.8874628440639,48.3937688119853));
#27812=CARTESIAN_POINT('Ctrl Pts',(-3.77789991410016,-6.00090404394665,
48.3883596235742));
#27813=CARTESIAN_POINT('Ctrl Pts',(-3.74087148412348,-5.97673620504531,
48.3821456831845));
#27814=CARTESIAN_POINT('Ctrl Pts',(-3.74102460738878,-5.95526602423798,
48.3768070663123));
#27815=CARTESIAN_POINT('Ctrl Pts',(-3.75987742959583,-5.91751946291062,
48.3692339775274));
#27816=CARTESIAN_POINT('Ctrl Pts',(-3.77857712853757,-5.9012430823906,48.3669995056146));
#27817=CARTESIAN_POINT('Ctrl Pts',(-3.77864184991379,-5.8874628440639,48.3669938551438));
#27818=CARTESIAN_POINT('Ctrl Pts',(-4.128454810656,-6.007051447105,48.3603316468569));
#27819=CARTESIAN_POINT('Ctrl Pts',(-4.12834943621599,-5.98314272027372,
48.3503998997031));
#27820=CARTESIAN_POINT('Ctrl Pts',(-4.12855150591046,-5.95992641567859,
48.3444127441005));
#27821=CARTESIAN_POINT('Ctrl Pts',(-4.12900833251941,-5.91876732373882,
48.3374043064722));
#27822=CARTESIAN_POINT('Ctrl Pts',(-4.12926308943388,-5.90082453639418,
48.3363830244465));
#27823=CARTESIAN_POINT('Ctrl Pts',(-4.12926308943388,-5.88746284406389,
48.3363830244465));
#27824=CARTESIAN_POINT('Origin',(-4.15507771262755,-5.88723161925861,48.6489825986039));
#27825=CARTESIAN_POINT('Origin',(-28.9703898424448,-14.7669045823054,38.4475926308288));
#27826=CARTESIAN_POINT('Origin',(-28.9703898424448,-12.8919045823054,38.4475926308288));
#27827=CARTESIAN_POINT('Origin',(-15.3043526660546,-14.4544045823054,-4.99172980493867));
#27828=CARTESIAN_POINT('Origin',(-32.2904773922958,-14.4544045823054,46.520314294909));
#27829=CARTESIAN_POINT('Origin',(0.0835265683620477,-14.4544045823054,0.0824317919394229));
#27830=CARTESIAN_POINT('Origin',(-32.0889297465829,-14.4544045823054,47.5183344911391));
#27831=CARTESIAN_POINT('Origin',(0.0835265683620477,-5.88746284406389,0.0824317919394229));
#27832=CARTESIAN_POINT('Origin',(-27.4181833845098,-5.88746284406389,40.3343690082786));
#27833=CARTESIAN_POINT('Origin',(-27.8490907775129,-14.7669045823054,40.036547827824));
#27834=CARTESIAN_POINT('Origin',(-27.8490907775129,-12.8919045823054,40.036547827824));
#27835=CARTESIAN_POINT('Origin',(-27.8490907775129,-6.59535043767466,40.036547827824));
#27836=CARTESIAN_POINT('Origin',(0.0835265683620477,-12.8919045823054,0.0824317919394229));
#27837=CARTESIAN_POINT('Ctrl Pts',(-29.1590516373201,-12.8919045823054,
38.6967170518605));
#27838=CARTESIAN_POINT('Ctrl Pts',(-29.1590516373201,-12.9139187960392,
38.6967170518605));
#27839=CARTESIAN_POINT('Ctrl Pts',(-29.1591848624577,-12.9356278245217,
38.6997029556855));
#27840=CARTESIAN_POINT('Ctrl Pts',(-29.159433947161,-12.9566097073225,38.7052239565964));
#27841=CARTESIAN_POINT('Ctrl Pts',(-29.1596773251019,-12.9771108756619,
38.7106184662385));
#27842=CARTESIAN_POINT('Ctrl Pts',(-29.1600313014214,-12.9969176625769,
38.7184329690427));
#27843=CARTESIAN_POINT('Ctrl Pts',(-29.1604800625459,-13.0156824718651,
38.7282608271112));
#27844=CARTESIAN_POINT('Ctrl Pts',(-29.1609427003112,-13.0350275286535,
38.7383925832896));
#27845=CARTESIAN_POINT('Ctrl Pts',(-29.1615060596073,-13.0532645768225,
38.7506637210088));
#27846=CARTESIAN_POINT('Ctrl Pts',(-29.1621534535084,-13.0700686738455,
38.7646490220121));
#27847=CARTESIAN_POINT('Ctrl Pts',(-29.1627579434982,-13.0857591343535,
38.7777074929781));
#27848=CARTESIAN_POINT('Ctrl Pts',(-29.1634356985008,-13.1002006435726,
38.7922604647321));
#27849=CARTESIAN_POINT('Ctrl Pts',(-29.1641737792839,-13.1131767225616,
38.8079815149163));
#27850=CARTESIAN_POINT('Ctrl Pts',(-29.1642261648535,-13.1140977047964,
38.8090973225455));
#27851=CARTESIAN_POINT('Ctrl Pts',(-29.1642788546012,-13.1150113249639,
38.8102190230898));
#27852=CARTESIAN_POINT('Ctrl Pts',(-29.1643318440343,-13.1159175149051,
38.8113465038983));
#27853=CARTESIAN_POINT('Ctrl Pts',(-29.1644679206162,-13.1182446058459,
38.8142418686074));
#27854=CARTESIAN_POINT('Ctrl Pts',(-29.16460601967,-13.1205242789863,38.817174852995));
#27855=CARTESIAN_POINT('Ctrl Pts',(-29.1647460246345,-13.1227565895721,
38.8201428584547));
#27856=CARTESIAN_POINT('Ctrl Pts',(-29.1654262109927,-13.1336018279011,
38.8345623244452));
#27857=CARTESIAN_POINT('Ctrl Pts',(-29.1661478962618,-13.1433259542984,
38.8497998614965));
#27858=CARTESIAN_POINT('Ctrl Pts',(-29.1669018579151,-13.1519718238984,
38.8656404993433));
#27859=CARTESIAN_POINT('Ctrl Pts',(-29.1677243343596,-13.1614033699958,
38.8829206241859));
#27860=CARTESIAN_POINT('Ctrl Pts',(-29.1685852378023,-13.1695524259102,
38.9009190345409));
#27861=CARTESIAN_POINT('Ctrl Pts',(-29.1694755597606,-13.1764446443666,
38.9194128816111));
#27862=CARTESIAN_POINT('Ctrl Pts',(-29.1704025310331,-13.1836205748858,
38.9386680115012));
#27863=CARTESIAN_POINT('Ctrl Pts',(-29.1713614497358,-13.189434638032,38.9584615530468));
#27864=CARTESIAN_POINT('Ctrl Pts',(-29.1723445987337,-13.1938753423316,
38.9785843074176));
#27865=CARTESIAN_POINT('Ctrl Pts',(-29.173333254577,-13.198340920045,38.9988197739984));
#27866=CARTESIAN_POINT('Ctrl Pts',(-29.1743464900272,-13.2014181302593,
39.019389799867));
#27867=CARTESIAN_POINT('Ctrl Pts',(-29.1753778401591,-13.2030479859147,
39.0401003436967));
#27868=CARTESIAN_POINT('Ctrl Pts',(-29.1759465980169,-13.2039468011497,
39.0515215712493));
#27869=CARTESIAN_POINT('Ctrl Pts',(-29.1765208826526,-13.2044045823054,
39.0629857191608));
#27870=CARTESIAN_POINT('Ctrl Pts',(-29.1770996549272,-13.2044045823054,
39.0744598620586));
#27871=CARTESIAN_POINT('Origin',(-27.8490907775129,-12.8919045823054,40.036547827824));
#27872=CARTESIAN_POINT('Ctrl Pts',(-29.2671708193829,-12.8919045823054,
38.3497289413026));
#27873=CARTESIAN_POINT('Ctrl Pts',(-29.3371224979176,-12.8919045823054,
38.5618640814605));
#27874=CARTESIAN_POINT('Ctrl Pts',(-29.1590516373201,-12.8919045823054,
38.6967170518605));
#27875=CARTESIAN_POINT('Ctrl Pts',(-29.2671708452715,-13.0608832998913,
38.3497290198124));
#27876=CARTESIAN_POINT('Ctrl Pts',(-29.3371225173464,-12.9975414109162,
38.5618641403768));
#27877=CARTESIAN_POINT('Ctrl Pts',(-29.1590516158475,-12.9763939382002,
38.6967170681218));
#27878=CARTESIAN_POINT('Ctrl Pts',(-29.2911696270366,-13.2263898891536,
38.4225076155515));
#27879=CARTESIAN_POINT('Ctrl Pts',(-29.3560557745662,-13.1003236725309,
38.6192810495675));
#27880=CARTESIAN_POINT('Ctrl Pts',(-29.161014348867,-13.0591472399316,38.7407134375252));
#27881=CARTESIAN_POINT('Ctrl Pts',(-29.3684014298945,-13.4534586900117,
38.6567204274108));
#27882=CARTESIAN_POINT('Ctrl Pts',(-29.4103322473219,-13.2166231342357,
38.7838796324259));
#27883=CARTESIAN_POINT('Ctrl Pts',(-29.1676166638971,-13.1726816319565,
38.881996315062));
#27884=CARTESIAN_POINT('Ctrl Pts',(-29.4214900734496,-13.5169045492971,
38.817716804871));
#27885=CARTESIAN_POINT('Ctrl Pts',(-29.4461016930836,-13.2287751252092,
38.8923538899239));
#27886=CARTESIAN_POINT('Ctrl Pts',(-29.1722839318329,-13.2044045823054,
38.9789882968653));
#27887=CARTESIAN_POINT('Ctrl Pts',(-29.4738806318652,-13.5169045823054,
38.9765961725324));
#27888=CARTESIAN_POINT('Ctrl Pts',(-29.4738806318652,-13.2044045823054,
38.9765961725324));
#27889=CARTESIAN_POINT('Ctrl Pts',(-29.1770996549272,-13.2044045823054,
39.0744598620586));
#27890=CARTESIAN_POINT('Origin',(-29.1770996549271,-13.5169045823054,39.0744598620586));
#27891=CARTESIAN_POINT('Ctrl Pts',(-31.9662912555927,-14.4267018210596,
46.5416570520116));
#27892=CARTESIAN_POINT('Ctrl Pts',(-31.938168182706,-14.766904582306,46.5537176466009));
#27893=CARTESIAN_POINT('Ctrl Pts',(-32.2529109022529,-14.7669045823054,
46.4201248733199));
#27894=CARTESIAN_POINT('Ctrl Pts',(-32.024734683047,-14.4797609665061,46.692175136077));
#27895=CARTESIAN_POINT('Ctrl Pts',(-32.043778675644,-14.7669045823045,46.6631128135208));
#27896=CARTESIAN_POINT('Ctrl Pts',(-32.3355543111131,-14.7669045823054,
46.6161921183141));
#27897=CARTESIAN_POINT('Ctrl Pts',(-32.0623733364669,-14.5360769750825,
46.8596692968509));
#27898=CARTESIAN_POINT('Ctrl Pts',(-32.1316825592432,-14.7669045823054,
46.8406276275195));
#27899=CARTESIAN_POINT('Ctrl Pts',(-32.3745755896651,-14.7669045823054,
46.8402083581988));
#27900=CARTESIAN_POINT('Ctrl Pts',(-32.0633148172228,-14.6333609973512,
47.1698657294858));
#27901=CARTESIAN_POINT('Ctrl Pts',(-32.1580599963963,-14.7669045823054,
47.1930718120375));
#27902=CARTESIAN_POINT('Ctrl Pts',(-32.3135212074945,-14.7669045823054,
47.2692900755125));
#27903=CARTESIAN_POINT('Ctrl Pts',(-32.0263650896152,-14.6768299128524,
47.3206255170885));
#27904=CARTESIAN_POINT('Ctrl Pts',(-32.1082092307808,-14.7669045823054,
47.3875168727934));
#27905=CARTESIAN_POINT('Ctrl Pts',(-32.2106516131303,-14.7669045823054,
47.4860887252743));
#27906=CARTESIAN_POINT('Ctrl Pts',(-31.9150640676236,-14.6796363815821,
47.3662735732131));
#27907=CARTESIAN_POINT('Ctrl Pts',(-31.9437759414398,-14.7669045823054,
47.452789218383));
#27908=CARTESIAN_POINT('Ctrl Pts',(-31.9869047021237,-14.7669045823054,
47.5712759627658));
#27909=CARTESIAN_POINT('Ctrl Pts',(-31.9648970362263,-14.6753754514101,
47.3354574511519));
#27910=CARTESIAN_POINT('Ctrl Pts',(-31.9735564605727,-14.6738626255535,
47.3277564171069));
#27911=CARTESIAN_POINT('Ctrl Pts',(-31.9814148868573,-14.672133306496,47.3193746779532));
#27912=CARTESIAN_POINT('Ctrl Pts',(-31.9885249956109,-14.6701816478973,
47.3104973988125));
#27913=CARTESIAN_POINT('Ctrl Pts',(-31.9958630049577,-14.6681674327095,
47.3013355758973));
#27914=CARTESIAN_POINT('Ctrl Pts',(-32.0024049887865,-14.6659157786115,
47.2916462220175));
#27915=CARTESIAN_POINT('Ctrl Pts',(-32.0082456503293,-14.6634429331545,
47.2815977859672));
#27916=CARTESIAN_POINT('Ctrl Pts',(-32.0144118761709,-14.6608322488258,
47.2709892400711));
#27917=CARTESIAN_POINT('Ctrl Pts',(-32.0197975133047,-14.6579745808513,
47.2599805552063));
#27918=CARTESIAN_POINT('Ctrl Pts',(-32.0245374663174,-14.6549226264771,
47.2487281978874));
#27919=CARTESIAN_POINT('Ctrl Pts',(-32.0294338809134,-14.6517699298356,
47.2371044103797));
#27920=CARTESIAN_POINT('Ctrl Pts',(-32.0336423882984,-14.6484098887067,
47.2252202530633));
#27921=CARTESIAN_POINT('Ctrl Pts',(-32.0373183972508,-14.6449389709832,
47.2132071216528));
#27922=CARTESIAN_POINT('Ctrl Pts',(-32.0411624851728,-14.6413093517216,
47.2006447111801));
#27923=CARTESIAN_POINT('Ctrl Pts',(-32.044425251709,-14.6375586122338,47.1879408085633));
#27924=CARTESIAN_POINT('Ctrl Pts',(-32.0472750829195,-14.6338375655311,
47.1752077273099));
#27925=CARTESIAN_POINT('Ctrl Pts',(-32.0478441028572,-14.6330945917876,
47.1726653391589));
#27926=CARTESIAN_POINT('Ctrl Pts',(-32.0483966054282,-14.6323529212119,
47.1701216848644));
#27927=CARTESIAN_POINT('Ctrl Pts',(-32.048933839889,-14.6316139267957,47.1675775138247));
#27928=CARTESIAN_POINT('Ctrl Pts',(-32.0526337697119,-14.6265244776274,
47.150055826385));
#27929=CARTESIAN_POINT('Ctrl Pts',(-32.0555021961016,-14.621344309823,47.1323873234176));
#27930=CARTESIAN_POINT('Ctrl Pts',(-32.0576643305193,-14.6160583702073,
47.114661556595));
#27931=CARTESIAN_POINT('Ctrl Pts',(-32.0599055390581,-14.6105791118847,
47.096287518591));
#27932=CARTESIAN_POINT('Ctrl Pts',(-32.0613890113421,-14.6049864174434,
47.0778513515879));
#27933=CARTESIAN_POINT('Ctrl Pts',(-32.0622469744254,-14.5993048356888,
47.0594133334773));
#27934=CARTESIAN_POINT('Ctrl Pts',(-32.0631510114803,-14.5933181440278,
47.0399851646972));
#27935=CARTESIAN_POINT('Ctrl Pts',(-32.0633615554861,-14.587233162304,47.0205542044588));
#27936=CARTESIAN_POINT('Ctrl Pts',(-32.0630080810849,-14.5811189364166,
47.0011584488534));
#27937=CARTESIAN_POINT('Ctrl Pts',(-32.0628890789164,-14.5790604955872,
46.9946285927458));
#27938=CARTESIAN_POINT('Ctrl Pts',(-32.0627058827591,-14.5769990340003,
46.9881025171608));
#27939=CARTESIAN_POINT('Ctrl Pts',(-32.06246257273,-14.5749379971507,46.9815811346738));
#27940=CARTESIAN_POINT('Ctrl Pts',(-32.0615130688658,-14.5668949154069,
46.9561318020068));
#27941=CARTESIAN_POINT('Ctrl Pts',(-32.0596357617387,-14.5588253828889,
46.9307664425349));
#27942=CARTESIAN_POINT('Ctrl Pts',(-32.0569499598408,-14.5507005312891,
46.905520730097));
#27943=CARTESIAN_POINT('Ctrl Pts',(-32.0540210533122,-14.5418402609492,
46.8779899088413));
#27944=CARTESIAN_POINT('Ctrl Pts',(-32.0501318587241,-14.5329148917832,
46.8506002843932));
#27945=CARTESIAN_POINT('Ctrl Pts',(-32.045398488845,-14.5239279943262,46.8233693228353));
#27946=CARTESIAN_POINT('Ctrl Pts',(-32.0404602839034,-14.5145521917657,
46.7949599501544));
#27947=CARTESIAN_POINT('Ctrl Pts',(-32.0346035375997,-14.5051108161098,
46.7667217647601));
#27948=CARTESIAN_POINT('Ctrl Pts',(-32.0279080163951,-14.4956334644579,
46.7386659092895));
#27949=CARTESIAN_POINT('Ctrl Pts',(-32.0209363322123,-14.4857652106525,
46.7094528640549));
#27950=CARTESIAN_POINT('Ctrl Pts',(-32.0130546915264,-14.4758595759615,
46.6804360413191));
#27951=CARTESIAN_POINT('Ctrl Pts',(-32.0042998405545,-14.4659531415325,
46.651642384214));
#27952=CARTESIAN_POINT('Ctrl Pts',(-32.0008975616248,-14.4621033383507,
46.6404526959834));
#27953=CARTESIAN_POINT('Ctrl Pts',(-31.9973629090797,-14.4582533144174,
46.6292969765153));
#27954=CARTESIAN_POINT('Ctrl Pts',(-31.9936964222114,-14.4544045595354,
46.6181780052196));
#27955=CARTESIAN_POINT('Ctrl Pts',(-27.2935253998823,-6.10843371318469,
40.1519176123711));
#27956=CARTESIAN_POINT('Ctrl Pts',(-27.2418903719914,-6.01690458230549,
40.0763437697123));
#27957=CARTESIAN_POINT('Ctrl Pts',(-27.2418903719914,-5.88746284406389,
40.0763437697123));
#27958=CARTESIAN_POINT('Ctrl Pts',(-27.325572359156,-6.10275018345656,40.1231384197862));
#27959=CARTESIAN_POINT('Ctrl Pts',(-27.2900413002514,-6.01222811250085,
40.0434451574011));
#27960=CARTESIAN_POINT('Ctrl Pts',(-27.3090641493039,-5.88746285448576,
40.0304479975372));
#27961=CARTESIAN_POINT('Ctrl Pts',(-27.3592234999427,-6.1141957746084,40.0998270880335));
#27962=CARTESIAN_POINT('Ctrl Pts',(-27.3386284262519,-6.02882146164725,
40.0101249754889));
#27963=CARTESIAN_POINT('Ctrl Pts',(-27.3762231578696,-5.91065570868276,
39.9842903529062));
#27964=CARTESIAN_POINT('Ctrl Pts',(-27.4199070979359,-6.16774318631831,
40.0709901510091));
#27965=CARTESIAN_POINT('Ctrl Pts',(-27.4166158072636,-6.09780352750759,
39.9565255115711));
#27966=CARTESIAN_POINT('Ctrl Pts',(-27.4898455402218,-5.99623773973482,
39.9058585933618));
#27967=CARTESIAN_POINT('Ctrl Pts',(-27.4472128335106,-6.20950986590621,
40.065114733074));
#27968=CARTESIAN_POINT('Ctrl Pts',(-27.446986984373,-6.15046547604274,39.9355946057315));
#27969=CARTESIAN_POINT('Ctrl Pts',(-27.5371343265496,-6.05824038173979,
39.8730380903669));
#27970=CARTESIAN_POINT('Ctrl Pts',(-27.5138459772748,-6.35463014070743,
40.068359994813));
#27971=CARTESIAN_POINT('Ctrl Pts',(-27.5066521003082,-6.32861804115436,
39.8945248287816));
#27972=CARTESIAN_POINT('Ctrl Pts',(-27.6431152180442,-6.26685602924669,
39.7993318216615));
#27973=CARTESIAN_POINT('Ctrl Pts',(-27.5397129060577,-6.47617237885517,
40.0962102326933));
#27974=CARTESIAN_POINT('Ctrl Pts',(-27.5039315392958,-6.4727604437398,39.8965578930712));
#27975=CARTESIAN_POINT('Ctrl Pts',(-27.6700355544528,-6.43425950785917,
39.7804316879677));
#27976=CARTESIAN_POINT('Ctrl Pts',(-27.5523098005748,-6.59535043767466,
40.1344115173502));
#27977=CARTESIAN_POINT('Ctrl Pts',(-27.4795079208223,-6.59535043767466,
39.9136328700245));
#27978=CARTESIAN_POINT('Ctrl Pts',(-27.6700355381162,-6.59535043767466,
39.7804316993888));
#27979=CARTESIAN_POINT('Ctrl Pts',(-27.5523097639759,-6.59535009141677,
40.1344114063608));
#27980=CARTESIAN_POINT('Ctrl Pts',(-27.549694674541,-6.57060902178217,40.1264809184535));
#27981=CARTESIAN_POINT('Ctrl Pts',(-27.5464955216116,-6.5457384076949,40.1189472692866));
#27982=CARTESIAN_POINT('Ctrl Pts',(-27.5426476143085,-6.52084484397761,
40.1119507718129));
#27983=CARTESIAN_POINT('Ctrl Pts',(-27.5397616703681,-6.50217458409161,
40.1067033742282));
#27984=CARTESIAN_POINT('Ctrl Pts',(-27.5365106509872,-6.48349034080867,
40.1017592884795));
#27985=CARTESIAN_POINT('Ctrl Pts',(-27.532847416671,-6.46482870577695,40.0971928287498));
#27986=CARTESIAN_POINT('Ctrl Pts',(-27.5314737038024,-6.45783059264005,
40.0954804063511));
#27987=CARTESIAN_POINT('Ctrl Pts',(-27.5300417965966,-6.45083562442592,
40.0938211965667));
#27988=CARTESIAN_POINT('Ctrl Pts',(-27.5285483060168,-6.44384570105556,
40.0922194417591));
#27989=CARTESIAN_POINT('Ctrl Pts',(-27.5259346975023,-6.43161333515741,
40.0894163708458));
#27990=CARTESIAN_POINT('Ctrl Pts',(-27.5231328183895,-6.41939631908899,
40.0867892506081));
#27991=CARTESIAN_POINT('Ctrl Pts',(-27.5201202176626,-6.40720563047245,
40.0843613974034));
#27992=CARTESIAN_POINT('Ctrl Pts',(-27.5156013165723,-6.38891959754764,
40.0807196175964));
#27993=CARTESIAN_POINT('Ctrl Pts',(-27.5106097081556,-6.37069173964469,
40.077526777822));
#27994=CARTESIAN_POINT('Ctrl Pts',(-27.5050448441814,-6.35256977567836,
40.0748589437388));
#27995=CARTESIAN_POINT('Ctrl Pts',(-27.5022624121943,-6.34350879369519,
40.0735250266972));
#27996=CARTESIAN_POINT('Ctrl Pts',(-27.4993360567762,-6.3344747311239,40.0723220518095));
#27997=CARTESIAN_POINT('Ctrl Pts',(-27.4962499309249,-6.32547111501694,
40.0712411903706));
#27998=CARTESIAN_POINT('Ctrl Pts',(-27.4947068679993,-6.32096930696347,
40.0707007596512));
#27999=CARTESIAN_POINT('Ctrl Pts',(-27.4931242188518,-6.31647639530748,
40.0701968069396));
#28000=CARTESIAN_POINT('Ctrl Pts',(-27.4914999811189,-6.31199416056962,
40.0697321796178));
#28001=CARTESIAN_POINT('Ctrl Pts',(-27.4898757433861,-6.30751192583176,
40.0692675522959));
#28002=CARTESIAN_POINT('Ctrl Pts',(-27.4882099136517,-6.3030403651958,40.0688422470209));
#28003=CARTESIAN_POINT('Ctrl Pts',(-27.4865003722782,-6.29858154433863,
40.0684588731157));
#28004=CARTESIAN_POINT('Ctrl Pts',(-27.4812555102352,-6.2849019103541,40.0672826844169));
#28005=CARTESIAN_POINT('Ctrl Pts',(-27.4755856598104,-6.27129040223665,
40.0664392906386));
#28006=CARTESIAN_POINT('Ctrl Pts',(-27.4694214423627,-6.25784359490804,
40.066081345996));
#28007=CARTESIAN_POINT('Ctrl Pts',(-27.4646998272645,-6.24754372326264,
40.0658071705887));
#28008=CARTESIAN_POINT('Ctrl Pts',(-27.4596665735312,-6.23735861368961,
40.0658422436823));
#28009=CARTESIAN_POINT('Ctrl Pts',(-27.4543102127987,-6.22740455152369,
40.0662584421382));
#28010=CARTESIAN_POINT('Ctrl Pts',(-27.4527665554702,-6.22453587598482,
40.0663783869717));
#28011=CARTESIAN_POINT('Ctrl Pts',(-27.4511949994592,-6.22168470670841,
40.0665304608586));
#28012=CARTESIAN_POINT('Ctrl Pts',(-27.4495943793826,-6.21885307551209,
40.0667167522398));
#28013=CARTESIAN_POINT('Ctrl Pts',(-27.4481938368156,-6.21637539821531,
40.0668797571984));
#28014=CARTESIAN_POINT('Ctrl Pts',(-27.4467710395402,-6.21391268023894,
40.0670689603025));
#28015=CARTESIAN_POINT('Ctrl Pts',(-27.4453250889059,-6.21146633976482,
40.067285741892));
#28016=CARTESIAN_POINT('Ctrl Pts',(-27.4402642616859,-6.20290414810542,
40.0680444774551));
#28017=CARTESIAN_POINT('Ctrl Pts',(-27.4349211443523,-6.19454160457023,
40.0691416007559));
#28018=CARTESIAN_POINT('Ctrl Pts',(-27.4292461252709,-6.18644670649284,
40.0706326389343));
#28019=CARTESIAN_POINT('Ctrl Pts',(-27.4242153245159,-6.17927072720969,
40.071954417044));
#28020=CARTESIAN_POINT('Ctrl Pts',(-27.4189234410945,-6.17230552110677,
40.0735870072275));
#28021=CARTESIAN_POINT('Ctrl Pts',(-27.4133244598885,-6.16560802962263,
40.0755585967453));
#28022=CARTESIAN_POINT('Ctrl Pts',(-27.4126074833121,-6.16475038350129,
40.0758110683023));
#28023=CARTESIAN_POINT('Ctrl Pts',(-27.4118854594803,-6.16389718068686,
40.0760691435545));
#28024=CARTESIAN_POINT('Ctrl Pts',(-27.4111582810183,-6.16304859028229,
40.076332922034));
#28025=CARTESIAN_POINT('Ctrl Pts',(-27.4069748832889,-6.15816671965832,
40.0778504178759));
#28026=CARTESIAN_POINT('Ctrl Pts',(-27.4026608751707,-6.15349535409897,
40.0795623732513));
#28027=CARTESIAN_POINT('Ctrl Pts',(-27.3982171490606,-6.14908120561047,
40.0814822596477));
#28028=CARTESIAN_POINT('Ctrl Pts',(-27.3965507517694,-6.14742589992728,
40.0822022170464));
#28029=CARTESIAN_POINT('Ctrl Pts',(-27.3948661088259,-6.14580677580884,
40.0829514055659));
#28030=CARTESIAN_POINT('Ctrl Pts',(-27.3931632535548,-6.14422633871427,
40.0837304977834));
#28031=CARTESIAN_POINT('Ctrl Pts',(-27.3924182543737,-6.14353489748539,
40.0840713506286));
#28032=CARTESIAN_POINT('Ctrl Pts',(-27.3916697692507,-6.14285086162515,
40.0844179267829));
#28033=CARTESIAN_POINT('Ctrl Pts',(-27.3909177948451,-6.14217440627914,
40.0847702338091));
#28034=CARTESIAN_POINT('Ctrl Pts',(-27.3904681928918,-6.1417699568157,40.0849808765197));
#28035=CARTESIAN_POINT('Ctrl Pts',(-27.3900173479083,-6.14136823954849,
40.0851935954983));
#28036=CARTESIAN_POINT('Ctrl Pts',(-27.3895652685859,-6.14096928576893,
40.0854083644669));
#28037=CARTESIAN_POINT('Ctrl Pts',(-27.3885996268668,-6.14011712024289,
40.08586711112));
#28038=CARTESIAN_POINT('Ctrl Pts',(-27.3876280770951,-6.13927790427025,
40.0863355648906));
#28039=CARTESIAN_POINT('Ctrl Pts',(-27.3866507863317,-6.13845171955947,
40.0868133190215));
#28040=CARTESIAN_POINT('Ctrl Pts',(-27.3794850171849,-6.13239390224247,
40.0903163458986));
#28041=CARTESIAN_POINT('Ctrl Pts',(-27.3720142576261,-6.12704603863401,
40.09433138839));
#28042=CARTESIAN_POINT('Ctrl Pts',(-27.3642632539306,-6.12254522320978,
40.0989235304305));
#28043=CARTESIAN_POINT('Ctrl Pts',(-27.3611502082718,-6.12073755487833,
40.1007678783891));
#28044=CARTESIAN_POINT('Ctrl Pts',(-27.3579921867464,-6.1190670360301,40.1027052304882));
#28045=CARTESIAN_POINT('Ctrl Pts',(-27.3547919380345,-6.11754464002831,
40.1047394416188));
#28046=CARTESIAN_POINT('Ctrl Pts',(-27.3534952922802,-6.11692781037227,
40.105563643568));
#28047=CARTESIAN_POINT('Ctrl Pts',(-27.3521978688196,-6.11633884284223,
40.1064006970497));
#28048=CARTESIAN_POINT('Ctrl Pts',(-27.3509000135422,-6.11577753018269,
40.1072500513475));
#28049=CARTESIAN_POINT('Ctrl Pts',(-27.3496832742196,-6.11525129956437,
40.1080463210017));
#28050=CARTESIAN_POINT('Ctrl Pts',(-27.3484661554654,-6.1147493750158,40.1088534018512));
#28051=CARTESIAN_POINT('Ctrl Pts',(-27.3472489508901,-6.11427158462743,
40.109670838332));
#28052=CARTESIAN_POINT('Ctrl Pts',(-27.3388812462172,-6.11098700211233,
40.1152903267884));
#28053=CARTESIAN_POINT('Ctrl Pts',(-27.3305072396875,-6.10884307366972,
40.1213990974306));
#28054=CARTESIAN_POINT('Ctrl Pts',(-27.322235046933,-6.10778191357492,40.1278491871424));
#28055=CARTESIAN_POINT('Ctrl Pts',(-27.3214824073746,-6.10768536468047,
40.1284360439549));
#28056=CARTESIAN_POINT('Ctrl Pts',(-27.3207305910292,-6.10759774950087,
40.12902573023));
#28057=CARTESIAN_POINT('Ctrl Pts',(-27.319979666939,-6.10751900703753,40.1296181367441));
#28058=CARTESIAN_POINT('Ctrl Pts',(-27.3122365353699,-6.10670705645327,
40.1357267190111));
#28059=CARTESIAN_POINT('Ctrl Pts',(-27.3045906547513,-6.1068415622247,40.1421229193531));
#28060=CARTESIAN_POINT('Ctrl Pts',(-27.2971463985059,-6.10786410630554,
40.1486937142711));
#28061=CARTESIAN_POINT('Ctrl Pts',(-27.2959339458739,-6.10803064896894,
40.1497639054803));
#28062=CARTESIAN_POINT('Ctrl Pts',(-27.2947268094371,-6.10822064294905,
40.1508387079977));
#28063=CARTESIAN_POINT('Ctrl Pts',(-27.2935253998823,-6.10843371318469,
40.1519176123711));
#28064=CARTESIAN_POINT('Origin',(-27.8490907775129,-12.8919045823054,40.036547827824));
#28065=CARTESIAN_POINT('Origin',(-27.8490907775129,-12.8919045823054,40.036547827824));
#28066=CARTESIAN_POINT('Origin',(-14.7107907121785,-13.5169045823054,-4.79600242588633));
#28067=CARTESIAN_POINT('Origin',(-31.3912427907138,-13.5169045823054,45.7890602015826));
#28068=CARTESIAN_POINT('Ctrl Pts',(-31.9675858640834,-14.6836564585996,
47.3436397133837));
#28069=CARTESIAN_POINT('Ctrl Pts',(-32.1960990859602,-14.7195047625521,
47.2319833969137));
#28070=CARTESIAN_POINT('Ctrl Pts',(-32.140341712633,-14.9046273277204,47.0628938417614));
#28071=CARTESIAN_POINT('Ctrl Pts',(-31.8173108281339,-14.2208393515118,
46.8863441102177));
#28072=CARTESIAN_POINT('Ctrl Pts',(-32.0453894454383,-14.2572370951476,
46.7749420308703));
#28073=CARTESIAN_POINT('Ctrl Pts',(-31.9896429860821,-14.4418102212184,
46.6058855733665));
#28074=CARTESIAN_POINT('Ctrl Pts',(-31.6669720145896,-13.7582547217136,
46.4288175299242));
#28075=CARTESIAN_POINT('Ctrl Pts',(-31.8945090807232,-13.7949155819404,
46.3173829274235));
#28076=CARTESIAN_POINT('Ctrl Pts',(-31.8388709365124,-13.9792255914427,
46.1486549459201));
#28077=CARTESIAN_POINT('Ctrl Pts',(-31.5165682646526,-13.2959337131846,
45.9710537470232));
#28078=CARTESIAN_POINT('Ctrl Pts',(-31.7434417477461,-13.3325299785125,
45.8592568248438));
#28079=CARTESIAN_POINT('Ctrl Pts',(-31.6880237676519,-13.5169045823054,
45.6911965120564));
#28080=CARTESIAN_POINT('Origin',(-31.3912427907138,-13.5169045823054,45.7890602015826));
#28081=CARTESIAN_POINT('Ctrl Pts',(-27.4498900633667,-6.28105857414855,
39.8238138910649));
#28082=CARTESIAN_POINT('Ctrl Pts',(-27.5054686557226,-6.09633085020216,
39.9923612758618));
#28083=CARTESIAN_POINT('Ctrl Pts',(-27.2778197979418,-6.06008770502775,
40.1040929402346));
#28084=CARTESIAN_POINT('Ctrl Pts',(-28.1663303157565,-8.47898077425032,
41.9964873213379));
#28085=CARTESIAN_POINT('Ctrl Pts',(-28.2252224962987,-8.30110493968633,
42.1750834784584));
#28086=CARTESIAN_POINT('Ctrl Pts',(-27.9918605627639,-8.25800948639314,
42.2784063052523));
#28087=CARTESIAN_POINT('Ctrl Pts',(-28.8808461149493,-10.6833293750548,
44.1633246636541));
#28088=CARTESIAN_POINT('Ctrl Pts',(-28.9397014588684,-10.5025148294221,
44.3418091102154));
#28089=CARTESIAN_POINT('Ctrl Pts',(-28.7042756097382,-10.4623581523752,
44.4466133273737));
#28090=CARTESIAN_POINT('Ctrl Pts',(-29.5940549924842,-12.8919045823054,
46.326198641332));
#28091=CARTESIAN_POINT('Ctrl Pts',(-29.651286959495,-12.7034528674627,46.49976004254));
#28092=CARTESIAN_POINT('Ctrl Pts',(-29.4155943178386,-12.6709337131846,
46.6106860996161));
#28093=CARTESIAN_POINT('Origin',(-29.2972740155461,-12.8919045823054,46.4240623308582));
#28094=CARTESIAN_POINT('Origin',(-13.2268858274881,-12.8919045823054,-4.30668397825546));
#28095=CARTESIAN_POINT('Ctrl Pts',(-30.04271957779,-13.2044045823055,46.6889364873753));
#28096=CARTESIAN_POINT('Ctrl Pts',(-30.0368201694537,-13.2044045823055,
46.695006276046));
#28097=CARTESIAN_POINT('Ctrl Pts',(-30.0305178990863,-13.20411637619,46.7007234861797));
#28098=CARTESIAN_POINT('Ctrl Pts',(-30.0238719237597,-13.2035045918484,
46.705933998298));
#28099=CARTESIAN_POINT('Ctrl Pts',(-30.0222118579831,-13.2033517772203,
46.707235506718));
#28100=CARTESIAN_POINT('Ctrl Pts',(-30.0205305478229,-13.2031788924169,
46.7085055118816));
#28101=CARTESIAN_POINT('Ctrl Pts',(-30.0188292749668,-13.2029856357525,
46.7097419077627));
#28102=CARTESIAN_POINT('Ctrl Pts',(-30.0145102056262,-13.2024950096128,
46.7128807808267));
#28103=CARTESIAN_POINT('Ctrl Pts',(-30.0100623794942,-13.2018727723585,
46.7158023935072));
#28104=CARTESIAN_POINT('Ctrl Pts',(-30.0055133346289,-13.2011172816476,
46.7184855719865));
#28105=CARTESIAN_POINT('Ctrl Pts',(-29.998689767331,-13.1999840455812,46.7225103397054));
#28106=CARTESIAN_POINT('Ctrl Pts',(-29.9916496764111,-13.1985506728398,
46.726024129218));
#28107=CARTESIAN_POINT('Ctrl Pts',(-29.9844563032259,-13.1968266777137,
46.7289158118595));
#28108=CARTESIAN_POINT('Ctrl Pts',(-29.9808596166333,-13.1959646801506,
46.7303616531803));
#28109=CARTESIAN_POINT('Ctrl Pts',(-29.9772246319322,-13.195030319004,46.731651963405));
#28110=CARTESIAN_POINT('Ctrl Pts',(-29.9735596330734,-13.1940263590679,
46.7327754786219));
#28111=CARTESIAN_POINT('Ctrl Pts',(-29.971727133644,-13.1935243790998,46.7333372362304));
#28112=CARTESIAN_POINT('Ctrl Pts',(-29.9698871192629,-13.1930050138329,
46.7338572987164));
#28113=CARTESIAN_POINT('Ctrl Pts',(-29.9680405503598,-13.1924686892783,
46.7343342824294));
#28114=CARTESIAN_POINT('Ctrl Pts',(-29.9675789081341,-13.1923346081396,
46.7344535283577));
#28115=CARTESIAN_POINT('Ctrl Pts',(-29.9671168559859,-13.1921994672886,
46.7345700819503));
#28116=CARTESIAN_POINT('Ctrl Pts',(-29.9666544083826,-13.1920632738588,
46.7346839217674));
#28117=CARTESIAN_POINT('Ctrl Pts',(-29.9652670655729,-13.1916546935696,
46.7350254412186));
#28118=CARTESIAN_POINT('Ctrl Pts',(-29.9638761650542,-13.1912366390105,
46.7353425362126));
#28119=CARTESIAN_POINT('Ctrl Pts',(-29.9624820851714,-13.1908093125307,
46.7356346320705));
#28120=CARTESIAN_POINT('Ctrl Pts',(-29.954042205835,-13.188222241323,46.7374030054799));
#28121=CARTESIAN_POINT('Ctrl Pts',(-29.9455363271605,-13.1853020171008,
46.738319884669));
#28122=CARTESIAN_POINT('Ctrl Pts',(-29.9370870977222,-13.1821047274604,
46.7384633004647));
#28123=CARTESIAN_POINT('Ctrl Pts',(-29.9307220034064,-13.1796960995182,
46.7385713405022));
#28124=CARTESIAN_POINT('Ctrl Pts',(-29.924388757318,-13.1771305701858,46.7382414915082));
#28125=CARTESIAN_POINT('Ctrl Pts',(-29.9181337478532,-13.1744346626403,
46.7375255006745));
#28126=CARTESIAN_POINT('Ctrl Pts',(-29.917223866056,-13.1740425038088,46.737421349429));
#28127=CARTESIAN_POINT('Ctrl Pts',(-29.9163156537632,-13.1736476854837,
46.7373084624657));
#28128=CARTESIAN_POINT('Ctrl Pts',(-29.9154092836977,-13.1732503241607,
46.7371869720081));
#28129=CARTESIAN_POINT('Ctrl Pts',(-29.9147043463233,-13.17294127286,46.7370924817249));
#28130=CARTESIAN_POINT('Ctrl Pts',(-29.9140001157073,-13.1726304994968,
46.7369927667443));
#28131=CARTESIAN_POINT('Ctrl Pts',(-29.9132966638191,-13.1723180491455,
46.7368878708566));
#28132=CARTESIAN_POINT('Ctrl Pts',(-29.9033263548421,-13.1678895635671,
46.7354011388876));
#28133=CARTESIAN_POINT('Ctrl Pts',(-29.8936167820225,-13.1631872663844,
46.7329350902098));
#28134=CARTESIAN_POINT('Ctrl Pts',(-29.8843259095194,-13.1583829057193,
46.7297748595837));
#28135=CARTESIAN_POINT('Ctrl Pts',(-29.8816299246712,-13.1569887973022,
46.7288578376483));
#28136=CARTESIAN_POINT('Ctrl Pts',(-29.8789690772141,-13.1555861806432,
46.7278826869499));
#28137=CARTESIAN_POINT('Ctrl Pts',(-29.8763469083833,-13.1541794056116,
46.7268570368218));
#28138=CARTESIAN_POINT('Ctrl Pts',(-29.867948476878,-13.1496737065098,46.723572026243));
#28139=CARTESIAN_POINT('Ctrl Pts',(-29.8598547091022,-13.1450668045687,
46.7197885306234));
#28140=CARTESIAN_POINT('Ctrl Pts',(-29.8520287057686,-13.1404003938699,
46.7155889038217));
#28141=CARTESIAN_POINT('Ctrl Pts',(-29.8476327076698,-13.137779192257,46.7132299025986));
#28142=CARTESIAN_POINT('Ctrl Pts',(-29.843321315133,-13.1351390520035,46.7107385600487));
#28143=CARTESIAN_POINT('Ctrl Pts',(-29.8390887268153,-13.1324866446614,
46.7081225206955));
#28144=CARTESIAN_POINT('Ctrl Pts',(-29.8346758466811,-13.1297212550724,
46.7053950482306));
#28145=CARTESIAN_POINT('Ctrl Pts',(-29.8303485053492,-13.1269417023507,
46.7025350007665));
#28146=CARTESIAN_POINT('Ctrl Pts',(-29.8261007325175,-13.1241525253868,
46.6995556323488));
#28147=CARTESIAN_POINT('Ctrl Pts',(-29.8242423319037,-13.122932260465,46.6982521586661));
#28148=CARTESIAN_POINT('Ctrl Pts',(-29.8223991720806,-13.1217101337094,
46.6969258426594));
#28149=CARTESIAN_POINT('Ctrl Pts',(-29.82057080665,-13.1204864412399,46.6955777768191));
#28150=CARTESIAN_POINT('Ctrl Pts',(-29.8188567140589,-13.1193392295498,
46.6943139650937));
#28151=CARTESIAN_POINT('Ctrl Pts',(-29.8171556245902,-13.1181906410734,
46.6930310372273));
#28152=CARTESIAN_POINT('Ctrl Pts',(-29.8154671982959,-13.117040885084,46.6917298843572));
#28153=CARTESIAN_POINT('Ctrl Pts',(-29.8051941573223,-13.1100453233422,
46.6838131652248));
#28154=CARTESIAN_POINT('Ctrl Pts',(-29.7953494354289,-13.1029809016301,
46.675192533093));
#28155=CARTESIAN_POINT('Ctrl Pts',(-29.7859484771511,-13.0959259298128,
46.6661148193062));
#28156=CARTESIAN_POINT('Ctrl Pts',(-29.7839183747256,-13.0944024345504,
46.6641545203418));
#28157=CARTESIAN_POINT('Ctrl Pts',(-29.7819089162172,-13.0928792536023,
46.6621727676645));
#28158=CARTESIAN_POINT('Ctrl Pts',(-29.7799201851399,-13.0913569710302,
46.6601718236165));
#28159=CARTESIAN_POINT('Ctrl Pts',(-29.7690104052807,-13.0830060341259,
46.6491950458494));
#28160=CARTESIAN_POINT('Ctrl Pts',(-29.7586608103041,-13.0746647314083,
46.6376540788201));
#28161=CARTESIAN_POINT('Ctrl Pts',(-29.7488108236965,-13.0663267356308,
46.6257713981828));
#28162=CARTESIAN_POINT('Ctrl Pts',(-29.748272514602,-13.0658710579598,46.6251220008477));
#28163=CARTESIAN_POINT('Ctrl Pts',(-29.7477357007175,-13.0654153808115,
46.6244715746663));
#28164=CARTESIAN_POINT('Ctrl Pts',(-29.7472003732994,-13.0649596999837,
46.6238201531363));
#28165=CARTESIAN_POINT('Ctrl Pts',(-29.7404781089958,-13.0592375814082,
46.6156400608235));
#28166=CARTESIAN_POINT('Ctrl Pts',(-29.7339925628948,-13.053534176996,46.6072713024434));
#28167=CARTESIAN_POINT('Ctrl Pts',(-29.7277161004611,-13.0478477661443,
46.598737203163));
#28168=CARTESIAN_POINT('Ctrl Pts',(-29.7170149824623,-13.0381526625477,
46.5841869044274));
#28169=CARTESIAN_POINT('Ctrl Pts',(-29.7069273852876,-13.0285130912561,
46.5691662228752));
#28170=CARTESIAN_POINT('Ctrl Pts',(-29.6973719426179,-13.0189444021978,
46.553797195801));
#28171=CARTESIAN_POINT('Ctrl Pts',(-29.6871702002742,-13.0087285175221,
46.5373886567408));
#28172=CARTESIAN_POINT('Ctrl Pts',(-29.6775748886097,-12.9985931561289,
46.5205824904044));
#28173=CARTESIAN_POINT('Ctrl Pts',(-29.6685050610264,-12.9885428112971,
46.503472020218));
#28174=CARTESIAN_POINT('Ctrl Pts',(-29.6583357622502,-12.9772741340857,
46.4842873684781));
#28175=CARTESIAN_POINT('Ctrl Pts',(-29.6488266209448,-12.9661119592019,
46.464719631505));
#28176=CARTESIAN_POINT('Ctrl Pts',(-29.6398905793283,-12.9550504724707,
46.4448415317008));
#28177=CARTESIAN_POINT('Ctrl Pts',(-29.6298393434875,-12.9426085416186,
46.4224826979162));
#28178=CARTESIAN_POINT('Ctrl Pts',(-29.6205123618971,-12.9302931192882,
46.3997297163687));
#28179=CARTESIAN_POINT('Ctrl Pts',(-29.6118286232292,-12.9180916100454,
46.376631896441));
#28180=CARTESIAN_POINT('Ctrl Pts',(-29.6055746337663,-12.9093041380643,
46.3599969505993));
#28181=CARTESIAN_POINT('Ctrl Pts',(-29.5996552034974,-12.9005755951523,
46.3431818156186));
#28182=CARTESIAN_POINT('Ctrl Pts',(-29.5940549924842,-12.8919045823054,
46.326198641332));
#28183=CARTESIAN_POINT('Origin',(-31.3912427907138,-13.5169045823054,45.7890602015826));
#28184=CARTESIAN_POINT('Origin',(-31.3912427907138,-13.5169045823054,45.7890602015826));
#28185=CARTESIAN_POINT('Ctrl Pts',(-30.1626755346769,-13.2959337131847,
46.8745131384049));
#28186=CARTESIAN_POINT('Ctrl Pts',(-30.1129881504469,-13.2044045823055,
46.7976447726886));
#28187=CARTESIAN_POINT('Ctrl Pts',(-30.04271957779,-13.2044045823055,46.6889364873753));
#28188=CARTESIAN_POINT('Ctrl Pts',(-30.08095390153,-13.2959337183951,46.927337660237));
#28189=CARTESIAN_POINT('Ctrl Pts',(-30.0567289927829,-13.209279823895,46.8398155271884));
#28190=CARTESIAN_POINT('Ctrl Pts',(-30.0057259985099,-13.2044045823055,
46.7269984752225));
#28191=CARTESIAN_POINT('Ctrl Pts',(-29.9887271578055,-13.2734166054794,
46.9598087435376));
#28192=CARTESIAN_POINT('Ctrl Pts',(-29.9896831552566,-13.193172351531,46.8638177887699));
#28193=CARTESIAN_POINT('Ctrl Pts',(-29.9601903592735,-13.1931460297457,
46.7438847747009));
#28194=CARTESIAN_POINT('Ctrl Pts',(-29.8139966334862,-13.1901047283844,
46.9726654864714));
#28195=CARTESIAN_POINT('Ctrl Pts',(-29.866204852841,-13.1260474868727,46.8633668402251));
#28196=CARTESIAN_POINT('Ctrl Pts',(-29.8664029441127,-13.1514900886124,
46.7298907631929));
#28197=CARTESIAN_POINT('Ctrl Pts',(-29.7351139893344,-13.1321577745916,
46.9541554619723));
#28198=CARTESIAN_POINT('Ctrl Pts',(-29.8115047075592,-13.0767072102091,
46.83982187418));
#28199=CARTESIAN_POINT('Ctrl Pts',(-29.8204272993462,-13.1225166214137,
46.700471501026));
#28200=CARTESIAN_POINT('Ctrl Pts',(-29.5397638152463,-12.9456232578403,
46.8572594916692));
#28201=CARTESIAN_POINT('Ctrl Pts',(-29.6836831453199,-12.917759331099,46.7330734174298));
#28202=CARTESIAN_POINT('Ctrl Pts',(-29.6989366770835,-13.0292493378237,
46.5791043383549));
#28203=CARTESIAN_POINT('Ctrl Pts',(-29.4578462161212,-12.8021218234312,
46.739230783511));
#28204=CARTESIAN_POINT('Ctrl Pts',(-29.649013231966,-12.7965826300655,46.6116445270736));
#28205=CARTESIAN_POINT('Ctrl Pts',(-29.6364065710858,-12.9574790903514,
46.4546338447575));
#28206=CARTESIAN_POINT('Ctrl Pts',(-29.4155943178386,-12.6709337131846,
46.6106860996161));
#28207=CARTESIAN_POINT('Ctrl Pts',(-29.6512869594949,-12.7034528674627,
46.49976004254));
#28208=CARTESIAN_POINT('Ctrl Pts',(-29.5940549924842,-12.8919045823054,
46.326198641332));
#28209=CARTESIAN_POINT('Origin',(-30.0427195777899,-13.5169045823054,46.6889364873753));
#28210=CARTESIAN_POINT('Origin',(0.0835265683620477,-13.5169045823054,0.0824317919394229));
#28211=CARTESIAN_POINT('Origin',(34.8549570309562,12.3739193162059,-36.4567656030545));
#28212=CARTESIAN_POINT('Origin',(34.5439318808757,11.9341984494201,-36.1457404735404));
#28213=CARTESIAN_POINT('Origin',(35.1659821576994,12.8136401876617,-36.7677907503641));
#28214=CARTESIAN_POINT('Origin',(34.5439318808757,11.9341984494201,-36.1457404735404));
#28215=CARTESIAN_POINT('Origin',(34.5439318808757,11.9341984494201,-36.1457404735404));
#28216=CARTESIAN_POINT('Origin',(35.1659821576994,12.8136401876617,-36.7677907503641));
#28217=CARTESIAN_POINT('Origin',(35.1659821576994,12.8136401876617,-36.7677907503641));
#28218=CARTESIAN_POINT('Origin',(35.1659821576994,12.8136401876617,-36.7677907503641));
#28219=CARTESIAN_POINT('Origin',(0.0835265683620477,11.9341984494201,0.0824317919394229));
#28220=CARTESIAN_POINT('Origin',(-34.3768787441515,11.9341984494201,-36.1457404735405));
#28221=CARTESIAN_POINT('Origin',(0.0835265683620477,12.8136401876617,0.0824317919394229));
#28222=CARTESIAN_POINT('Ctrl Pts',(11.0320394968432,13.1261401876617,-49.6050682080606));
#28223=CARTESIAN_POINT('Ctrl Pts',(10.6578693364404,13.1261401876617,-49.6453148766512));
#28224=CARTESIAN_POINT('Ctrl Pts',(10.2836734751494,13.1182694471953,-49.6836022760034));
#28225=CARTESIAN_POINT('Ctrl Pts',(9.90942930877251,13.1033923474057,-49.7199013138211));
#28226=CARTESIAN_POINT('Ctrl Pts',(9.90937195321906,13.1033900673854,-49.7199068769042));
#28227=CARTESIAN_POINT('Ctrl Pts',(9.90931459767862,13.1033877872104,-49.7199124399391));
#28228=CARTESIAN_POINT('Ctrl Pts',(9.90925724215118,13.1033855068806,-49.7199180029256));
#28229=CARTESIAN_POINT('Ctrl Pts',(9.69153210444253,13.0947292335987,-49.7410354449037));
#28230=CARTESIAN_POINT('Ctrl Pts',(9.47385022844805,13.0838402503218,-49.7614722083415));
#28231=CARTESIAN_POINT('Ctrl Pts',(9.25629353024675,13.069869045462,-49.7812208487346));
#28232=CARTESIAN_POINT('Ctrl Pts',(9.09983844834887,13.0598217059932,-49.7954230092547));
#28233=CARTESIAN_POINT('Ctrl Pts',(8.94344804305751,13.0481798478176,-49.8092691162915));
#28234=CARTESIAN_POINT('Ctrl Pts',(8.78715657141638,13.0346110567867,-49.8227532649998));
#28235=CARTESIAN_POINT('Origin',(24.5746430918789,12.8136401876617,-26.1764516845437));
#28236=CARTESIAN_POINT('Origin',(38.9743995336223,12.8136401876617,-40.5762081262869));
#28237=CARTESIAN_POINT('Origin',(34.5439318808757,-3.61941807409668,-36.1457404735404));
#28238=CARTESIAN_POINT('Origin',(34.5439318808757,-3.61941807409668,-36.1457404735404));
#28239=CARTESIAN_POINT('Origin',(34.5439318808757,-3.61941807409669,-36.1457404735404));
#28240=CARTESIAN_POINT('Origin',(-34.3768787441515,11.9341984494201,-36.1457404735405));
#28241=CARTESIAN_POINT('Origin',(-34.3768787441515,11.9341984494202,-36.1457404735405));
#28242=CARTESIAN_POINT('Ctrl Pts',(11.0320394968433,13.1261401876617,-49.6050682080606));
#28243=CARTESIAN_POINT('Ctrl Pts',(11.0320394968433,13.1261401876617,-49.9175682080606));
#28244=CARTESIAN_POINT('Ctrl Pts',(11.0320394968433,13.4386401876617,-49.9175682080606));
#28245=CARTESIAN_POINT('Ctrl Pts',(10.6584907317851,13.1261401876617,-49.6452480378299));
#28246=CARTESIAN_POINT('Ctrl Pts',(10.6809373469102,13.1639055963026,-49.9175682080606));
#28247=CARTESIAN_POINT('Ctrl Pts',(10.6496370560559,13.4386401851022,-49.9175682080606));
#28248=CARTESIAN_POINT('Ctrl Pts',(10.2842597524009,13.1182927286047,-49.6835453366231));
#28249=CARTESIAN_POINT('Ctrl Pts',(10.2980626523239,13.1821712224823,-49.9175682080606));
#28250=CARTESIAN_POINT('Ctrl Pts',(10.2678955540983,13.4229452699559,-49.9175682080606));
#28251=CARTESIAN_POINT('Ctrl Pts',(9.5345988672954,13.0884919386943,-49.7562572211741));
#28252=CARTESIAN_POINT('Ctrl Pts',(9.54083079601551,13.1804128114024,-49.9175682080606));
#28253=CARTESIAN_POINT('Ctrl Pts',(9.50565038581019,13.3633436893187,-49.9175682080606));
#28254=CARTESIAN_POINT('Ctrl Pts',(9.15977276126021,13.0669605544565,-49.7906055560521));
#28255=CARTESIAN_POINT('Ctrl Pts',(9.1588613746445,13.1642472289417,-49.9175682080606));
#28256=CARTESIAN_POINT('Ctrl Pts',(9.12568496896286,13.3202672259815,-49.9175682080606));
#28257=CARTESIAN_POINT('Ctrl Pts',(8.78715657141589,13.0346110567867,-49.8227532649998));
#28258=CARTESIAN_POINT('Ctrl Pts',(8.77156878298277,13.125337974864,-49.9175682080606));
#28259=CARTESIAN_POINT('Ctrl Pts',(8.74919157457976,13.2555819259088,-49.9175682080606));
#28260=CARTESIAN_POINT('Origin',(11.0320394968432,13.4386401876617,-49.6050682080606));
#28261=CARTESIAN_POINT('Origin',(8.7491915745805,13.2555819259033,-49.6050682080606));
#28262=CARTESIAN_POINT('Origin',(39.8582830101055,12.8136401876617,-39.6923246498037));
#28263=CARTESIAN_POINT('Origin',(40.7421664865887,12.8136401876617,-38.8084411733206));
#28264=CARTESIAN_POINT('Ctrl Pts',(38.0393490816115,-8.24885981233825,-39.1992159360345));
#28265=CARTESIAN_POINT('Ctrl Pts',(37.8856271521298,-8.46631238203733,-39.0454940065529));
#28266=CARTESIAN_POINT('Ctrl Pts',(37.6657443451358,-8.46983068145904,-39.2604024894786));
#28267=CARTESIAN_POINT('Ctrl Pts',(36.9478802019249,-6.70569384849427,-38.1077470563479));
#28268=CARTESIAN_POINT('Ctrl Pts',(36.7944751038544,-6.92339564386804,-37.954341958285));
#28269=CARTESIAN_POINT('Ctrl Pts',(36.5743787698635,-6.92666471828378,-38.1688349292337));
#28270=CARTESIAN_POINT('Ctrl Pts',(35.8563993091448,-5.16254485803399,-37.0162661635679));
#28271=CARTESIAN_POINT('Ctrl Pts',(35.7031187964695,-5.38020745679319,-36.8629856508092));
#28272=CARTESIAN_POINT('Ctrl Pts',(35.483009954652,-5.38351572788346,-37.0772471608648));
#28273=CARTESIAN_POINT('Ctrl Pts',(34.7649027499965,-3.61941807409668,-35.9247696044196));
#28274=CARTESIAN_POINT('Ctrl Pts',(34.6114148933597,-3.83655054711529,-35.7712817477828));
#28275=CARTESIAN_POINT('Ctrl Pts',(34.3916369666325,-3.84038894321747,-35.9856330592972));
#28276=CARTESIAN_POINT('Origin',(37.8183782124907,-8.24885981233827,-39.4201868051553));
#28277=CARTESIAN_POINT('Origin',(0.0835265683620477,-3.61941807409668,0.0824317919394229));
#28278=CARTESIAN_POINT('Origin',(-34.3768787441515,-3.61941807409668,-36.1457404735405));
#28279=CARTESIAN_POINT('Origin',(-34.6879044362409,12.3739187291536,-36.4567658910079));
#28280=CARTESIAN_POINT('Origin',(-34.9989290209752,12.8136401876617,-36.7677907503642));
#28281=CARTESIAN_POINT('Origin',(0.0835265683620477,12.8136401876617,0.0824317919394229));
#28282=CARTESIAN_POINT('Ctrl Pts',(-8.62010343469281,13.0346110567825,-49.8227532650011));
#28283=CARTESIAN_POINT('Ctrl Pts',(-8.88131178011465,13.0572884390954,-49.8002173445413));
#28284=CARTESIAN_POINT('Ctrl Pts',(-9.14274668539152,13.0745923805386,-49.7766769038922));
#28285=CARTESIAN_POINT('Ctrl Pts',(-9.40431840153695,13.0880420718507,-49.7521473008839));
#28286=CARTESIAN_POINT('Ctrl Pts',(-9.51689874960235,13.0938308128951,-49.7415897708677));
#28287=CARTESIAN_POINT('Ctrl Pts',(-9.62950455408787,13.0989048482899,-49.7308488985899));
#28288=CARTESIAN_POINT('Ctrl Pts',(-9.74212903364439,13.1033825850677,-49.7199254399034));
#28289=CARTESIAN_POINT('Ctrl Pts',(-9.74242935783179,13.1033945253906,-49.7198963114327));
#28290=CARTESIAN_POINT('Ctrl Pts',(-9.7427296825782,13.1034064614895,-49.7198671816217));
#28291=CARTESIAN_POINT('Ctrl Pts',(-9.74303000788388,13.1034183933665,-49.7198380504703));
#28292=CARTESIAN_POINT('Ctrl Pts',(-9.98721127321016,13.1131196764878,-49.6961527956236));
#28293=CARTESIAN_POINT('Ctrl Pts',(-10.2314035286019,13.1198333629236,-49.6716164060401));
#28294=CARTESIAN_POINT('Ctrl Pts',(-10.4755740809779,13.1233309724858,-49.6462439593173));
#28295=CARTESIAN_POINT('Ctrl Pts',(-10.6053869203596,13.1251904703815,-49.6327547431972));
#28296=CARTESIAN_POINT('Ctrl Pts',(-10.7351934140452,13.1261401876617,-49.6190290586065));
#28297=CARTESIAN_POINT('Ctrl Pts',(-10.8649863601192,13.1261401876617,-49.6050682080606));
#28298=CARTESIAN_POINT('Origin',(-34.9989290209752,12.8136401876617,-36.7677907503642));
#28299=CARTESIAN_POINT('Ctrl Pts',(8.78715657141686,13.0346110567825,-49.8227532650012));
#28300=CARTESIAN_POINT('Ctrl Pts',(8.77156878298359,13.1253379748597,-49.9175682080606));
#28301=CARTESIAN_POINT('Ctrl Pts',(8.7491915745805,13.2555819259033,-49.9175682080606));
#28302=CARTESIAN_POINT('Ctrl Pts',(5.9167136340953,12.5435283274364,-49.8248727468205));
#28303=CARTESIAN_POINT('Ctrl Pts',(5.91175753908113,12.6357570952065,-49.9175682080606));
#28304=CARTESIAN_POINT('Ctrl Pts',(5.89089499049724,12.7644980954123,-49.9175682080606));
#28305=CARTESIAN_POINT('Ctrl Pts',(3.02011116462985,12.2852858973025,-49.8260360759873));
#28306=CARTESIAN_POINT('Ctrl Pts',(3.01473384245429,12.3768143018313,-49.9175682080606));
#28307=CARTESIAN_POINT('Ctrl Pts',(3.00710937180082,12.5062567663872,-49.9175682080606));
#28308=CARTESIAN_POINT('Ctrl Pts',(-1.36745139963336,12.2842756298963,-49.8260405689135));
#28309=CARTESIAN_POINT('Ctrl Pts',(-1.36478834461974,12.3758051232163,-49.9175682080606));
#28310=CARTESIAN_POINT('Ctrl Pts',(-1.36102716280008,12.5052464990352,-49.9175682080606));
#28311=CARTESIAN_POINT('Ctrl Pts',(-2.84134992071046,12.3489547591764,-49.8257518757999));
#28312=CARTESIAN_POINT('Ctrl Pts',(-2.83674726276666,12.4404805872018,-49.9175682080606));
#28313=CARTESIAN_POINT('Ctrl Pts',(-2.82840051213665,12.5699256283378,-49.9175682080606));
#28314=CARTESIAN_POINT('Ctrl Pts',(-5.75032001544249,12.6021248598315,-49.8246345776219));
#28315=CARTESIAN_POINT('Ctrl Pts',(-5.74047966090505,12.6933787936176,-49.9175682080606));
#28316=CARTESIAN_POINT('Ctrl Pts',(-5.72463777045536,12.8230957289117,-49.9175682080606));
#28317=CARTESIAN_POINT('Ctrl Pts',(-7.19139408987476,12.7901838029064,-49.8238081974504));
#28318=CARTESIAN_POINT('Ctrl Pts',(-7.17966289645425,12.8814125534473,-49.9175682080606));
#28319=CARTESIAN_POINT('Ctrl Pts',(-7.15947736247938,13.0111545790442,-49.9175682080606));
#28320=CARTESIAN_POINT('Ctrl Pts',(-8.62010343469281,13.0346110567825,-49.8227532650012));
#28321=CARTESIAN_POINT('Ctrl Pts',(-8.60451564625954,13.1253379748597,-49.9175682080606));
#28322=CARTESIAN_POINT('Ctrl Pts',(-8.58213843785645,13.2555819259033,-49.9175682080606));
#28323=CARTESIAN_POINT('Origin',(-8.58213843785645,13.2555819259033,-49.6050682080606));
#28324=CARTESIAN_POINT('Origin',(0.0835265683620477,13.4386401876617,-49.6050682080606));
#28325=CARTESIAN_POINT('Origin',(44.4585265683622,13.4386401876617,-49.6050682080606));
#28326=CARTESIAN_POINT('Origin',(26.3424100448454,12.8136401876617,-24.4086847315773));
#28327=CARTESIAN_POINT('Origin',(36.9337491106658,12.8136401876617,-35.0000237973977));
#28328=CARTESIAN_POINT('Origin',(37.8183782124907,-8.24885981233827,-39.4201868051553));
#28329=CARTESIAN_POINT('Origin',(37.8183782124907,-8.24885981233827,-39.4201868051553));
#28330=CARTESIAN_POINT('Origin',(37.8183782124907,-8.24885981233827,-39.4201868051553));
#28331=CARTESIAN_POINT('Origin',(-34.3768787441515,-3.61941807409668,-36.1457404735405));
#28332=CARTESIAN_POINT('Origin',(-34.3768787441515,-3.61941807409668,-36.1457404735405));
#28333=CARTESIAN_POINT('Origin',(-34.9989290209752,12.8136401876617,-36.7677907503642));
#28334=CARTESIAN_POINT('Origin',(-34.9989290209752,12.8136401876617,-36.7677907503642));
#28335=CARTESIAN_POINT('Ctrl Pts',(-8.6201034346928,13.0346110567825,-49.8227532650011));
#28336=CARTESIAN_POINT('Ctrl Pts',(-8.60451564625953,13.1253379748597,-49.9175682080606));
#28337=CARTESIAN_POINT('Ctrl Pts',(-8.58213843785645,13.2555819259033,-49.9175682080606));
#28338=CARTESIAN_POINT('Ctrl Pts',(-8.99338683221866,13.0670184804062,-49.7905479931254));
#28339=CARTESIAN_POINT('Ctrl Pts',(-8.99252376979541,13.1643191174805,-49.9175682080606));
#28340=CARTESIAN_POINT('Ctrl Pts',(-8.95930452222033,13.3203828042395,-49.9175682080606));
#28341=CARTESIAN_POINT('Ctrl Pts',(-9.36803051056639,13.0885197051924,-49.756212524541));
#28342=CARTESIAN_POINT('Ctrl Pts',(-9.37428367693385,13.1804336598308,-49.9175682080606));
#28343=CARTESIAN_POINT('Ctrl Pts',(-9.33908873922842,13.3633992223637,-49.9175682080606));
#28344=CARTESIAN_POINT('Ctrl Pts',(-10.1180295169891,13.1183169307001,-49.6834631932219));
#28345=CARTESIAN_POINT('Ctrl Pts',(-10.1318579424303,13.1821517325912,-49.9175682080606));
#28346=CARTESIAN_POINT('Ctrl Pts',(-10.1016805625987,13.4229936740979,-49.9175682080606));
#28347=CARTESIAN_POINT('Ctrl Pts',(-10.4925362263167,13.1261401876617,-49.6451298663487));
#28348=CARTESIAN_POINT('Ctrl Pts',(-10.5148588400716,13.1638007628797,-49.9175682080606));
#28349=CARTESIAN_POINT('Ctrl Pts',(-10.4837073054091,13.4386401852138,-49.9175682080606));
#28350=CARTESIAN_POINT('Ctrl Pts',(-10.8649863601192,13.1261401876617,-49.6050682080606));
#28351=CARTESIAN_POINT('Ctrl Pts',(-10.8649863601192,13.1261401876617,-49.9175682080606));
#28352=CARTESIAN_POINT('Ctrl Pts',(-10.8649863601192,13.4386401876617,-49.9175682080606));
#28353=CARTESIAN_POINT('Origin',(-10.8649863601192,13.4386401876617,-49.6050682080606));
#28354=CARTESIAN_POINT('Origin',(44.4585265683622,13.4386401876617,-44.2925682080604));
#28355=CARTESIAN_POINT('Origin',(49.7710265683622,13.4386401876617,-44.2925682080604));
#28356=CARTESIAN_POINT('Origin',(36.9337491106658,12.8136401876617,-35.0000237973977));
#28357=CARTESIAN_POINT('Origin',(36.9337491106658,12.8136401876617,-35.0000237973977));
#28358=CARTESIAN_POINT('Origin',(36.9337491106658,12.8136401876617,-35.0000237973977));
#28359=CARTESIAN_POINT('Origin',(39.6373121409847,-8.24885981233827,-41.2391207336493));
#28360=CARTESIAN_POINT('Origin',(0.0835265683620477,-8.24885981233827,0.0824317919394229));
#28361=CARTESIAN_POINT('Ctrl Pts',(21.7919948253812,-8.46983068146548,-49.8076885551764));
#28362=CARTESIAN_POINT('Ctrl Pts',(21.8521423242108,-8.48281912914163,-49.7956815989318));
#28363=CARTESIAN_POINT('Ctrl Pts',(21.9125265915097,-8.49383985404005,-49.7835868143488));
#28364=CARTESIAN_POINT('Ctrl Pts',(21.9730858028217,-8.50331222135622,-49.7714165769901));
#28365=CARTESIAN_POINT('Ctrl Pts',(22.0387999717056,-8.51359090121448,-49.7582103773745));
#28366=CARTESIAN_POINT('Ctrl Pts',(22.1047202451555,-8.52204613529236,-49.7449153215987));
#28367=CARTESIAN_POINT('Ctrl Pts',(22.1707904779483,-8.52915470826165,-49.7315420543742));
#28368=CARTESIAN_POINT('Ctrl Pts',(22.2084677088732,-8.53320844523197,-49.7239158109641));
#28369=CARTESIAN_POINT('Ctrl Pts',(22.2461941051687,-8.53682321976947,-49.7162640419939));
#28370=CARTESIAN_POINT('Ctrl Pts',(22.2839618928278,-8.54008060317762,-49.7085880973647));
#28371=CARTESIAN_POINT('Ctrl Pts',(22.2853194127144,-8.54019768609481,-49.7083121943232));
#28372=CARTESIAN_POINT('Ctrl Pts',(22.2866770266266,-8.54031425987122,-49.7080362514587));
#28373=CARTESIAN_POINT('Ctrl Pts',(22.2880347319652,-8.54043032524655,-49.7077602693195));
#28374=CARTESIAN_POINT('Ctrl Pts',(22.3534462848796,-8.54602212504614,-49.6944639967121));
#28375=CARTESIAN_POINT('Ctrl Pts',(22.4189815616388,-8.55043067995687,-49.681094851513));
#28376=CARTESIAN_POINT('Ctrl Pts',(22.4845845014327,-8.55374151002609,-49.667665924648));
#28377=CARTESIAN_POINT('Ctrl Pts',(22.550095188687,-8.55704768432099,-49.6542558818851));
#28378=CARTESIAN_POINT('Ctrl Pts',(22.6156761216241,-8.55925889971346,-49.6407856528723));
#28379=CARTESIAN_POINT('Ctrl Pts',(22.6812748008842,-8.56041391612642,-49.6272656412831));
#28380=CARTESIAN_POINT('Ctrl Pts',(22.7171068924841,-8.56104482294307,-49.6198805795844));
#28381=CARTESIAN_POINT('Ctrl Pts',(22.7529440968362,-8.56135981233827,-49.6124806680525));
#28382=CARTESIAN_POINT('Ctrl Pts',(22.7887737236329,-8.56135981233827,-49.6050682080606));
#28383=CARTESIAN_POINT('Ctrl Pts',(-37.4986912084115,-8.46983068145905,
-39.2604024894787));
#28384=CARTESIAN_POINT('Ctrl Pts',(-37.7185740154056,-8.46631238203734,
-39.045494006553));
#28385=CARTESIAN_POINT('Ctrl Pts',(-37.8722959448872,-8.24885981233825,
-39.1992159360346));
#28386=CARTESIAN_POINT('Ctrl Pts',(-36.4073256331548,-6.92666471828356,
-38.1688349292187));
#28387=CARTESIAN_POINT('Ctrl Pts',(-36.6274219671529,-6.92339564385727,
-37.9543419582776));
#28388=CARTESIAN_POINT('Ctrl Pts',(-36.7808270652083,-6.7056938484836,-38.1077470563557));
#28389=CARTESIAN_POINT('Ctrl Pts',(-35.3159568179087,-5.38351572788376,
-37.0772471608834));
#28390=CARTESIAN_POINT('Ctrl Pts',(-35.5360656597061,-5.38020745678442,
-36.8629856508611));
#28391=CARTESIAN_POINT('Ctrl Pts',(-35.6893461724156,-5.16254485804107,
-37.016266163563));
#28392=CARTESIAN_POINT('Ctrl Pts',(-34.2245838299083,-3.84038894321748,
-35.9856330592973));
#28393=CARTESIAN_POINT('Ctrl Pts',(-34.4443617566355,-3.83655054711529,
-35.7712817477829));
#28394=CARTESIAN_POINT('Ctrl Pts',(-34.5978496132723,-3.61941807409668,
-35.9247696044197));
#28395=CARTESIAN_POINT('Origin',(-37.6513250757665,-8.24885981233827,-39.4201868051554));
#28396=CARTESIAN_POINT('Origin',(-24.4075899551548,12.8136401876617,-26.1764516845438));
#28397=CARTESIAN_POINT('Origin',(-38.8073463968981,12.8136401876617,-40.576208126287));
#28398=CARTESIAN_POINT('Origin',(0.0835265683620477,13.4386401876617,-49.6050682080606));
#28399=CARTESIAN_POINT('Origin',(-44.2914734316379,13.4386401876617,-49.6050682080606));
#28400=CARTESIAN_POINT('Origin',(49.7710265683621,13.4386401876617,0.0824317919395964));
#28401=CARTESIAN_POINT('Origin',(49.7710265683621,13.4386401876617,-10.8660811365416));
#28402=CARTESIAN_POINT('Origin',(0.0835265683620477,12.8136401876617,0.0824317919394229));
#28403=CARTESIAN_POINT('Ctrl Pts',(49.9887116253026,13.0346110567825,-8.62119821111519));
#28404=CARTESIAN_POINT('Ctrl Pts',(49.9661757048102,13.0572884391283,-8.88240655691535));
#28405=CARTESIAN_POINT('Ctrl Pts',(49.9426352641249,13.0745923805885,-9.14384146257121));
#28406=CARTESIAN_POINT('Ctrl Pts',(49.918105661078,13.0880420719089,-9.40541317909589));
#28407=CARTESIAN_POINT('Ctrl Pts',(49.9075481310961,13.0938308129289,-9.51799352678263));
#28408=CARTESIAN_POINT('Ctrl Pts',(49.8968072588538,13.0989048483046,-9.63059933088929));
#28409=CARTESIAN_POINT('Ctrl Pts',(49.8858838002042,13.1033825850674,-9.74322381006683));
#28410=CARTESIAN_POINT('Ctrl Pts',(49.8858546717335,13.1033945253904,-9.74352413425422));
#28411=CARTESIAN_POINT('Ctrl Pts',(49.8858255419225,13.1034064614893,-9.74382445900064));
#28412=CARTESIAN_POINT('Ctrl Pts',(49.8857964107712,13.1034183933662,-9.74412478430632));
#28413=CARTESIAN_POINT('Ctrl Pts',(49.8621111558389,13.113119676523,-9.98830605051857));
#28414=CARTESIAN_POINT('Ctrl Pts',(49.8375747661617,13.1198333629724,-10.2324983067964));
#28415=CARTESIAN_POINT('Ctrl Pts',(49.8122023193407,13.123330972524,-10.4766688600581));
#28416=CARTESIAN_POINT('Ctrl Pts',(49.7987131033095,13.1251904703945,-10.6064816985539));
#28417=CARTESIAN_POINT('Ctrl Pts',(49.7849874188113,13.1261401876617,-10.7362881913535));
#28418=CARTESIAN_POINT('Ctrl Pts',(49.7710265683621,13.1261401876617,-10.8660811365416));
#28419=CARTESIAN_POINT('Origin',(36.6227242513098,12.3739187291548,-34.6889992126612));
#28420=CARTESIAN_POINT('Origin',(36.3116988338421,11.9341984494202,-34.377973520574));
#28421=CARTESIAN_POINT('Ctrl Pts',(22.7887737236329,-8.87385981233827,-49.9175682080606));
#28422=CARTESIAN_POINT('Ctrl Pts',(22.7887737236329,-8.56135981233826,-49.9175682080606));
#28423=CARTESIAN_POINT('Ctrl Pts',(22.7887737236329,-8.56135981233827,-49.6050682080606));
#28424=CARTESIAN_POINT('Ctrl Pts',(22.6060432734091,-8.87385981115686,-49.9175682080606));
#28425=CARTESIAN_POINT('Ctrl Pts',(22.630506965973,-8.59410214473098,-49.9175682080606));
#28426=CARTESIAN_POINT('Ctrl Pts',(22.6218302886772,-8.56135981233827,-49.6396055907562));
#28427=CARTESIAN_POINT('Ctrl Pts',(22.4199497037722,-8.86016990857446,-49.9175682080606));
#28428=CARTESIAN_POINT('Ctrl Pts',(22.4537595355486,-8.61269267441879,-49.9175682080606));
#28429=CARTESIAN_POINT('Ctrl Pts',(22.4513199439386,-8.55451485837127,-49.6745741172675));
#28430=CARTESIAN_POINT('Ctrl Pts',(22.0556610128347,-8.80243256293693,-49.9175682080606));
#28431=CARTESIAN_POINT('Ctrl Pts',(22.1054332504262,-8.61241087733877,-49.9175682080606));
#28432=CARTESIAN_POINT('Ctrl Pts',(22.1166038668002,-8.52564618972366,-49.7426016210618));
#28433=CARTESIAN_POINT('Ctrl Pts',(21.8765903956183,-8.75973143359561,-49.9175682080606));
#28434=CARTESIAN_POINT('Ctrl Pts',(21.9308811035567,-8.59777411058361,-49.9175682080626));
#28435=CARTESIAN_POINT('Ctrl Pts',(21.9517844512709,-8.50433615795936,-49.7757905000569));
#28436=CARTESIAN_POINT('Ctrl Pts',(21.7038295264605,-8.69080155058829,-49.9175682080606));
#28437=CARTESIAN_POINT('Ctrl Pts',(21.7573153886808,-8.5567486113334,-49.9175682080606));
#28438=CARTESIAN_POINT('Ctrl Pts',(21.7919948253812,-8.46983068146548,-49.8076885551764));
#28439=CARTESIAN_POINT('Origin',(21.7038295264614,-8.69080155057986,-49.6050682080606));
#28440=CARTESIAN_POINT('Origin',(22.7887737236329,-8.87385981233827,-49.6050682080606));
#28441=CARTESIAN_POINT('Origin',(-37.6513250757665,-8.24885981233827,-39.4201868051554));
#28442=CARTESIAN_POINT('Origin',(-37.6513250757665,-8.24885981233827,-39.4201868051554));
#28443=CARTESIAN_POINT('Origin',(-37.6513250757665,-8.24885981233827,-39.4201868051554));
#28444=CARTESIAN_POINT('Origin',(-39.6912298733813,12.8136401876617,-39.6923246498039));
#28445=CARTESIAN_POINT('Origin',(-40.5751133498644,12.8136401876617,-38.8084411733207));
#28446=CARTESIAN_POINT('Origin',(-44.291473431638,13.4386401876617,-44.2925682080606));
#28447=CARTESIAN_POINT('Origin',(-49.603973431638,13.4386401876617,-44.2925682080605));
#28448=CARTESIAN_POINT('Ctrl Pts',(49.9887116253026,13.0346110567825,-8.62119821111519));
#28449=CARTESIAN_POINT('Ctrl Pts',(50.0835265683621,13.1253379748597,-8.60561042268191));
#28450=CARTESIAN_POINT('Ctrl Pts',(50.0835265683621,13.2555819259033,-8.58323321427883));
#28451=CARTESIAN_POINT('Ctrl Pts',(49.956506353427,13.0670184804063,-8.99448160864149));
#28452=CARTESIAN_POINT('Ctrl Pts',(50.0835265683621,13.1643191174749,-8.99361854621833));
#28453=CARTESIAN_POINT('Ctrl Pts',(50.0835265683621,13.3203828042289,-8.96039929864488));
#28454=CARTESIAN_POINT('Ctrl Pts',(49.9221708848413,13.0885197051919,-9.36912528698815));
#28455=CARTESIAN_POINT('Ctrl Pts',(50.0835265683621,13.1804336598305,-9.37537845335551));
#28456=CARTESIAN_POINT('Ctrl Pts',(50.0835265683621,13.363399222363,-9.34018351565049));
#28457=CARTESIAN_POINT('Ctrl Pts',(49.8494215535246,13.1183169307007,-10.1191242934122));
#28458=CARTESIAN_POINT('Ctrl Pts',(50.0835265683621,13.1821517325915,-10.1329527188525));
#28459=CARTESIAN_POINT('Ctrl Pts',(50.0835265683621,13.4229936740986,-10.1027753390215));
#28460=CARTESIAN_POINT('Ctrl Pts',(49.8110882266463,13.1261401876617,-10.4936310027383));
#28461=CARTESIAN_POINT('Ctrl Pts',(50.0835265683621,13.163800762876,-10.5159536164931));
#28462=CARTESIAN_POINT('Ctrl Pts',(50.0835265683621,13.4386401852138,-10.4848020818312));
#28463=CARTESIAN_POINT('Ctrl Pts',(49.7710265683621,13.1261401876617,-10.8660811365416));
#28464=CARTESIAN_POINT('Ctrl Pts',(50.0835265683621,13.1261401876617,-10.8660811365416));
#28465=CARTESIAN_POINT('Ctrl Pts',(50.0835265683621,13.4386401876617,-10.8660811365416));
#28466=CARTESIAN_POINT('Origin',(49.7710265683621,13.2555819259033,-8.58323321427883));
#28467=CARTESIAN_POINT('Origin',(36.3116988338421,11.9341984494201,-34.377973520574));
#28468=CARTESIAN_POINT('Origin',(36.3116988338421,11.9341984494201,-34.377973520574));
#28469=CARTESIAN_POINT('Origin',(36.3116988338421,11.9341984494201,-34.377973520574));
#28470=CARTESIAN_POINT('Origin',(41.4050790939511,-8.24885981233827,-39.4713537806829));
#28471=CARTESIAN_POINT('Origin',(39.586145165457,-8.24885981233827,-37.6524198521889));
#28472=CARTESIAN_POINT('Origin',(0.0835265683620477,-8.87385981233827,-49.6050682080606));
#28473=CARTESIAN_POINT('Origin',(44.4585265683622,-8.87385981233827,-49.6050682080606));
#28474=CARTESIAN_POINT('Ctrl Pts',(21.9120191201608,-8.77420095227338,-49.9175682080606));
#28475=CARTESIAN_POINT('Ctrl Pts',(21.9659793624217,-8.6400331083672,-49.9175682080606));
#28476=CARTESIAN_POINT('Ctrl Pts',(22.0009097439611,-8.55319446848574,-49.8073324854834));
#28477=CARTESIAN_POINT('Ctrl Pts',(18.416083709289,-7.36815837305484,-49.9175682080606));
#28478=CARTESIAN_POINT('Ctrl Pts',(18.4800995730594,-7.24249091494012,-49.9175682080606));
#28479=CARTESIAN_POINT('Ctrl Pts',(18.4930530061579,-7.14715496089317,-49.8125752704599));
#28480=CARTESIAN_POINT('Ctrl Pts',(14.8511163433864,-6.21561709174538,-49.9175682080606));
#28481=CARTESIAN_POINT('Ctrl Pts',(14.9005782180646,-6.08656532545208,-49.9175682080606));
#28482=CARTESIAN_POINT('Ctrl Pts',(14.914458845539,-5.9946085575776,-49.8172935699712));
#28483=CARTESIAN_POINT('Ctrl Pts',(9.39579666290848,-5.02557369219655,-49.9175682080606));
#28484=CARTESIAN_POINT('Ctrl Pts',(9.42266531444727,-4.8958192523429,-49.9175682080606));
#28485=CARTESIAN_POINT('Ctrl Pts',(9.43658922229887,-4.80456526664712,-49.8223359778271));
#28486=CARTESIAN_POINT('Ctrl Pts',(7.57838814645687,-4.71947214408127,-49.9175682080606));
#28487=CARTESIAN_POINT('Ctrl Pts',(7.59939962270635,-4.58961053626329,-49.9175682080606));
#28488=CARTESIAN_POINT('Ctrl Pts',(7.61140680648957,-4.4984637156123,-49.823670236462));
#28489=CARTESIAN_POINT('Ctrl Pts',(4.81242924625007,-4.40691837826564,-49.9175682080606));
#28490=CARTESIAN_POINT('Ctrl Pts',(4.82512043530452,-4.2772572131369,-49.9175682080606));
#28491=CARTESIAN_POINT('Ctrl Pts',(4.8333804099258,-4.18590981848868,-49.8250429970702));
#28492=CARTESIAN_POINT('Ctrl Pts',(3.88371419304163,-4.327158062246,-49.9175682080606));
#28493=CARTESIAN_POINT('Ctrl Pts',(3.89381225256888,-4.19755005843117,-49.9175682080606));
#28494=CARTESIAN_POINT('Ctrl Pts',(3.9005754487046,-4.1061494680653,-49.8253960354399));
#28495=CARTESIAN_POINT('Ctrl Pts',(2.01256027103393,-4.21946011836696,-49.9175682080606));
#28496=CARTESIAN_POINT('Ctrl Pts',(2.01779667868678,-4.08996813964017,-49.9175682080606));
#28497=CARTESIAN_POINT('Ctrl Pts',(2.02114001333537,-3.99845145937632,-49.8258735845114));
#28498=CARTESIAN_POINT('Ctrl Pts',(1.0793230968735,-4.19205938565825,-49.9175682080606));
#28499=CARTESIAN_POINT('Ctrl Pts',(1.08192261688495,-4.06258497561548,-49.9175682080606));
#28500=CARTESIAN_POINT('Ctrl Pts',(1.08375236041024,-3.9710507150754,-49.8259956725485));
#28501=CARTESIAN_POINT('Ctrl Pts',(-3.57528016808697,-4.18598197768416,
-49.9175682080606));
#28502=CARTESIAN_POINT('Ctrl Pts',(-3.58473840334075,-4.05651422028169,
-49.9175682080606));
#28503=CARTESIAN_POINT('Ctrl Pts',(-3.59155443180908,-3.96497330343923,
-49.8260227101939));
#28504=CARTESIAN_POINT('Ctrl Pts',(-7.26155728764166,-4.60394036703586,
-49.9175682080606));
#28505=CARTESIAN_POINT('Ctrl Pts',(-7.29225903965945,-4.47650762043256,
-49.9175682080606));
#28506=CARTESIAN_POINT('Ctrl Pts',(-7.29419220051882,-4.38293092070441,
-49.8241256417463));
#28507=CARTESIAN_POINT('Ctrl Pts',(-11.8283085920387,-5.59091481619605,
-49.9175682080606));
#28508=CARTESIAN_POINT('Ctrl Pts',(-11.8595750836968,-5.46011080390599,
-49.9175682080606));
#28509=CARTESIAN_POINT('Ctrl Pts',(-11.8798541643496,-5.36990690683693,
-49.8199398075984));
#28510=CARTESIAN_POINT('Ctrl Pts',(-12.7389229297277,-5.81129472998947,
-49.9175682080606));
#28511=CARTESIAN_POINT('Ctrl Pts',(-12.7725641377111,-5.68032983292167,
-49.9175682080606));
#28512=CARTESIAN_POINT('Ctrl Pts',(-12.7941716628244,-5.59028691905929,
-49.8190149631812));
#28513=CARTESIAN_POINT('Ctrl Pts',(-14.5390501691854,-6.29050753230873,
-49.9175682080606));
#28514=CARTESIAN_POINT('Ctrl Pts',(-14.5770895837205,-6.15904772772748,
-49.9175682080606));
#28515=CARTESIAN_POINT('Ctrl Pts',(-14.6014698233081,-6.06949999371313,
-49.817034098248));
#28516=CARTESIAN_POINT('Ctrl Pts',(-15.4308544492521,-6.54980455615392,
-49.9175682080606));
#28517=CARTESIAN_POINT('Ctrl Pts',(-15.4711362244083,-6.41814737485005,
-49.9175682080606));
#28518=CARTESIAN_POINT('Ctrl Pts',(-15.4967513843562,-6.32879713522007,
-49.8159761217162));
#28519=CARTESIAN_POINT('Ctrl Pts',(-18.083799066244,-7.38126084278977,-49.9175682080606));
#28520=CARTESIAN_POINT('Ctrl Pts',(-18.133230497015,-7.2496461959732,-49.9175682080606));
#28521=CARTESIAN_POINT('Ctrl Pts',(-18.1597996579572,-7.16025352122019,
-49.8126404346489));
#28522=CARTESIAN_POINT('Ctrl Pts',(-19.8225328933696,-8.00683451480551,
-49.9175682080606));
#28523=CARTESIAN_POINT('Ctrl Pts',(-19.8764542487545,-7.87510646585778,
-49.9175682080606));
#28524=CARTESIAN_POINT('Ctrl Pts',(-19.9048327172755,-7.78582757943561,
-49.8102024034937));
#28525=CARTESIAN_POINT('Ctrl Pts',(-21.5367763897373,-8.69080155057986,
-49.9175682080606));
#28526=CARTESIAN_POINT('Ctrl Pts',(-21.5902754221335,-8.55671560258979,
-49.9175682080606));
#28527=CARTESIAN_POINT('Ctrl Pts',(-21.6249557626307,-8.4697954075151,-49.8076439541995));
#28528=CARTESIAN_POINT('Origin',(-21.5367763897373,-8.69080155057986,-49.6050682080606));
#28529=CARTESIAN_POINT('Origin',(0.0835265683620477,-8.24885981233827,0.0824317919394229));
#28530=CARTESIAN_POINT('Ctrl Pts',(-22.6217205869088,-8.56135981233827,
-49.6050682080606));
#28531=CARTESIAN_POINT('Ctrl Pts',(-22.4870650497075,-8.56135981233827,
-49.632925846288));
#28532=CARTESIAN_POINT('Ctrl Pts',(-22.3526852962314,-8.55702114807138,
-49.660532025143));
#28533=CARTESIAN_POINT('Ctrl Pts',(-22.218611604898,-8.54791555691041,-49.6878806083244));
#28534=CARTESIAN_POINT('Ctrl Pts',(-22.1862325124773,-8.54571653654471,
-49.6944853515339));
#28535=CARTESIAN_POINT('Ctrl Pts',(-22.1538713295352,-8.5432392648958,-49.7010750507536));
#28536=CARTESIAN_POINT('Ctrl Pts',(-22.1215285998496,-8.54047726034825,
-49.7076495796239));
#28537=CARTESIAN_POINT('Ctrl Pts',(-22.1202156261661,-8.54036513501685,
-49.7079164768052));
#28538=CARTESIAN_POINT('Ctrl Pts',(-22.118902733746,-8.54025254469889,-49.7081833384701));
#28539=CARTESIAN_POINT('Ctrl Pts',(-22.117589920377,-8.54013948886801,-49.7084501650743));
#28540=CARTESIAN_POINT('Ctrl Pts',(-22.0560724680956,-8.53484177721648,
-49.7209534601193));
#28541=CARTESIAN_POINT('Ctrl Pts',(-21.9945592187267,-8.5285710544529,-49.733413252321));
#28542=CARTESIAN_POINT('Ctrl Pts',(-21.9331497324827,-8.52099310668472,
-49.7458111112004));
#28543=CARTESIAN_POINT('Ctrl Pts',(-21.8801974450504,-8.51445877961392,
-49.7565015603001));
#28544=CARTESIAN_POINT('Ctrl Pts',(-21.8273216695811,-8.50695259656883,
-49.767146064923));
#28545=CARTESIAN_POINT('Ctrl Pts',(-21.7746031077857,-8.49822768693253,
-49.7777286249897));
#28546=CARTESIAN_POINT('Ctrl Pts',(-21.7245435456955,-8.48994284112497,
-49.7877774257287));
#28547=CARTESIAN_POINT('Ctrl Pts',(-21.6746251818596,-8.48055949752606,
-49.7977704781088));
#28548=CARTESIAN_POINT('Ctrl Pts',(-21.6249416886588,-8.46983068145907,
-49.8076885551783));
#28549=CARTESIAN_POINT('Origin',(-39.4702590042605,-8.24885981233827,-41.2391207336494));
#28550=CARTESIAN_POINT('Origin',(-26.1753569081211,12.8136401876617,-24.4086847315773));
#28551=CARTESIAN_POINT('Origin',(-36.7666959739416,12.8136401876617,-35.0000237973978));
#28552=CARTESIAN_POINT('Origin',(0.0835265683620477,12.8136401876617,0.0824317919394229));
#28553=CARTESIAN_POINT('Ctrl Pts',(-49.603973431638,13.1261401876617,-10.8660811365418));
#28554=CARTESIAN_POINT('Ctrl Pts',(-49.644220100234,13.1261401876617,-10.4919109761389));
#28555=CARTESIAN_POINT('Ctrl Pts',(-49.6825074995808,13.1182694471954,-10.1177151148479));
#28556=CARTESIAN_POINT('Ctrl Pts',(-49.7188065373979,13.1033923474055,-9.74347094847105));
#28557=CARTESIAN_POINT('Ctrl Pts',(-49.718812100481,13.1033900673852,-9.74341359291761));
#28558=CARTESIAN_POINT('Ctrl Pts',(-49.7188176635159,13.1033877872102,-9.74335623737716));
#28559=CARTESIAN_POINT('Ctrl Pts',(-49.7188232265025,13.1033855068804,-9.74329888184971));
#28560=CARTESIAN_POINT('Ctrl Pts',(-49.7399406684873,13.0947292335955,-9.52557374406794));
#28561=CARTESIAN_POINT('Ctrl Pts',(-49.7603774319321,13.0838402503142,-9.30789186800036));
#28562=CARTESIAN_POINT('Ctrl Pts',(-49.7801260723316,13.0698690454478,-9.09033516972605));
#28563=CARTESIAN_POINT('Ctrl Pts',(-49.7943282328449,13.0598217059822,-8.93388008790132));
#28564=CARTESIAN_POINT('Ctrl Pts',(-49.8081743398752,13.0481798478112,-8.77748968268304));
#28565=CARTESIAN_POINT('Ctrl Pts',(-49.8216584885772,13.0346110567867,-8.62119821111491));
#28566=CARTESIAN_POINT('Origin',(-36.7666959739416,12.8136401876617,-35.0000237973978));
#28567=CARTESIAN_POINT('Origin',(-49.603973431638,13.4386401876617,0.0824317919394229));
#28568=CARTESIAN_POINT('Origin',(-49.603973431638,13.4386401876617,-10.8660811365418));
#28569=CARTESIAN_POINT('Ctrl Pts',(49.9887116253026,13.0346110567825,8.78606179499438));
#28570=CARTESIAN_POINT('Ctrl Pts',(50.083526568362,13.1253379748597,8.77047400656112));
#28571=CARTESIAN_POINT('Ctrl Pts',(50.083526568362,13.2555819259033,8.74809679815803));
#28572=CARTESIAN_POINT('Ctrl Pts',(49.9908311071223,12.5435283274362,5.91561885766924));
#28573=CARTESIAN_POINT('Ctrl Pts',(50.083526568362,12.6357570952139,5.91066276265311));
#28574=CARTESIAN_POINT('Ctrl Pts',(50.083526568362,12.7644980954124,5.88980021407049));
#28575=CARTESIAN_POINT('Ctrl Pts',(49.9919944362938,12.2852858973076,3.01901638821139));
#28576=CARTESIAN_POINT('Ctrl Pts',(50.0835265683621,12.3768143018414,3.01363906603581));
#28577=CARTESIAN_POINT('Ctrl Pts',(50.083526568362,12.5062567663973,3.00601459538233));
#28578=CARTESIAN_POINT('Ctrl Pts',(49.9919989292124,12.2842756298938,-1.36854617605777));
#28579=CARTESIAN_POINT('Ctrl Pts',(50.0835265683621,12.3758051232112,-1.36588312104414));
#28580=CARTESIAN_POINT('Ctrl Pts',(50.0835265683621,12.5052464990302,-1.36212193922448));
#28581=CARTESIAN_POINT('Ctrl Pts',(49.9917102361039,12.3489547591789,-2.84244469713244));
#28582=CARTESIAN_POINT('Ctrl Pts',(50.0835265683621,12.4404805872093,-2.83784203918765));
#28583=CARTESIAN_POINT('Ctrl Pts',(50.0835265683621,12.5699256283428,-2.82949528855841));
#28584=CARTESIAN_POINT('Ctrl Pts',(49.9905929379208,12.602124859829,-5.75141479186526));
#28585=CARTESIAN_POINT('Ctrl Pts',(50.0835265683621,12.69337879361,-5.74157443732728));
#28586=CARTESIAN_POINT('Ctrl Pts',(50.0835265683621,12.8230957289067,-5.72573254687836));
#28587=CARTESIAN_POINT('Ctrl Pts',(49.9897665577655,12.7901838029195,-7.19248886629495));
#28588=CARTESIAN_POINT('Ctrl Pts',(50.0835265683621,12.8814125534697,-7.18075767287272));
#28589=CARTESIAN_POINT('Ctrl Pts',(50.0835265683621,13.011154579071,-7.16057213889734));
#28590=CARTESIAN_POINT('Ctrl Pts',(49.9887116253026,13.0346110567825,-8.62119821111519));
#28591=CARTESIAN_POINT('Ctrl Pts',(50.0835265683621,13.1253379748596,-8.60561042268192));
#28592=CARTESIAN_POINT('Ctrl Pts',(50.0835265683621,13.2555819259033,-8.58323321427883));
#28593=CARTESIAN_POINT('Origin',(49.771026568362,13.2555819259033,8.74809679815802));
#28594=CARTESIAN_POINT('Origin',(0.0835265683620477,11.9341984494201,0.0824317919394229));
#28595=CARTESIAN_POINT('Origin',(36.311698833842,11.9341984494201,34.542837104453));
#28596=CARTESIAN_POINT('Origin',(36.3116988338421,11.4830954176946,-34.377973520574));
#28597=CARTESIAN_POINT('Origin',(36.3116988338421,-3.61941807409669,-34.377973520574));
#28598=CARTESIAN_POINT('Ctrl Pts',(39.4263608497803,-8.46983068145906,-37.499785984834));
#28599=CARTESIAN_POINT('Ctrl Pts',(39.2114523668546,-8.46631238203735,-37.7196687918281));
#28600=CARTESIAN_POINT('Ctrl Pts',(39.3651742963362,-8.24885981233826,-37.8733907213097));
#28601=CARTESIAN_POINT('Ctrl Pts',(38.3347932895204,-6.92666471828348,-36.4084204095771));
#28602=CARTESIAN_POINT('Ctrl Pts',(38.120300318573,-6.92339564386607,-36.6285167435691));
#28603=CARTESIAN_POINT('Ctrl Pts',(38.273705416651,-6.70569384849234,-36.7819218416245));
#28604=CARTESIAN_POINT('Ctrl Pts',(37.24320552117,-5.38351572788356,-35.3170515943467));
#28605=CARTESIAN_POINT('Ctrl Pts',(37.0289440111501,-5.38020745678081,-35.5371604361463));
#28606=CARTESIAN_POINT('Ctrl Pts',(37.1822245238672,-5.16254485803749,-35.6904409488406));
#28607=CARTESIAN_POINT('Ctrl Pts',(36.1515914195989,-3.84038894321748,-34.2256786063308));
#28608=CARTESIAN_POINT('Ctrl Pts',(35.9372401080845,-3.8365505471153,-34.445456533058));
#28609=CARTESIAN_POINT('Ctrl Pts',(36.0907279647213,-3.61941807409669,-34.5989443896948));
#28610=CARTESIAN_POINT('Origin',(39.586145165457,-8.24885981233827,-37.6524198521889));
#28611=CARTESIAN_POINT('Origin',(36.3116988338421,-3.61941807409669,-34.377973520574));
#28612=CARTESIAN_POINT('Origin',(39.586145165457,-8.24885981233827,-37.6524198521889));
#28613=CARTESIAN_POINT('Origin',(39.586145165457,-8.24885981233827,-37.6524198521889));
#28614=CARTESIAN_POINT('Origin',(44.4585265683622,-8.87385981233827,-44.2925682080604));
#28615=CARTESIAN_POINT('Origin',(49.7710265683622,-8.87385981233827,-44.2925682080604));
#28616=CARTESIAN_POINT('Ctrl Pts',(-22.6217205869088,-8.56135981233827,
-49.6050682080606));
#28617=CARTESIAN_POINT('Ctrl Pts',(-22.6217205869088,-8.56135981233827,
-49.9175682080606));
#28618=CARTESIAN_POINT('Ctrl Pts',(-22.6217205869088,-8.87385981233827,
-49.9175682080606));
#28619=CARTESIAN_POINT('Ctrl Pts',(-22.4523904056315,-8.56135981233827,
-49.6400993625636));
#28620=CARTESIAN_POINT('Ctrl Pts',(-22.4612973244651,-8.59454828035443,
-49.9175682080606));
#28621=CARTESIAN_POINT('Ctrl Pts',(-22.436382391298,-8.87385980853143,-49.9175682080606));
#28622=CARTESIAN_POINT('Ctrl Pts',(-22.2842585826169,-8.55449257599307,
-49.6745749606216));
#28623=CARTESIAN_POINT('Ctrl Pts',(-22.2866330693819,-8.61264419244103,
-49.9175682080606));
#28624=CARTESIAN_POINT('Ctrl Pts',(-22.2528889951113,-8.86012534447524,
-49.9175682080606));
#28625=CARTESIAN_POINT('Ctrl Pts',(-21.9509213395377,-8.52578588737924,
-49.7423238840037));
#28626=CARTESIAN_POINT('Ctrl Pts',(-21.9397562137707,-8.61245644138935,
-49.9175682080606));
#28627=CARTESIAN_POINT('Ctrl Pts',(-21.8900982070676,-8.80271195759283,
-49.9175682080606));
#28628=CARTESIAN_POINT('Ctrl Pts',(-21.7844807419713,-8.5042820521619,-49.7758405246614));
#28629=CARTESIAN_POINT('Ctrl Pts',(-21.7635637494166,-8.59771167170021,
-49.9175682080606));
#28630=CARTESIAN_POINT('Ctrl Pts',(-21.7092890597639,-8.75963242031969,
-49.9175682080606));
#28631=CARTESIAN_POINT('Ctrl Pts',(-21.6249416886588,-8.46983068145907,
-49.8076885551783));
#28632=CARTESIAN_POINT('Ctrl Pts',(-21.5902622519579,-8.55674861132668,
-49.9175682080606));
#28633=CARTESIAN_POINT('Ctrl Pts',(-21.5367763897373,-8.69080155057986,
-49.9175682080606));
#28634=CARTESIAN_POINT('Origin',(-22.6217205869088,-8.87385981233827,-49.6050682080606));
#28635=CARTESIAN_POINT('Origin',(-36.7666959739416,12.8136401876617,-35.0000237973978));
#28636=CARTESIAN_POINT('Origin',(-36.7666959739416,12.8136401876617,-35.0000237973978));
#28637=CARTESIAN_POINT('Ctrl Pts',(-49.603973431638,13.1261401876617,-10.8660811365418));
#28638=CARTESIAN_POINT('Ctrl Pts',(-49.916473431638,13.1261401876617,-10.8660811365418));
#28639=CARTESIAN_POINT('Ctrl Pts',(-49.916473431638,13.4386401876617,-10.8660811365418));
#28640=CARTESIAN_POINT('Ctrl Pts',(-49.6441532614126,13.1261401876617,-10.4925323714846));
#28641=CARTESIAN_POINT('Ctrl Pts',(-49.916473431638,13.1639055963079,-10.5149789866091));
#28642=CARTESIAN_POINT('Ctrl Pts',(-49.916473431638,13.4386401851022,-10.4836786957547));
#28643=CARTESIAN_POINT('Ctrl Pts',(-49.6824505602016,13.1182927286052,-10.118301392099));
#28644=CARTESIAN_POINT('Ctrl Pts',(-49.9164734316366,13.1821712224823,-10.1321042920214));
#28645=CARTESIAN_POINT('Ctrl Pts',(-49.916473431638,13.4229452699559,-10.1019371937965));
#28646=CARTESIAN_POINT('Ctrl Pts',(-49.7551624447503,13.0884919386939,-9.3686405069943));
#28647=CARTESIAN_POINT('Ctrl Pts',(-49.9164734316392,13.1804128114024,-9.37487243571382));
#28648=CARTESIAN_POINT('Ctrl Pts',(-49.916473431638,13.3633436893187,-9.33969202550905));
#28649=CARTESIAN_POINT('Ctrl Pts',(-49.789510779629,13.066960554456,-8.99381440095842));
#28650=CARTESIAN_POINT('Ctrl Pts',(-49.9164734316379,13.1642472289408,-8.99290301434246));
#28651=CARTESIAN_POINT('Ctrl Pts',(-49.916473431638,13.3202672259813,-8.95972660866116));
#28652=CARTESIAN_POINT('Ctrl Pts',(-49.8216584885772,13.0346110567867,-8.62119821111442));
#28653=CARTESIAN_POINT('Ctrl Pts',(-49.9164734316379,13.125337974864,-8.60561042268131));
#28654=CARTESIAN_POINT('Ctrl Pts',(-49.916473431638,13.2555819259088,-8.5832332142783));
#28655=CARTESIAN_POINT('Origin',(-49.603973431638,13.2555819259033,-8.58323321427904));
#28656=CARTESIAN_POINT('Ctrl Pts',(49.771026568362,13.1261401876617,11.0309447204208));
#28657=CARTESIAN_POINT('Ctrl Pts',(50.083526568362,13.1261401876617,11.0309447204208));
#28658=CARTESIAN_POINT('Ctrl Pts',(50.083526568362,13.4386401876617,11.0309447204208));
#28659=CARTESIAN_POINT('Ctrl Pts',(49.8112063981312,13.1261401876617,10.657395955363));
#28660=CARTESIAN_POINT('Ctrl Pts',(50.083526568362,13.1639055963028,10.6798425704875));
#28661=CARTESIAN_POINT('Ctrl Pts',(50.083526568362,13.4386401851022,10.6485422796337));
#28662=CARTESIAN_POINT('Ctrl Pts',(49.8495036969259,13.1182927286052,10.2831649759781));
#28663=CARTESIAN_POINT('Ctrl Pts',(50.0835265683606,13.1821712224833,10.2969678759003));
#28664=CARTESIAN_POINT('Ctrl Pts',(50.083526568362,13.4229452699559,10.2668007776755));
#28665=CARTESIAN_POINT('Ctrl Pts',(49.9222155814742,13.0884919386938,9.53350409087325));
#28666=CARTESIAN_POINT('Ctrl Pts',(50.0835265683633,13.1804128114014,9.53973601959273));
#28667=CARTESIAN_POINT('Ctrl Pts',(50.083526568362,13.3633436893187,9.50455560938805));
#28668=CARTESIAN_POINT('Ctrl Pts',(49.9565639163529,13.0669605544559,9.15867798483744));
#28669=CARTESIAN_POINT('Ctrl Pts',(50.083526568362,13.1642472289387,9.15776659822167));
#28670=CARTESIAN_POINT('Ctrl Pts',(50.083526568362,13.3202672259815,9.12459019254013));
#28671=CARTESIAN_POINT('Ctrl Pts',(49.9887116253013,13.0346110567867,8.78606179499341));
#28672=CARTESIAN_POINT('Ctrl Pts',(50.083526568362,13.125337974864,8.77047400656029));
#28673=CARTESIAN_POINT('Ctrl Pts',(50.083526568362,13.2555819259088,8.74809679815729));
#28674=CARTESIAN_POINT('Origin',(49.771026568362,13.4386401876617,11.0309447204208));
#28675=CARTESIAN_POINT('Ctrl Pts',(49.9887116253012,13.0346110567867,8.7860617949939));
#28676=CARTESIAN_POINT('Ctrl Pts',(49.9699614074307,13.0534789730025,9.00339098706776));
#28677=CARTESIAN_POINT('Ctrl Pts',(49.9505117180268,13.0686233597236,9.22091083915132));
#28678=CARTESIAN_POINT('Ctrl Pts',(49.930377004077,13.0809296718092,9.4385314775567));
#28679=CARTESIAN_POINT('Ctrl Pts',(49.9158972002272,13.0897797098856,9.59503254162007));
#28680=CARTESIAN_POINT('Ctrl Pts',(49.9010628922511,13.0971603804857,9.7515862513039));
#28681=CARTESIAN_POINT('Ctrl Pts',(49.8858763632264,13.1033855068803,9.90816246572872));
#28682=CARTESIAN_POINT('Ctrl Pts',(49.8858708002398,13.1033877872101,9.90821982125617));
#28683=CARTESIAN_POINT('Ctrl Pts',(49.8858652372049,13.1033900673851,9.90827717679661));
#28684=CARTESIAN_POINT('Ctrl Pts',(49.8858596741218,13.1033923474054,9.90833453235006));
#28685=CARTESIAN_POINT('Ctrl Pts',(49.8495606363048,13.1182694471954,10.282578698727));
#28686=CARTESIAN_POINT('Ctrl Pts',(49.8112732369526,13.1261401876617,10.6567745600179));
#28687=CARTESIAN_POINT('Ctrl Pts',(49.771026568362,13.1261401876617,11.0309447204208));
#28688=CARTESIAN_POINT('Origin',(36.311698833842,11.9341984494201,34.542837104453));
#28689=CARTESIAN_POINT('Origin',(36.311698833842,11.9341984494202,34.542837104453));
#28690=CARTESIAN_POINT('Origin',(36.311698833842,11.9341984494201,34.542837104453));
#28691=CARTESIAN_POINT('Origin',(36.3116988338421,-3.61941807409669,-34.377973520574));
#28692=CARTESIAN_POINT('Origin',(36.3116988338421,-3.61941807409668,-34.377973520574));
#28693=CARTESIAN_POINT('Origin',(0.0835265683620477,-8.24885981233827,0.0824317919394229));
#28694=CARTESIAN_POINT('Ctrl Pts',(49.7710265683621,-8.56135981233827,-22.6228153633312));
#28695=CARTESIAN_POINT('Ctrl Pts',(49.7988842066419,-8.56135981233827,-22.4881598258772));
#28696=CARTESIAN_POINT('Ctrl Pts',(49.8264903855486,-8.55702114805526,-22.3537800721493));
#28697=CARTESIAN_POINT('Ctrl Pts',(49.8538389687804,-8.54791555685928,-22.2197063805655));
#28698=CARTESIAN_POINT('Ctrl Pts',(49.8604437119383,-8.54571653650635,-22.1873272883967));
#28699=CARTESIAN_POINT('Ctrl Pts',(49.8670334111066,-8.54323926487447,-22.1549661057063));
#28700=CARTESIAN_POINT('Ctrl Pts',(49.8736079399258,-8.54047726034837,-22.122623376272));
#28701=CARTESIAN_POINT('Ctrl Pts',(49.8738748371071,-8.54036513501696,-22.1213104025886));
#28702=CARTESIAN_POINT('Ctrl Pts',(49.874141698772,-8.540252544699,-22.1199975101685));
#28703=CARTESIAN_POINT('Ctrl Pts',(49.8744085253762,-8.54013948886812,-22.1186846967995));
#28704=CARTESIAN_POINT('Ctrl Pts',(49.8869118204158,-8.53484177721875,-22.0571672445435));
#28705=CARTESIAN_POINT('Ctrl Pts',(49.8993716126124,-8.52857105445812,-21.9956539952));
#28706=CARTESIAN_POINT('Ctrl Pts',(49.9117694714868,-8.52099310669413,-21.9342445089813));
#28707=CARTESIAN_POINT('Ctrl Pts',(49.9224599205877,-8.51445877962352,-21.881292221543));
#28708=CARTESIAN_POINT('Ctrl Pts',(49.9331044252119,-8.50695259657853,-21.8284164460676));
#28709=CARTESIAN_POINT('Ctrl Pts',(49.9436869852797,-8.49822768694213,-21.7756978842662));
#28710=CARTESIAN_POINT('Ctrl Pts',(49.9537357860226,-8.48994284113222,-21.7256383221565));
#28711=CARTESIAN_POINT('Ctrl Pts',(49.9637288384065,-8.4805594975302,-21.6757199583012));
#28712=CARTESIAN_POINT('Ctrl Pts',(49.9736469154798,-8.46983068145907,-21.6260364650812));
#28713=CARTESIAN_POINT('Origin',(49.7710265683621,-8.87385981233827,0.0824317919395964));
#28714=CARTESIAN_POINT('Origin',(49.7710265683621,-8.87385981233827,-22.6228153633312));
#28715=CARTESIAN_POINT('Origin',(0.0835265683620477,-8.87385981233827,-49.6050682080606));
#28716=CARTESIAN_POINT('Origin',(-44.2914734316379,-8.87385981233827,-49.6050682080606));
#28717=CARTESIAN_POINT('Origin',(-41.2380259572268,-8.24885981233827,-39.4713537806831));
#28718=CARTESIAN_POINT('Origin',(-39.4190920287328,-8.24885981233827,-37.6524198521891));
#28719=CARTESIAN_POINT('Origin',(-36.4556708266332,12.3739193162038,-34.6889986706566));
#28720=CARTESIAN_POINT('Origin',(-36.1446456971179,11.9341984494201,-34.3779735205741));
#28721=CARTESIAN_POINT('Ctrl Pts',(-49.8216584885785,13.0346110567825,-8.62119821111539));
#28722=CARTESIAN_POINT('Ctrl Pts',(-49.916473431638,13.1253379748596,-8.60561042268212));
#28723=CARTESIAN_POINT('Ctrl Pts',(-49.916473431638,13.2555819259033,-8.58323321427904));
#28724=CARTESIAN_POINT('Ctrl Pts',(-49.8237759955599,12.5439858927424,-5.75342980308448));
#28725=CARTESIAN_POINT('Ctrl Pts',(-49.9164734316379,12.6362124110381,-5.74845883635996));
#28726=CARTESIAN_POINT('Ctrl Pts',(-49.916473431638,12.7649555013805,-5.72759890891797));
#28727=CARTESIAN_POINT('Ctrl Pts',(-49.8249470688541,12.2839886353264,-2.84806387820799));
#28728=CARTESIAN_POINT('Ctrl Pts',(-49.916473431638,12.3755184395154,-2.84268189602221));
#28729=CARTESIAN_POINT('Ctrl Pts',(-49.916473431638,12.5049595044998,-2.83508904408025));
#28730=CARTESIAN_POINT('Ctrl Pts',(-49.8249415226426,12.2852357315166,3.03418378172085));
#28731=CARTESIAN_POINT('Ctrl Pts',(-49.9164734316379,12.3767641898923,3.02877807703737));
#28732=CARTESIAN_POINT('Ctrl Pts',(-49.916473431638,12.5062066005848,3.02111483476545));
#28733=CARTESIAN_POINT('Ctrl Pts',(-49.8237672317522,12.5460164567317,5.9301622998315));
#28734=CARTESIAN_POINT('Ctrl Pts',(-49.916473431638,12.6382323220339,5.92512141906298));
#28735=CARTESIAN_POINT('Ctrl Pts',(-49.916473431638,12.7669860817746,5.90428125111807));
#28736=CARTESIAN_POINT('Ctrl Pts',(-49.8216584885785,13.0346110567825,8.78606179499423));
#28737=CARTESIAN_POINT('Ctrl Pts',(-49.9164734316379,13.1253379748596,8.77047400656096));
#28738=CARTESIAN_POINT('Ctrl Pts',(-49.916473431638,13.2555819259033,8.74809679815787));
#28739=CARTESIAN_POINT('Origin',(-49.603973431638,13.2555819259033,8.74809679815787));
#28740=CARTESIAN_POINT('Origin',(49.7710265683621,13.4386401876617,0.0824317919395964));
#28741=CARTESIAN_POINT('Origin',(49.7710265683619,13.4386401876617,36.6697170232579));
#28742=CARTESIAN_POINT('Origin',(0.0835265683620477,12.8136401876617,0.0824317919394229));
#28743=CARTESIAN_POINT('Origin',(36.9337491106657,12.8136401876617,35.1648873812767));
#28744=CARTESIAN_POINT('Origin',(36.6227239633541,12.3739193162048,34.853862254537));
#28745=CARTESIAN_POINT('Origin',(36.9337491106657,12.8136401876617,35.1648873812767));
#28746=CARTESIAN_POINT('Origin',(36.311698833842,11.4830954176946,34.542837104453));
#28747=CARTESIAN_POINT('Origin',(36.311698833842,-3.61941807409668,34.542837104453));
#28748=CARTESIAN_POINT('Origin',(0.0835265683620477,-3.61941807409668,0.0824317919394229));
#28749=CARTESIAN_POINT('Origin',(36.311698833842,-3.61941807409668,34.542837104453));
#28750=CARTESIAN_POINT('Ctrl Pts',(49.7710265683621,-8.56135981233827,-22.6228153633312));
#28751=CARTESIAN_POINT('Ctrl Pts',(50.0835265683621,-8.56135981233826,-22.6228153633312));
#28752=CARTESIAN_POINT('Ctrl Pts',(50.0835265683621,-8.87385981233827,-22.6228153633312));
#28753=CARTESIAN_POINT('Ctrl Pts',(49.8060577228649,-8.56135981233827,-22.453485182054));
#28754=CARTESIAN_POINT('Ctrl Pts',(50.0835265683603,-8.59454828035624,-22.4623921008879));
#28755=CARTESIAN_POINT('Ctrl Pts',(50.0835265683621,-8.87385980853143,-22.4374771677204));
#28756=CARTESIAN_POINT('Ctrl Pts',(49.8405333209238,-8.55449257599331,-22.2853533590394));
#28757=CARTESIAN_POINT('Ctrl Pts',(50.0835265683621,-8.6126441924417,-22.2877278458042));
#28758=CARTESIAN_POINT('Ctrl Pts',(50.0835265683621,-8.86012534447524,-22.2539837715337));
#28759=CARTESIAN_POINT('Ctrl Pts',(49.9082822443045,-8.52578588737901,-21.9520161159601));
#28760=CARTESIAN_POINT('Ctrl Pts',(50.0835265683621,-8.61245644138874,-21.940850990193));
#28761=CARTESIAN_POINT('Ctrl Pts',(50.0835265683621,-8.80271195759284,-21.8911929834901));
#28762=CARTESIAN_POINT('Ctrl Pts',(49.9417988849617,-8.50428205216071,-21.7855755183937));
#28763=CARTESIAN_POINT('Ctrl Pts',(50.0835265683621,-8.59771167170023,-21.7646585258391));
#28764=CARTESIAN_POINT('Ctrl Pts',(50.0835265683621,-8.75963242031947,-21.7103838361864));
#28765=CARTESIAN_POINT('Ctrl Pts',(49.9736469154798,-8.46983068145907,-21.6260364650812));
#28766=CARTESIAN_POINT('Ctrl Pts',(50.0835265683621,-8.55674861132668,-21.5913570283804));
#28767=CARTESIAN_POINT('Ctrl Pts',(50.0835265683621,-8.69080155057987,-21.5378711661598));
#28768=CARTESIAN_POINT('Origin',(49.7710265683621,-8.69080155057986,-21.5378711661598));
#28769=CARTESIAN_POINT('Origin',(-44.291473431638,-8.87385981233827,-44.2925682080606));
#28770=CARTESIAN_POINT('Origin',(-49.603973431638,-8.87385981233827,-44.2925682080605));
#28771=CARTESIAN_POINT('Origin',(-39.4190920287328,-8.24885981233827,-37.6524198521891));
#28772=CARTESIAN_POINT('Origin',(-39.4190920287328,-8.24885981233827,-37.6524198521891));
#28773=CARTESIAN_POINT('Origin',(-39.4190920287328,-8.24885981233827,-37.6524198521891));
#28774=CARTESIAN_POINT('Origin',(-36.1446456971179,11.9341984494201,-34.3779735205741));
#28775=CARTESIAN_POINT('Origin',(-36.1446456971179,11.9341984494201,-34.3779735205741));
#28776=CARTESIAN_POINT('Origin',(-36.1446456971179,11.9341984494202,-34.3779735205741));
#28777=CARTESIAN_POINT('Ctrl Pts',(-49.8216584885785,13.0346110567825,8.78606179499422));
#28778=CARTESIAN_POINT('Ctrl Pts',(-49.9164734316379,13.1253379748597,8.77047400656095));
#28779=CARTESIAN_POINT('Ctrl Pts',(-49.916473431638,13.2555819259033,8.74809679815786));
#28780=CARTESIAN_POINT('Ctrl Pts',(-49.7894532167015,13.0670184804049,9.15934519252001));
#28781=CARTESIAN_POINT('Ctrl Pts',(-49.916473431638,13.1643191174741,9.15848213009695));
#28782=CARTESIAN_POINT('Ctrl Pts',(-49.916473431638,13.3203828042259,9.12526288252385));
#28783=CARTESIAN_POINT('Ctrl Pts',(-49.7551177481173,13.088519705192,9.53398887086785));
#28784=CARTESIAN_POINT('Ctrl Pts',(-49.9164734316379,13.1804336598305,9.5402420372352));
#28785=CARTESIAN_POINT('Ctrl Pts',(-49.916473431638,13.3633992223637,9.50504709953018));
#28786=CARTESIAN_POINT('Ctrl Pts',(-49.6823684168004,13.1183169307006,10.2839878772905));
#28787=CARTESIAN_POINT('Ctrl Pts',(-49.9164734316379,13.1821517325915,10.2978163027309));
#28788=CARTESIAN_POINT('Ctrl Pts',(-49.916473431638,13.4229936740979,10.2676389228998));
#28789=CARTESIAN_POINT('Ctrl Pts',(-49.6440350899221,13.1261401876617,10.6584945866178));
#28790=CARTESIAN_POINT('Ctrl Pts',(-49.9164734316379,13.163800762876,10.6808172003725));
#28791=CARTESIAN_POINT('Ctrl Pts',(-49.916473431638,13.4386401852138,10.6496656657108));
#28792=CARTESIAN_POINT('Ctrl Pts',(-49.603973431638,13.1261401876617,11.0309447204206));
#28793=CARTESIAN_POINT('Ctrl Pts',(-49.9164734316379,13.1261401876617,11.0309447204206));
#28794=CARTESIAN_POINT('Ctrl Pts',(-49.916473431638,13.4386401876617,11.0309447204206));
#28795=CARTESIAN_POINT('Ctrl Pts',(-49.603973431638,13.1261401876617,11.0309447204206));
#28796=CARTESIAN_POINT('Ctrl Pts',(-49.6302329959052,13.1261401876617,10.7868115855527));
#28797=CARTESIAN_POINT('Ctrl Pts',(-49.6556610339887,13.122783140923,10.5426318837783));
#28798=CARTESIAN_POINT('Ctrl Pts',(-49.6802470100602,13.1163230256676,10.2984481491949));
#28799=CARTESIAN_POINT('Ctrl Pts',(-49.6933181003556,13.1128885169226,10.1686283025428));
#28800=CARTESIAN_POINT('Ctrl Pts',(-49.7061510505488,13.1085760632363,10.0388069024177));
#28801=CARTESIAN_POINT('Ctrl Pts',(-49.7187432740471,13.1034183933663,9.90898836818533));
#28802=CARTESIAN_POINT('Ctrl Pts',(-49.7187724051985,13.1034064614893,9.90868804287966));
#28803=CARTESIAN_POINT('Ctrl Pts',(-49.7188015350095,13.1033945253904,9.90838771813324));
#28804=CARTESIAN_POINT('Ctrl Pts',(-49.7188306634802,13.1033825850675,9.90808739394585));
#28805=CARTESIAN_POINT('Ctrl Pts',(-49.7442104734438,13.0929789105763,9.64641314126808));
#28806=CARTESIAN_POINT('Ctrl Pts',(-49.768605180415,13.0793591824316,9.3848393250672));
#28807=CARTESIAN_POINT('Ctrl Pts',(-49.7920029933405,13.0610261308093,9.12345253841242));
#28808=CARTESIAN_POINT('Ctrl Pts',(-49.8020734013628,13.0531355937442,9.01095178453317));
#28809=CARTESIAN_POINT('Ctrl Pts',(-49.8119590386648,13.0443713918135,8.89848574803371));
#28810=CARTESIAN_POINT('Ctrl Pts',(-49.8216584885785,13.0346110567825,8.78606179499422));
#28811=CARTESIAN_POINT('Origin',(-49.603973431638,13.4386401876617,11.0309447204206));
#28812=CARTESIAN_POINT('Origin',(44.4585265683621,13.4386401876617,44.4574317919394));
#28813=CARTESIAN_POINT('Origin',(44.458526568362,13.4386401876617,49.7699317919394));
#28814=CARTESIAN_POINT('Origin',(36.9337491106657,12.8136401876617,35.1648873812767));
#28815=CARTESIAN_POINT('Origin',(36.9337491106657,12.8136401876617,35.1648873812767));
#28816=CARTESIAN_POINT('Origin',(36.311698833842,-3.61941807409668,34.542837104453));
#28817=CARTESIAN_POINT('Origin',(36.311698833842,-3.61941807409669,34.542837104453));
#28818=CARTESIAN_POINT('Ctrl Pts',(50.083526568362,-8.77420095969686,21.9109243621945));
#28819=CARTESIAN_POINT('Ctrl Pts',(50.0835265683628,-8.64003311578147,21.9648846044965));
#28820=CARTESIAN_POINT('Ctrl Pts',(49.9732908457536,-8.55319447590597,21.9998149860589));
#28821=CARTESIAN_POINT('Ctrl Pts',(50.083526568362,-7.36815837710381,18.4149889454167));
#28822=CARTESIAN_POINT('Ctrl Pts',(50.0835265683487,-7.24249091899859,18.4790048093049));
#28823=CARTESIAN_POINT('Ctrl Pts',(49.978533630732,-7.14715496494006,18.4919582423361));
#28824=CARTESIAN_POINT('Ctrl Pts',(50.083526568362,-6.21561709315083,14.8500215734068));
#28825=CARTESIAN_POINT('Ctrl Pts',(50.083526568362,-6.08656532686357,14.8994834481387));
#28826=CARTESIAN_POINT('Ctrl Pts',(49.9832519302634,-5.99460855897936,14.9133640755833));
#28827=CARTESIAN_POINT('Ctrl Pts',(50.083526568362,-5.02557369219655,9.39470188648604));
#28828=CARTESIAN_POINT('Ctrl Pts',(50.083526568362,-4.89581925233923,9.4215705380266));
#28829=CARTESIAN_POINT('Ctrl Pts',(49.9882943381249,-4.80456526664396,9.43549444587848));
#28830=CARTESIAN_POINT('Ctrl Pts',(50.083526568362,-4.71947214408127,7.57729337003443));
#28831=CARTESIAN_POINT('Ctrl Pts',(50.083526568362,-4.58961053625969,7.59830484628597));
#28832=CARTESIAN_POINT('Ctrl Pts',(49.98962859676,-4.49846371560897,7.61031203006756));
#28833=CARTESIAN_POINT('Ctrl Pts',(50.083526568362,-4.40691837826565,4.81133446982763));
#28834=CARTESIAN_POINT('Ctrl Pts',(50.083526568362,-4.27725721313452,4.82402565888155));
#28835=CARTESIAN_POINT('Ctrl Pts',(49.9910013573683,-4.18590981848534,4.83228563350366));
#28836=CARTESIAN_POINT('Ctrl Pts',(50.083526568362,-4.327158062246,3.88261941661919));
#28837=CARTESIAN_POINT('Ctrl Pts',(50.083526568362,-4.19755005842839,3.89271747614665));
#28838=CARTESIAN_POINT('Ctrl Pts',(49.991354395738,-4.10614946806195,3.89948067228241));
#28839=CARTESIAN_POINT('Ctrl Pts',(50.083526568362,-4.21946011836696,2.01146549461149));
#28840=CARTESIAN_POINT('Ctrl Pts',(50.0835265683621,-4.08996813963739,2.01670190226445));
#28841=CARTESIAN_POINT('Ctrl Pts',(49.9918319448095,-3.99845145937297,2.02004523691305));
#28842=CARTESIAN_POINT('Ctrl Pts',(50.0835265683621,-4.19205938565866,1.07822832045126));
#28843=CARTESIAN_POINT('Ctrl Pts',(50.0835265683621,-4.06258497561311,1.08082784046275));
#28844=CARTESIAN_POINT('Ctrl Pts',(49.9919540328468,-3.97105071507225,1.08265758398807));
#28845=CARTESIAN_POINT('Ctrl Pts',(50.0835265683621,-4.18598197768254,-3.57637494451022));
#28846=CARTESIAN_POINT('Ctrl Pts',(50.0835265683621,-4.05651422027729,-3.58583317976415));
#28847=CARTESIAN_POINT('Ctrl Pts',(49.9919810704912,-3.96497330343507,-3.59264920823258));
#28848=CARTESIAN_POINT('Ctrl Pts',(50.0835265683621,-4.60394036703586,-7.26265206407059));
#28849=CARTESIAN_POINT('Ctrl Pts',(50.0835265683621,-4.47650762043161,-7.29335381609307));
#28850=CARTESIAN_POINT('Ctrl Pts',(49.9900840020437,-4.3829309207017,-7.29528697694766));
#28851=CARTESIAN_POINT('Ctrl Pts',(50.0835265683621,-5.59091481619605,-11.8294033684595));
#28852=CARTESIAN_POINT('Ctrl Pts',(50.0835265683621,-5.46011080390277,-11.8606698601175));
#28853=CARTESIAN_POINT('Ctrl Pts',(49.9858981678965,-5.36990690683347,-11.8809489407712));
#28854=CARTESIAN_POINT('Ctrl Pts',(50.0835265683621,-5.81129472998664,-12.7400177061517));
#28855=CARTESIAN_POINT('Ctrl Pts',(50.0835265683589,-5.68032983291523,-12.773658914136));
#28856=CARTESIAN_POINT('Ctrl Pts',(49.9849733234776,-5.59028691905481,-12.7952664392488));
#28857=CARTESIAN_POINT('Ctrl Pts',(50.0835265683621,-6.29050753231155,-14.5401449456062));
#28858=CARTESIAN_POINT('Ctrl Pts',(50.0835265683654,-6.1590477277283,-14.5781843601422));
#28859=CARTESIAN_POINT('Ctrl Pts',(49.9829924585474,-6.06949999371107,-14.6025645997302));
#28860=CARTESIAN_POINT('Ctrl Pts',(50.0835265683621,-6.54980455615391,-15.4319492256746));
#28861=CARTESIAN_POINT('Ctrl Pts',(50.0835265683621,-6.41814737484765,-15.4722310008318));
#28862=CARTESIAN_POINT('Ctrl Pts',(49.9819344820143,-6.32879713521657,-15.497846160778));
#28863=CARTESIAN_POINT('Ctrl Pts',(50.0835265683621,-7.38126084278977,-18.0848938426664));
#28864=CARTESIAN_POINT('Ctrl Pts',(50.0835265683621,-7.24964619596978,-18.1343252734394));
#28865=CARTESIAN_POINT('Ctrl Pts',(49.9785987949462,-7.16025352121745,-18.1608944343837));
#28866=CARTESIAN_POINT('Ctrl Pts',(50.0835265683621,-8.0068345148146,-19.8236276697884));
#28867=CARTESIAN_POINT('Ctrl Pts',(50.0835265683621,-7.87510646586731,-19.8775490251741));
#28868=CARTESIAN_POINT('Ctrl Pts',(49.9761607637979,-7.78582757943672,-19.9059274936949));
#28869=CARTESIAN_POINT('Ctrl Pts',(50.0835265683621,-8.69080155057986,-21.5378711661598));
#28870=CARTESIAN_POINT('Ctrl Pts',(50.0835265683621,-8.55671560258686,-21.5913701985572));
#28871=CARTESIAN_POINT('Ctrl Pts',(49.9736023144971,-8.46979540751197,-21.6260505390544));
#28872=CARTESIAN_POINT('Origin',(49.771026568362,-8.69080155057986,21.702734750039));
#28873=CARTESIAN_POINT('Origin',(-49.603973431638,-8.87385981233827,0.0824317919394229));
#28874=CARTESIAN_POINT('Origin',(-49.603973431638,-8.87385981233827,-22.6228153633314));
#28875=CARTESIAN_POINT('Origin',(0.0835265683620477,-8.24885981233827,0.0824317919394229));
#28876=CARTESIAN_POINT('Ctrl Pts',(-49.8065937787538,-8.46983068146548,
-21.6260364650797));
#28877=CARTESIAN_POINT('Ctrl Pts',(-49.7945868225115,-8.48281912913915,
-21.6861839638978));
#28878=CARTESIAN_POINT('Ctrl Pts',(-49.7824920379308,-8.49383985403581,
-21.7465682311851));
#28879=CARTESIAN_POINT('Ctrl Pts',(-49.7703218005744,-8.50331222135076,
-21.8071274424854));
#28880=CARTESIAN_POINT('Ctrl Pts',(-49.7571156009582,-8.51359090121018,
-21.8728416113725));
#28881=CARTESIAN_POINT('Ctrl Pts',(-49.7438205451818,-8.52204613528895,
-21.9387618848257));
#28882=CARTESIAN_POINT('Ctrl Pts',(-49.7304472779566,-8.52915470825893,
-22.0048321176218));
#28883=CARTESIAN_POINT('Ctrl Pts',(-49.7228210345449,-8.53320844523035,
-22.042509348555));
#28884=CARTESIAN_POINT('Ctrl Pts',(-49.715169265573,-8.53682321976873,-22.0802357448589));
#28885=CARTESIAN_POINT('Ctrl Pts',(-49.707493320942,-8.5400806031776,-22.1180035325263));
#28886=CARTESIAN_POINT('Ctrl Pts',(-49.7072174179006,-8.54019768609479,
-22.119361052413));
#28887=CARTESIAN_POINT('Ctrl Pts',(-49.706941475036,-8.5403142598712,-22.1207186663251));
#28888=CARTESIAN_POINT('Ctrl Pts',(-49.7066654928968,-8.54043032524654,
-22.1220763716637));
#28889=CARTESIAN_POINT('Ctrl Pts',(-49.6933692202904,-8.54602212504574,
-22.1874879245738));
#28890=CARTESIAN_POINT('Ctrl Pts',(-49.680000075092,-8.55043067995626,-22.2530232013284));
#28891=CARTESIAN_POINT('Ctrl Pts',(-49.6665711482279,-8.5537415100254,-22.3186261411179));
#28892=CARTESIAN_POINT('Ctrl Pts',(-49.6531611054658,-8.55704768432024,
-22.3841368283679));
#28893=CARTESIAN_POINT('Ctrl Pts',(-49.6396908764539,-8.55925889971278,
-22.4497177613008));
#28894=CARTESIAN_POINT('Ctrl Pts',(-49.6261708648657,-8.56041391612595,
-22.5153164405566));
#28895=CARTESIAN_POINT('Ctrl Pts',(-49.6187858031651,-8.56104482294291,
-22.5511485321651));
#28896=CARTESIAN_POINT('Ctrl Pts',(-49.6113858916315,-8.56135981233827,
-22.586985736526));
#28897=CARTESIAN_POINT('Ctrl Pts',(-49.603973431638,-8.56135981233827,-22.6228153633314));
#28898=CARTESIAN_POINT('Ctrl Pts',(-39.198121159612,-8.24885981233822,-37.8733907213098));
#28899=CARTESIAN_POINT('Ctrl Pts',(-39.0443992301304,-8.46631238203731,
-37.7196687918282));
#28900=CARTESIAN_POINT('Ctrl Pts',(-39.259307713056,-8.46983068145902,-37.4997859848341));
#28901=CARTESIAN_POINT('Ctrl Pts',(-38.1066522799264,-6.70569384849083,
-36.7819218416243));
#28902=CARTESIAN_POINT('Ctrl Pts',(-37.9532471818597,-6.9233956438646,-36.6285167435576));
#28903=CARTESIAN_POINT('Ctrl Pts',(-38.1677401528067,-6.92666471828269,
-36.408420409565));
#28904=CARTESIAN_POINT('Ctrl Pts',(-37.0151713871357,-5.16254485804652,
-35.6904409488335));
#28905=CARTESIAN_POINT('Ctrl Pts',(-36.8618908744034,-5.38020745678985,
-35.5371604361543));
#28906=CARTESIAN_POINT('Ctrl Pts',(-37.0761523844306,-5.38351572788263,
-35.3170515943614));
#28907=CARTESIAN_POINT('Ctrl Pts',(-35.9236748279971,-3.61941807409667,
-34.5989443896949));
#28908=CARTESIAN_POINT('Ctrl Pts',(-35.7701869713603,-3.83655054711528,
-34.4454565330581));
#28909=CARTESIAN_POINT('Ctrl Pts',(-35.9845382828747,-3.84038894321746,
-34.2256786063309));
#28910=CARTESIAN_POINT('Origin',(-36.1446456971179,-3.61941807409669,-34.3779735205741));
#28911=CARTESIAN_POINT('Origin',(-36.1446456971179,11.4830954176946,-34.3779735205741));
#28912=CARTESIAN_POINT('Origin',(-36.1446456971179,-3.61941807409668,-34.3779735205741));
#28913=CARTESIAN_POINT('Origin',(0.0835265683620477,11.9341984494201,0.0824317919394229));
#28914=CARTESIAN_POINT('Origin',(-36.1446456971182,11.9341984494201,34.5428371044526));
#28915=CARTESIAN_POINT('Origin',(-36.4556711145887,12.3739187291526,34.8538627965404));
#28916=CARTESIAN_POINT('Origin',(-36.7666959739419,12.8136401876617,35.1648873812763));
#28917=CARTESIAN_POINT('Origin',(-36.1446456971182,11.9341984494202,34.5428371044526));
#28918=CARTESIAN_POINT('Origin',(0.0835265683620477,12.8136401876617,0.0824317919394229));
#28919=CARTESIAN_POINT('Origin',(-36.7666959739419,12.8136401876617,35.1648873812763));
#28920=CARTESIAN_POINT('Origin',(-49.603973431638,13.4386401876617,0.0824317919394229));
#28921=CARTESIAN_POINT('Origin',(-49.603973431638,13.4386401876617,44.4574317919389));
#28922=CARTESIAN_POINT('Origin',(0.0835265683620476,13.4386401876617,49.7699317919394));
#28923=CARTESIAN_POINT('Origin',(11.0320394968433,13.4386401876617,49.7699317919394));
#28924=CARTESIAN_POINT('Origin',(26.3424100448452,12.8136401876617,24.5735483154562));
#28925=CARTESIAN_POINT('Ctrl Pts',(39.3651742963362,-8.24885981233836,38.0382543051888));
#28926=CARTESIAN_POINT('Ctrl Pts',(39.2114523668546,-8.46631238203745,37.8845323757072));
#28927=CARTESIAN_POINT('Ctrl Pts',(39.4263608497802,-8.46983068145916,37.6646495687131));
#28928=CARTESIAN_POINT('Ctrl Pts',(38.2737054166549,-6.70569384848682,36.9467854255075));
#28929=CARTESIAN_POINT('Ctrl Pts',(38.1203003185921,-6.92339564386061,36.7933803274371));
#28930=CARTESIAN_POINT('Ctrl Pts',(38.3347932895352,-6.92666471828384,36.5732839934409));
#28931=CARTESIAN_POINT('Ctrl Pts',(37.1822245238622,-5.16254485804367,35.8553045327148));
#28932=CARTESIAN_POINT('Ctrl Pts',(37.0289440111306,-5.38020745678604,35.7020240200362));
#28933=CARTESIAN_POINT('Ctrl Pts',(37.2432055211549,-5.38351572788296,35.4819151782406));
#28934=CARTESIAN_POINT('Ctrl Pts',(36.0907279647212,-3.61941807409668,34.7638079735738));
#28935=CARTESIAN_POINT('Ctrl Pts',(35.9372401080844,-3.83655054711529,34.610320116937));
#28936=CARTESIAN_POINT('Ctrl Pts',(36.1515914195988,-3.84038894321748,34.3905421902098));
#28937=CARTESIAN_POINT('Origin',(39.5861451654569,-8.24885981233827,37.8172834360679));
#28938=CARTESIAN_POINT('Origin',(0.0835265683620477,-8.24885981233827,0.0824317919394229));
#28939=CARTESIAN_POINT('Ctrl Pts',(49.9736469154778,-8.46983068146547,21.7909000489587));
#28940=CARTESIAN_POINT('Ctrl Pts',(49.9616399592362,-8.48281912913843,21.8510475477735));
#28941=CARTESIAN_POINT('Ctrl Pts',(49.949545174656,-8.4938398540346,21.9114318150575));
#28942=CARTESIAN_POINT('Ctrl Pts',(49.9373749373003,-8.50331222134921,21.9719910263544));
#28943=CARTESIAN_POINT('Ctrl Pts',(49.9241687376785,-8.51359090121315,22.0377051952691));
#28944=CARTESIAN_POINT('Ctrl Pts',(49.9108736818965,-8.52204613529488,22.1036254687501));
#28945=CARTESIAN_POINT('Ctrl Pts',(49.8975004146657,-8.52915470826684,22.1696957015741));
#28946=CARTESIAN_POINT('Ctrl Pts',(49.8898741712589,-8.53320844523506,22.2073729324829));
#28947=CARTESIAN_POINT('Ctrl Pts',(49.882222402292,-8.53682321977086,22.2450993287624));
#28948=CARTESIAN_POINT('Ctrl Pts',(49.8745464576661,-8.54008060317762,22.2828671164053));
#28949=CARTESIAN_POINT('Ctrl Pts',(49.8742705546247,-8.54019768609482,22.284224636292));
#28950=CARTESIAN_POINT('Ctrl Pts',(49.8739946117601,-8.54031425987122,22.2855822502041));
#28951=CARTESIAN_POINT('Ctrl Pts',(49.8737186296209,-8.54043032524656,22.2869399555427));
#28952=CARTESIAN_POINT('Ctrl Pts',(49.8604223570134,-8.54602212504619,22.3523515084577));
#28953=CARTESIAN_POINT('Ctrl Pts',(49.8470532118141,-8.55043067995696,22.4178867852175));
#28954=CARTESIAN_POINT('Ctrl Pts',(49.8336242849491,-8.55374151002619,22.4834897250119));
#28955=CARTESIAN_POINT('Ctrl Pts',(49.820214242186,-8.55704768432111,22.5490004122671));
#28956=CARTESIAN_POINT('Ctrl Pts',(49.806744013173,-8.55925889971357,22.6145813452051));
#28957=CARTESIAN_POINT('Ctrl Pts',(49.7932240015836,-8.5604139161265,22.6801800244661));
#28958=CARTESIAN_POINT('Ctrl Pts',(49.7858389398851,-8.5610448229431,22.7160121160645));
#28959=CARTESIAN_POINT('Ctrl Pts',(49.7784390283535,-8.56135981233827,22.7518493204152));
#28960=CARTESIAN_POINT('Ctrl Pts',(49.771026568362,-8.56135981233827,22.7876789472104));
#28961=CARTESIAN_POINT('Origin',(39.5861451654569,-8.24885981233827,37.8172834360679));
#28962=CARTESIAN_POINT('Ctrl Pts',(50.083526568362,-8.87385981233827,22.7876789472104));
#28963=CARTESIAN_POINT('Ctrl Pts',(50.083526568362,-8.56135981233826,22.7876789472104));
#28964=CARTESIAN_POINT('Ctrl Pts',(49.771026568362,-8.56135981233827,22.7876789472104));
#28965=CARTESIAN_POINT('Ctrl Pts',(50.083526568362,-8.87385981115686,22.6049484969869));
#28966=CARTESIAN_POINT('Ctrl Pts',(50.083526568362,-8.59410214473078,22.6294121895504));
#28967=CARTESIAN_POINT('Ctrl Pts',(49.8055639510575,-8.56135981233827,22.6207355122547));
#28968=CARTESIAN_POINT('Ctrl Pts',(50.083526568362,-8.86016990857478,22.4188549273494));
#28969=CARTESIAN_POINT('Ctrl Pts',(50.083526568362,-8.61269267441895,22.4526647591265));
#28970=CARTESIAN_POINT('Ctrl Pts',(49.8405324775689,-8.55451485837129,22.4502251675162));
#28971=CARTESIAN_POINT('Ctrl Pts',(50.083526568362,-8.80243256293661,22.0545662364126));
#28972=CARTESIAN_POINT('Ctrl Pts',(50.083526568362,-8.61241087733861,22.1043384740035));
#28973=CARTESIAN_POINT('Ctrl Pts',(49.9085599813632,-8.52564618972364,22.1155090903777));
#28974=CARTESIAN_POINT('Ctrl Pts',(50.083526568362,-8.75973143359955,21.8754956191941));
#28975=CARTESIAN_POINT('Ctrl Pts',(50.083526568362,-8.59777411058796,21.9297863271335));
#28976=CARTESIAN_POINT('Ctrl Pts',(49.9417488603592,-8.50433615796023,21.9506896748485));
#28977=CARTESIAN_POINT('Ctrl Pts',(50.083526568362,-8.69080155058829,21.7027347500381));
#28978=CARTESIAN_POINT('Ctrl Pts',(50.083526568362,-8.55674861133339,21.7562206122583));
#28979=CARTESIAN_POINT('Ctrl Pts',(49.9736469154778,-8.46983068146547,21.7909000489587));
#28980=CARTESIAN_POINT('Origin',(49.771026568362,-8.87385981233827,22.7876789472104));
#28981=CARTESIAN_POINT('Ctrl Pts',(-49.916473431638,-8.87385981233827,-22.6228153633314));
#28982=CARTESIAN_POINT('Ctrl Pts',(-49.9164734316379,-8.56135981233827,
-22.6228153633314));
#28983=CARTESIAN_POINT('Ctrl Pts',(-49.603973431638,-8.56135981233827,-22.6228153633314));
#28984=CARTESIAN_POINT('Ctrl Pts',(-49.916473431638,-8.87385981115686,-22.4400849131078));
#28985=CARTESIAN_POINT('Ctrl Pts',(-49.916473431638,-8.59410214473059,-22.4645486056717));
#28986=CARTESIAN_POINT('Ctrl Pts',(-49.638510814333,-8.56135981233827,-22.4558719283758));
#28987=CARTESIAN_POINT('Ctrl Pts',(-49.916473431638,-8.86016990857445,-22.2539913434704));
#28988=CARTESIAN_POINT('Ctrl Pts',(-49.9164734316379,-8.61269267441878,
-22.2878011752468));
#28989=CARTESIAN_POINT('Ctrl Pts',(-49.6734793408449,-8.55451485837122,
-22.2853615836368));
#28990=CARTESIAN_POINT('Ctrl Pts',(-49.916473431638,-8.80243256293692,-21.8897026525336));
#28991=CARTESIAN_POINT('Ctrl Pts',(-49.9164734316379,-8.61241087733876,
-21.9394748901251));
#28992=CARTESIAN_POINT('Ctrl Pts',(-49.7415068446392,-8.5256461897237,-21.950645506499));
#28993=CARTESIAN_POINT('Ctrl Pts',(-49.916473431638,-8.75973143359542,-21.7106320353166));
#28994=CARTESIAN_POINT('Ctrl Pts',(-49.9164734316379,-8.59777411058377,
-21.764922743255));
#28995=CARTESIAN_POINT('Ctrl Pts',(-49.7746957236346,-8.5043361579596,-21.7858260909692));
#28996=CARTESIAN_POINT('Ctrl Pts',(-49.916473431638,-8.6908015505883,-21.5378711661591));
#28997=CARTESIAN_POINT('Ctrl Pts',(-49.916473431638,-8.5567486113334,-21.5913570283793));
#28998=CARTESIAN_POINT('Ctrl Pts',(-49.8065937787538,-8.46983068146548,
-21.6260364650797));
#28999=CARTESIAN_POINT('Origin',(-49.603973431638,-8.69080155057987,-21.5378711661599));
#29000=CARTESIAN_POINT('Origin',(-36.1446456971179,-3.61941807409668,-34.3779735205741));
#29001=CARTESIAN_POINT('Origin',(-36.1446456971179,-3.61941807409668,-34.3779735205741));
#29002=CARTESIAN_POINT('Origin',(-36.1446456971182,11.9341984494201,34.5428371044526));
#29003=CARTESIAN_POINT('Origin',(-36.1446456971182,11.9341984494201,34.5428371044526));
#29004=CARTESIAN_POINT('Origin',(-36.7666959739419,12.8136401876617,35.1648873812763));
#29005=CARTESIAN_POINT('Origin',(-36.7666959739419,12.8136401876617,35.1648873812763));
#29006=CARTESIAN_POINT('Origin',(-44.2914734316384,13.4386401876617,44.457431791939));
#29007=CARTESIAN_POINT('Origin',(-44.2914734316384,13.4386401876617,49.769931791939));
#29008=CARTESIAN_POINT('Ctrl Pts',(8.7871565714169,13.0346110567825,49.98761684888));
#29009=CARTESIAN_POINT('Ctrl Pts',(8.77156878298363,13.1253379748597,50.0824317919394));
#29010=CARTESIAN_POINT('Ctrl Pts',(8.74919157458054,13.2555819259033,50.0824317919394));
#29011=CARTESIAN_POINT('Ctrl Pts',(9.16043996894276,13.0670184804062,49.9554115770043));
#29012=CARTESIAN_POINT('Ctrl Pts',(9.15957690651951,13.1643191174805,50.0824317919394));
#29013=CARTESIAN_POINT('Ctrl Pts',(9.12635765894441,13.3203828042395,50.0824317919394));
#29014=CARTESIAN_POINT('Ctrl Pts',(9.53508364729048,13.0885197051924,49.9210761084199));
#29015=CARTESIAN_POINT('Ctrl Pts',(9.54133681365794,13.1804336598308,50.0824317919394));
#29016=CARTESIAN_POINT('Ctrl Pts',(9.50614187595252,13.3633992223637,50.0824317919394));
#29017=CARTESIAN_POINT('Ctrl Pts',(10.2850826537132,13.1183169307001,49.8483267771008));
#29018=CARTESIAN_POINT('Ctrl Pts',(10.2989110791544,13.1821517325912,50.0824317919394));
#29019=CARTESIAN_POINT('Ctrl Pts',(10.2687336993228,13.4229936740979,50.0824317919394));
#29020=CARTESIAN_POINT('Ctrl Pts',(10.6595893630408,13.1261401876617,49.8099934502275));
#29021=CARTESIAN_POINT('Ctrl Pts',(10.6819119767957,13.1638007628797,50.0824317919394));
#29022=CARTESIAN_POINT('Ctrl Pts',(10.6507604421332,13.4386401852138,50.0824317919394));
#29023=CARTESIAN_POINT('Ctrl Pts',(11.0320394968433,13.1261401876617,49.7699317919394));
#29024=CARTESIAN_POINT('Ctrl Pts',(11.0320394968433,13.1261401876617,50.0824317919394));
#29025=CARTESIAN_POINT('Ctrl Pts',(11.0320394968433,13.4386401876617,50.0824317919394));
#29026=CARTESIAN_POINT('Origin',(8.74919157458055,13.2555819259033,49.7699317919394));
#29027=CARTESIAN_POINT('Ctrl Pts',(11.0320394968433,13.1261401876617,49.7699317919394));
#29028=CARTESIAN_POINT('Ctrl Pts',(10.7879063626455,13.1261401876617,49.7961913561371));
#29029=CARTESIAN_POINT('Ctrl Pts',(10.5437266615415,13.1227831409413,49.8216193941525));
#29030=CARTESIAN_POINT('Ctrl Pts',(10.2995429276285,13.1163230257208,49.8462053701604));
#29031=CARTESIAN_POINT('Ctrl Pts',(10.1697230803061,13.1128885169672,49.8592764605253));
#29032=CARTESIAN_POINT('Ctrl Pts',(10.0399016795106,13.1085760632631,49.8721094107857));
#29033=CARTESIAN_POINT('Ctrl Pts',(9.91008314460798,13.1034183933665,49.8847016343491));
#29034=CARTESIAN_POINT('Ctrl Pts',(9.9097828193023,13.1034064614895,49.8847307655005));
#29035=CARTESIAN_POINT('Ctrl Pts',(9.90948249455588,13.1033945253906,49.8847598953115));
#29036=CARTESIAN_POINT('Ctrl Pts',(9.90918217036849,13.1033825850677,49.8847890237822));
#29037=CARTESIAN_POINT('Ctrl Pts',(9.64750791812301,13.0929789105939,49.9101688337043));
#29038=CARTESIAN_POINT('Ctrl Pts',(9.38593410235409,13.0793591824768,49.9345635406361));
#29039=CARTESIAN_POINT('Ctrl Pts',(9.12454731613055,13.0610261309002,49.9579613535261));
#29040=CARTESIAN_POINT('Ctrl Pts',(9.01204656181922,13.0531355938115,49.9680317615884));
#29041=CARTESIAN_POINT('Ctrl Pts',(8.89958052488792,13.044371391851,49.977917398929));
#29042=CARTESIAN_POINT('Ctrl Pts',(8.7871565714169,13.0346110567825,49.98761684888));
#29043=CARTESIAN_POINT('Origin',(39.5861451654569,-8.24885981233827,37.8172834360679));
#29044=CARTESIAN_POINT('Origin',(39.5861451654569,-8.24885981233827,37.8172834360679));
#29045=CARTESIAN_POINT('Origin',(49.7710265683621,-8.87385981233827,0.0824317919395964));
#29046=CARTESIAN_POINT('Origin',(49.7710265683619,-8.87385981233827,36.6697170232579));
#29047=CARTESIAN_POINT('Ctrl Pts',(-49.806390285198,-8.51742571162867,21.9103807300632));
#29048=CARTESIAN_POINT('Ctrl Pts',(-49.9164734316379,-8.60429852763446,
21.8755587571809));
#29049=CARTESIAN_POINT('Ctrl Pts',(-49.916473431638,-8.73841680848988,21.821799675756));
#29050=CARTESIAN_POINT('Ctrl Pts',(-49.8090085275553,-7.81611845087935,
20.1547534124056));
#29051=CARTESIAN_POINT('Ctrl Pts',(-49.9164734316379,-7.905452447202,20.1264636503561));
#29052=CARTESIAN_POINT('Ctrl Pts',(-49.916473431638,-8.03710989934276,20.0721563037169));
#29053=CARTESIAN_POINT('Ctrl Pts',(-49.811505080355,-7.17497856296609,18.3722381388645));
#29054=CARTESIAN_POINT('Ctrl Pts',(-49.916473431638,-7.26440945854389,18.3457771808587));
#29055=CARTESIAN_POINT('Ctrl Pts',(-49.916473431638,-7.39597034001919,18.2960666122331));
#29056=CARTESIAN_POINT('Ctrl Pts',(-49.8148908786805,-6.33083548943257,
15.6694891089486));
#29057=CARTESIAN_POINT('Ctrl Pts',(-49.916473431638,-6.42018164708939,15.643863548684));
#29058=CARTESIAN_POINT('Ctrl Pts',(-49.916473431638,-6.55182731464684,15.6035705286288));
#29059=CARTESIAN_POINT('Ctrl Pts',(-49.8159488661239,-6.07147275224007,
14.7743893106039));
#29060=CARTESIAN_POINT('Ctrl Pts',(-49.9164734316379,-6.1610167959071,14.7499995971314));
#29061=CARTESIAN_POINT('Ctrl Pts',(-49.916473431638,-6.29246464497438,14.7119466567203));
#29062=CARTESIAN_POINT('Ctrl Pts',(-49.8179305761161,-5.59194595832842,
12.9667362137106));
#29063=CARTESIAN_POINT('Ctrl Pts',(-49.9164734316379,-5.68198529154953,
12.9451192661143));
#29064=CARTESIAN_POINT('Ctrl Pts',(-49.916473431638,-5.81293800731357,12.9114646652259));
#29065=CARTESIAN_POINT('Ctrl Pts',(-49.818851928498,-5.37235566849251,12.0558730479342));
#29066=CARTESIAN_POINT('Ctrl Pts',(-49.9164734316379,-5.46255331592529,
12.0355704304617));
#29067=CARTESIAN_POINT('Ctrl Pts',(-49.916473431638,-5.5933477731877,12.0042902846947));
#29068=CARTESIAN_POINT('Ctrl Pts',(-49.8230168203026,-4.39003165639685,
7.49797183341572));
#29069=CARTESIAN_POINT('Ctrl Pts',(-49.916473431638,-4.48357391698338,7.49584681502986));
#29070=CARTESIAN_POINT('Ctrl Pts',(-49.916473431638,-4.6110246353903,7.46517834582782));
#29071=CARTESIAN_POINT('Ctrl Pts',(-49.8249248580392,-3.9693070073482,3.81016121038314));
#29072=CARTESIAN_POINT('Ctrl Pts',(-49.916473431638,-4.0608403985703,3.8033166949147));
#29073=CARTESIAN_POINT('Ctrl Pts',(-49.916473431638,-4.19029955013506,3.79365499210425));
#29074=CARTESIAN_POINT('Ctrl Pts',(-49.8249220643427,-3.96993507524447,
-0.857931554581411));
#29075=CARTESIAN_POINT('Ctrl Pts',(-49.916473431638,-4.06146778743525,-0.85620740371108));
#29076=CARTESIAN_POINT('Ctrl Pts',(-49.916473431638,-4.19092761786416,-0.853767668538309));
#29077=CARTESIAN_POINT('Ctrl Pts',(-49.8248043537542,-3.99635691345978,
-1.79721876196628));
#29078=CARTESIAN_POINT('Ctrl Pts',(-49.9164734316379,-4.08787247118437,
-1.793974725638));
#29079=CARTESIAN_POINT('Ctrl Pts',(-49.916473431638,-4.21734944964593,-1.78889590701665));
#29080=CARTESIAN_POINT('Ctrl Pts',(-49.8243398235277,-4.10112063979829,
-3.66632558149043));
#29081=CARTESIAN_POINT('Ctrl Pts',(-49.916473431638,-4.19252330504738,-3.65967940853563));
#29082=CARTESIAN_POINT('Ctrl Pts',(-49.916473431638,-4.32211313978211,-3.64976555244737));
#29083=CARTESIAN_POINT('Ctrl Pts',(-49.8239941455949,-4.17921237910952,
-4.59529073762686));
#29084=CARTESIAN_POINT('Ctrl Pts',(-49.916473431638,-4.270562939551,-4.58715350637057));
#29085=CARTESIAN_POINT('Ctrl Pts',(-49.916473431638,-4.40020485981034,-4.57465641978639));
#29086=CARTESIAN_POINT('Ctrl Pts',(-49.8226424366985,-4.48691998515858,
-7.36617052593359));
#29087=CARTESIAN_POINT('Ctrl Pts',(-49.916473431638,-4.57807108938205,-7.3542734158373));
#29088=CARTESIAN_POINT('Ctrl Pts',(-49.916473431638,-4.7079123912234,-7.33349441387557));
#29089=CARTESIAN_POINT('Ctrl Pts',(-49.8213206429539,-4.79002518529142,
-9.19205418037808));
#29090=CARTESIAN_POINT('Ctrl Pts',(-49.9164734316379,-4.88128811498848,
-9.17826244785312));
#29091=CARTESIAN_POINT('Ctrl Pts',(-49.916473431638,-5.01101759107685,-9.15159463779479));
#29092=CARTESIAN_POINT('Ctrl Pts',(-49.8180136507671,-5.57013492024956,
-12.8056466912206));
#29093=CARTESIAN_POINT('Ctrl Pts',(-49.916473431638,-5.66058104929807,-12.7859604123856));
#29094=CARTESIAN_POINT('Ctrl Pts',(-49.916473431638,-5.79112706648838,-12.7502963145487));
#29095=CARTESIAN_POINT('Ctrl Pts',(-49.8160298017131,-6.04706234041287,
-14.5933718646951));
#29096=CARTESIAN_POINT('Ctrl Pts',(-49.916473431638,-6.13757065813332,-14.5718489152074));
#29097=CARTESIAN_POINT('Ctrl Pts',(-49.916473431638,-6.26805446129722,-14.5309143455853));
#29098=CARTESIAN_POINT('Ctrl Pts',(-49.8115462443468,-7.16453247036129,
-18.1766274992858));
#29099=CARTESIAN_POINT('Ctrl Pts',(-49.916473431638,-7.25396587946009,-18.1501885883301));
#29100=CARTESIAN_POINT('Ctrl Pts',(-49.916473431638,-7.3855242488532,-18.1005692862277));
#29101=CARTESIAN_POINT('Ctrl Pts',(-49.8090319587906,-7.80982710888312,
-19.9742784910252));
#29102=CARTESIAN_POINT('Ctrl Pts',(-49.916473431638,-7.89920232384119,-19.9460959591859));
#29103=CARTESIAN_POINT('Ctrl Pts',(-49.916473431638,-8.03081819453224,-19.8917334283858));
#29104=CARTESIAN_POINT('Ctrl Pts',(-49.8063885873382,-8.51788060322345,
-21.7466537855478));
#29105=CARTESIAN_POINT('Ctrl Pts',(-49.916473431638,-8.60475296695841,-21.7118303962669));
#29106=CARTESIAN_POINT('Ctrl Pts',(-49.916473431638,-8.73887172590212,-21.6580689256479));
#29107=CARTESIAN_POINT('Origin',(-49.603973431638,-8.69080155057986,21.7027347500388));
#29108=CARTESIAN_POINT('Origin',(0.0835265683620477,-3.61941807409668,0.0824317919394229));
#29109=CARTESIAN_POINT('Origin',(-36.1446456971182,-3.61941807409668,34.5428371044526));
#29110=CARTESIAN_POINT('Origin',(-36.1446456971182,11.4830954176946,34.5428371044526));
#29111=CARTESIAN_POINT('Origin',(-36.1446456971182,-3.61941807409669,34.5428371044526));
#29112=CARTESIAN_POINT('Origin',(-26.1753569081214,12.8136401876617,24.573548315456));
#29113=CARTESIAN_POINT('Origin',(0.0835265683620476,13.4386401876617,49.7699317919394));
#29114=CARTESIAN_POINT('Origin',(-10.8649863601191,13.4386401876617,49.7699317919394));
#29115=CARTESIAN_POINT('Ctrl Pts',(-8.62010343469276,13.0346110567825,49.98761684888));
#29116=CARTESIAN_POINT('Ctrl Pts',(-8.60451564625949,13.1253379748597,50.0824317919394));
#29117=CARTESIAN_POINT('Ctrl Pts',(-8.58213843785641,13.2555819259033,50.0824317919394));
#29118=CARTESIAN_POINT('Ctrl Pts',(-5.74966049737118,12.5435283274364,49.9897363306993));
#29119=CARTESIAN_POINT('Ctrl Pts',(-5.74470440235702,12.6357570952065,50.0824317919394));
#29120=CARTESIAN_POINT('Ctrl Pts',(-5.72384185377314,12.7644980954123,50.0824317919394));
#29121=CARTESIAN_POINT('Ctrl Pts',(-2.85305802790577,12.2852858973025,49.9908996598662));
#29122=CARTESIAN_POINT('Ctrl Pts',(-2.84768070573019,12.3768143018313,50.0824317919394));
#29123=CARTESIAN_POINT('Ctrl Pts',(-2.84005623507672,12.5062567663872,50.0824317919394));
#29124=CARTESIAN_POINT('Ctrl Pts',(1.53450453635747,12.2842756298963,49.9909041527923));
#29125=CARTESIAN_POINT('Ctrl Pts',(1.53184148134384,12.3758051232163,50.0824317919394));
#29126=CARTESIAN_POINT('Ctrl Pts',(1.52808029952419,12.5052464990352,50.0824317919394));
#29127=CARTESIAN_POINT('Ctrl Pts',(3.00840305743394,12.3489547591764,49.9906154596787));
#29128=CARTESIAN_POINT('Ctrl Pts',(3.00380039949013,12.4404805872018,50.0824317919394));
#29129=CARTESIAN_POINT('Ctrl Pts',(2.99545364886012,12.5699256283378,50.0824317919394));
#29130=CARTESIAN_POINT('Ctrl Pts',(5.91737315216722,12.6021248598315,49.9894981615007));
#29131=CARTESIAN_POINT('Ctrl Pts',(5.90753279762978,12.6933787936176,50.0824317919394));
#29132=CARTESIAN_POINT('Ctrl Pts',(5.89169090718009,12.8230957289117,50.0824317919394));
#29133=CARTESIAN_POINT('Ctrl Pts',(7.35844722659859,12.7901838029052,49.9886717813281));
#29134=CARTESIAN_POINT('Ctrl Pts',(7.34671603317829,12.8814125534449,50.0824317919394));
#29135=CARTESIAN_POINT('Ctrl Pts',(7.32653049920342,13.0111545790419,50.0824317919394));
#29136=CARTESIAN_POINT('Ctrl Pts',(8.7871565714169,13.0346110567825,49.98761684888));
#29137=CARTESIAN_POINT('Ctrl Pts',(8.77156878298363,13.1253379748597,50.0824317919394));
#29138=CARTESIAN_POINT('Ctrl Pts',(8.74919157458054,13.2555819259033,50.0824317919394));
#29139=CARTESIAN_POINT('Origin',(-8.58213843785641,13.2555819259033,49.7699317919394));
#29140=CARTESIAN_POINT('Origin',(0.0835265683620477,12.8136401876617,0.0824317919394229));
#29141=CARTESIAN_POINT('Origin',(35.1659821576993,12.8136401876617,36.932654334243));
#29142=CARTESIAN_POINT('Origin',(24.5746430918789,12.8136401876617,26.3413152684227));
#29143=CARTESIAN_POINT('Origin',(35.1659821576993,12.8136401876617,36.932654334243));
#29144=CARTESIAN_POINT('Origin',(41.4050790939509,-8.24885981233827,39.6362173645619));
#29145=CARTESIAN_POINT('Origin',(40.7421664865885,-8.24885981233827,38.9733047571995));
#29146=CARTESIAN_POINT('Origin',(44.4585265683621,-8.87385981233827,44.4574317919394));
#29147=CARTESIAN_POINT('Origin',(44.458526568362,-8.87385981233827,49.7699317919394));
#29148=CARTESIAN_POINT('Ctrl Pts',(-49.603973431638,-8.56135981233827,22.7876789472102));
#29149=CARTESIAN_POINT('Ctrl Pts',(-49.9164734316379,-8.56135981233827,
22.7876789472102));
#29150=CARTESIAN_POINT('Ctrl Pts',(-49.916473431638,-8.87385981233827,22.7876789472102));
#29151=CARTESIAN_POINT('Ctrl Pts',(-49.6390045861426,-8.56135981233827,
22.6183487659333));
#29152=CARTESIAN_POINT('Ctrl Pts',(-49.916473431638,-8.59454828035616,22.6272556847667));
#29153=CARTESIAN_POINT('Ctrl Pts',(-49.916473431638,-8.87385980853143,22.6023407515994));
#29154=CARTESIAN_POINT('Ctrl Pts',(-49.6734801841997,-8.55449257599332,
22.4502169429184));
#29155=CARTESIAN_POINT('Ctrl Pts',(-49.916473431638,-8.61264419244186,22.4525914296835));
#29156=CARTESIAN_POINT('Ctrl Pts',(-49.916473431638,-8.86012534447556,22.4188473554127));
#29157=CARTESIAN_POINT('Ctrl Pts',(-49.7412291075803,-8.52578588737898,
22.1168796998391));
#29158=CARTESIAN_POINT('Ctrl Pts',(-49.916473431638,-8.61245644138859,22.1057145740718));
#29159=CARTESIAN_POINT('Ctrl Pts',(-49.916473431638,-8.80271195759251,22.0560565673691));
#29160=CARTESIAN_POINT('Ctrl Pts',(-49.7747457482377,-8.50428205216085,
21.9504391022727));
#29161=CARTESIAN_POINT('Ctrl Pts',(-49.916473431636,-8.59771167170006,21.9295221097184));
#29162=CARTESIAN_POINT('Ctrl Pts',(-49.916473431638,-8.75963242031971,21.8752474200655));
#29163=CARTESIAN_POINT('Ctrl Pts',(-49.8065937787556,-8.46983068145906,
21.7909000489602));
#29164=CARTESIAN_POINT('Ctrl Pts',(-49.916473431638,-8.55674861132667,21.7562206122594));
#29165=CARTESIAN_POINT('Ctrl Pts',(-49.916473431638,-8.69080155057985,21.7027347500388));
#29166=CARTESIAN_POINT('Origin',(-49.603973431638,-8.87385981233827,22.7876789472102));
#29167=CARTESIAN_POINT('Ctrl Pts',(-49.8065937787556,-8.46983068145906,
21.7909000489602));
#29168=CARTESIAN_POINT('Ctrl Pts',(-49.7963235078174,-8.48094048097799,
21.8423478177927));
#29169=CARTESIAN_POINT('Ctrl Pts',(-49.7859728826426,-8.49060780497133,
21.8940472511784));
#29170=CARTESIAN_POINT('Ctrl Pts',(-49.775563128702,-8.49910612137133,21.9458948974734));
#29171=CARTESIAN_POINT('Ctrl Pts',(-49.764379289321,-8.50823638575309,22.0015980151221));
#29172=CARTESIAN_POINT('Ctrl Pts',(-49.7531270731297,-8.51601690934008,
22.0574729005677));
#29173=CARTESIAN_POINT('Ctrl Pts',(-49.741824971166,-8.52273612856652,22.1134260010429));
#29174=CARTESIAN_POINT('Ctrl Pts',(-49.7303817060214,-8.52953927079792,
22.1700779553834));
#29175=CARTESIAN_POINT('Ctrl Pts',(-49.7188870758208,-8.53525345256675,
22.2268112355569));
#29176=CARTESIAN_POINT('Ctrl Pts',(-49.7073553886521,-8.54013948886813,
22.2835482806785));
#29177=CARTESIAN_POINT('Ctrl Pts',(-49.7070885620479,-8.54025254469902,
22.2848610940475));
#29178=CARTESIAN_POINT('Ctrl Pts',(-49.706821700383,-8.54036513501698,22.2861739864676));
#29179=CARTESIAN_POINT('Ctrl Pts',(-49.7065548032017,-8.54047726034838,
22.287486960151));
#29180=CARTESIAN_POINT('Ctrl Pts',(-49.6793313303115,-8.55191402751557,
22.4214100810567));
#29181=CARTESIAN_POINT('Ctrl Pts',(-49.6518481112244,-8.5584728839653,22.5556485348429));
#29182=CARTESIAN_POINT('Ctrl Pts',(-49.6241123555729,-8.56059423319272,
22.6901689000943));
#29183=CARTESIAN_POINT('Ctrl Pts',(-49.6174141089786,-8.56110654374291,
22.7226558670884));
#29184=CARTESIAN_POINT('Ctrl Pts',(-49.6107011130711,-8.56135981233827,
22.7551593362476));
#29185=CARTESIAN_POINT('Ctrl Pts',(-49.603973431638,-8.56135981233827,22.7876789472102));
#29186=CARTESIAN_POINT('Origin',(-36.1446456971182,-3.61941807409668,34.5428371044526));
#29187=CARTESIAN_POINT('Origin',(-36.1446456971182,-3.61941807409668,34.5428371044526));
#29188=CARTESIAN_POINT('Ctrl Pts',(-10.8649863601191,13.1261401876617,49.7699317919394));
#29189=CARTESIAN_POINT('Ctrl Pts',(-10.8649863601191,13.1261401876617,50.0824317919394));
#29190=CARTESIAN_POINT('Ctrl Pts',(-10.8649863601191,13.4386401876617,50.0824317919394));
#29191=CARTESIAN_POINT('Ctrl Pts',(-10.4914375950611,13.1261401876617,49.8101116217086));
#29192=CARTESIAN_POINT('Ctrl Pts',(-10.5138842101856,13.1639055963027,50.0824317919394));
#29193=CARTESIAN_POINT('Ctrl Pts',(-10.4825839193318,13.4386401851022,50.0824317919394));
#29194=CARTESIAN_POINT('Ctrl Pts',(-10.1172066156767,13.1182927286051,49.8484089205029));
#29195=CARTESIAN_POINT('Ctrl Pts',(-10.1310095155991,13.1821712224816,50.0824317919381));
#29196=CARTESIAN_POINT('Ctrl Pts',(-10.1008424173742,13.4229452699553,50.0824317919394));
#29197=CARTESIAN_POINT('Ctrl Pts',(-9.36754573057138,13.0884919386939,49.921120805052));
#29198=CARTESIAN_POINT('Ctrl Pts',(-9.37377765929087,13.180412811403,50.0824317919407));
#29199=CARTESIAN_POINT('Ctrl Pts',(-9.33859724908609,13.3633436893193,50.0824317919394));
#29200=CARTESIAN_POINT('Ctrl Pts',(-8.99271962453602,13.0669605544565,49.955469139931));
#29201=CARTESIAN_POINT('Ctrl Pts',(-8.99180823791993,13.1642472289417,50.0824317919394));
#29202=CARTESIAN_POINT('Ctrl Pts',(-8.95863183223867,13.3202672259815,50.0824317919394));
#29203=CARTESIAN_POINT('Ctrl Pts',(-8.62010343469179,13.0346110567867,49.9876168488787));
#29204=CARTESIAN_POINT('Ctrl Pts',(-8.60451564625867,13.125337974864,50.0824317919394));
#29205=CARTESIAN_POINT('Ctrl Pts',(-8.58213843785567,13.2555819259088,50.0824317919394));
#29206=CARTESIAN_POINT('Ctrl Pts',(-8.62010343469228,13.0346110567867,49.9876168488786));
#29207=CARTESIAN_POINT('Ctrl Pts',(-8.83743262669382,13.0534789729962,49.9688666310144));
#29208=CARTESIAN_POINT('Ctrl Pts',(-9.05495247870489,13.0686233597136,49.9494169416172));
#29209=CARTESIAN_POINT('Ctrl Pts',(-9.27257311703778,13.0809296717971,49.9292822276746));
#29210=CARTESIAN_POINT('Ctrl Pts',(-9.42907418117352,13.0897797098789,49.9148024238186));
#29211=CARTESIAN_POINT('Ctrl Pts',(-9.5856278909298,13.0971603804829,49.8999681158358));
#29212=CARTESIAN_POINT('Ctrl Pts',(-9.74220410542708,13.1033855068804,49.884781586804));
#29213=CARTESIAN_POINT('Ctrl Pts',(-9.74226146095453,13.1033877872102,49.8847760238175));
#29214=CARTESIAN_POINT('Ctrl Pts',(-9.74231881649497,13.1033900673852,49.8847704607826));
#29215=CARTESIAN_POINT('Ctrl Pts',(-9.74237617204842,13.1033923474055,49.8847648976995));
#29216=CARTESIAN_POINT('Ctrl Pts',(-10.1166203384253,13.1182694471954,49.8484658598822));
#29217=CARTESIAN_POINT('Ctrl Pts',(-10.4908161997162,13.1261401876617,49.8101784605299));
#29218=CARTESIAN_POINT('Ctrl Pts',(-10.8649863601191,13.1261401876617,49.7699317919394));
#29219=CARTESIAN_POINT('Origin',(35.1659821576993,12.8136401876617,36.932654334243));
#29220=CARTESIAN_POINT('Origin',(35.1659821576993,12.8136401876617,36.932654334243));
#29221=CARTESIAN_POINT('Origin',(39.8582830101054,-8.24885981233827,39.8571882336827));
#29222=CARTESIAN_POINT('Origin',(38.9743995336222,-8.24885981233827,40.7410717101659));
#29223=CARTESIAN_POINT('Origin',(0.0835265683620476,-8.87385981233827,49.7699317919394));
#29224=CARTESIAN_POINT('Origin',(22.7887737236329,-8.87385981233827,49.7699317919394));
#29225=CARTESIAN_POINT('Origin',(-49.603973431638,-8.87385981233827,0.0824317919394229));
#29226=CARTESIAN_POINT('Origin',(-49.603973431638,-8.87385981233827,44.4574317919389));
#29227=CARTESIAN_POINT('Origin',(0.0835265683620477,-8.24885981233827,0.0824317919394229));
#29228=CARTESIAN_POINT('Origin',(-39.4190920287332,-8.24885981233827,37.8172834360675));
#29229=CARTESIAN_POINT('Ctrl Pts',(-39.2593077130565,-8.4698306814591,37.6646495687126));
#29230=CARTESIAN_POINT('Ctrl Pts',(-39.0443992301308,-8.46631238203738,
37.8845323757067));
#29231=CARTESIAN_POINT('Ctrl Pts',(-39.1981211596124,-8.2488598123383,38.0382543051883));
#29232=CARTESIAN_POINT('Ctrl Pts',(-38.1677401528071,-6.92666471828265,
36.5732839934435));
#29233=CARTESIAN_POINT('Ctrl Pts',(-37.9532471818617,-6.9233956438625,36.7933803274376));
#29234=CARTESIAN_POINT('Ctrl Pts',(-38.1066522799251,-6.70569384849333,
36.946785425501));
#29235=CARTESIAN_POINT('Ctrl Pts',(-37.0761523844497,-5.38351572788325,
35.4819151782211));
#29236=CARTESIAN_POINT('Ctrl Pts',(-36.8618908744297,-5.38020745678036,
35.7020240200208));
#29237=CARTESIAN_POINT('Ctrl Pts',(-37.0151713871424,-5.16254485803799,
35.8553045327183));
#29238=CARTESIAN_POINT('Ctrl Pts',(-35.984538282875,-3.84038894321749,34.3905421902094));
#29239=CARTESIAN_POINT('Ctrl Pts',(-35.7701869713607,-3.8365505471153,34.6103201169366));
#29240=CARTESIAN_POINT('Ctrl Pts',(-35.9236748279975,-3.61941807409669,
34.7638079735734));
#29241=CARTESIAN_POINT('Origin',(-39.4190920287332,-8.24885981233827,37.8172834360675));
#29242=CARTESIAN_POINT('Origin',(-24.407589955155,12.8136401876617,26.3413152684223));
#29243=CARTESIAN_POINT('Origin',(-34.9989290209756,12.8136401876617,36.9326543342427));
#29244=CARTESIAN_POINT('Origin',(0.0835265683620477,12.8136401876617,0.0824317919394229));
#29245=CARTESIAN_POINT('Origin',(-34.9989290209756,12.8136401876617,36.9326543342427));
#29246=CARTESIAN_POINT('Origin',(34.8549575729643,12.3739187291566,36.6216294748833));
#29247=CARTESIAN_POINT('Origin',(34.5439318808756,11.9341984494202,36.3106040574193));
#29248=CARTESIAN_POINT('Origin',(39.6373121409846,-8.24885981233827,41.4039843175283));
#29249=CARTESIAN_POINT('Origin',(37.8183782124906,-8.24885981233827,39.5850503890343));
#29250=CARTESIAN_POINT('Origin',(0.0835265683620477,-8.24885981233827,0.0824317919394229));
#29251=CARTESIAN_POINT('Ctrl Pts',(22.7887737236329,-8.56135981233827,49.7699317919394));
#29252=CARTESIAN_POINT('Ctrl Pts',(22.6541181864147,-8.56135981233827,49.7977894301704));
#29253=CARTESIAN_POINT('Ctrl Pts',(22.5197384329217,-8.55702114807029,49.8253956090288));
#29254=CARTESIAN_POINT('Ctrl Pts',(22.3856647415717,-8.54791555690698,49.8527441922136));
#29255=CARTESIAN_POINT('Ctrl Pts',(22.3532856491678,-8.54571653654214,49.8593489354196));
#29256=CARTESIAN_POINT('Ctrl Pts',(22.3209244662425,-8.54323926489437,49.8659386346358));
#29257=CARTESIAN_POINT('Ctrl Pts',(22.2885817365737,-8.54047726034825,49.8725131635028));
#29258=CARTESIAN_POINT('Ctrl Pts',(22.2872687628902,-8.54036513501685,49.872780060684));
#29259=CARTESIAN_POINT('Ctrl Pts',(22.2859558704701,-8.54025254469889,49.873046922349));
#29260=CARTESIAN_POINT('Ctrl Pts',(22.2846430571011,-8.54013948886801,49.8733137489532));
#29261=CARTESIAN_POINT('Ctrl Pts',(22.22312560482,-8.5348417772165,49.8858170439981));
#29262=CARTESIAN_POINT('Ctrl Pts',(22.1616123554514,-8.52857105445296,49.8982768361997));
#29263=CARTESIAN_POINT('Ctrl Pts',(22.1002028692077,-8.52099310668482,49.9106746950791));
#29264=CARTESIAN_POINT('Ctrl Pts',(22.0472505817754,-8.51445877961403,49.9213651441788));
#29265=CARTESIAN_POINT('Ctrl Pts',(21.994374806306,-8.50695259656895,49.9320096488017));
#29266=CARTESIAN_POINT('Ctrl Pts',(21.9416562445106,-8.49822768693266,49.9425922088684));
#29267=CARTESIAN_POINT('Ctrl Pts',(21.8915966824201,-8.48994284112507,49.9526410096075));
#29268=CARTESIAN_POINT('Ctrl Pts',(21.8416783185839,-8.48055949752612,49.9626340619876));
#29269=CARTESIAN_POINT('Ctrl Pts',(21.7919948253829,-8.46983068145907,49.9725521390571));
#29270=CARTESIAN_POINT('Origin',(37.8183782124906,-8.24885981233827,39.5850503890343));
#29271=CARTESIAN_POINT('Ctrl Pts',(22.7887737236329,-8.56135981233827,49.7699317919394));
#29272=CARTESIAN_POINT('Ctrl Pts',(22.7887737236329,-8.56135981233827,50.0824317919394));
#29273=CARTESIAN_POINT('Ctrl Pts',(22.7887737236329,-8.87385981233827,50.0824317919394));
#29274=CARTESIAN_POINT('Ctrl Pts',(22.6194435423556,-8.56135981233827,49.8049629464425));
#29275=CARTESIAN_POINT('Ctrl Pts',(22.6283504611892,-8.59454828035467,50.0824317919394));
#29276=CARTESIAN_POINT('Ctrl Pts',(22.6034355280221,-8.87385980853143,50.0824317919394));
#29277=CARTESIAN_POINT('Ctrl Pts',(22.451311719341,-8.55449257599307,49.8394385445005));
#29278=CARTESIAN_POINT('Ctrl Pts',(22.453686206106,-8.61264419244103,50.0824317919394));
#29279=CARTESIAN_POINT('Ctrl Pts',(22.4199421318354,-8.86012534447524,50.0824317919394));
#29280=CARTESIAN_POINT('Ctrl Pts',(22.1179744762618,-8.52578588737924,49.9071874678825));
#29281=CARTESIAN_POINT('Ctrl Pts',(22.1068093504948,-8.61245644138935,50.0824317919394));
#29282=CARTESIAN_POINT('Ctrl Pts',(22.0571513437917,-8.80271195759283,50.0824317919394));
#29283=CARTESIAN_POINT('Ctrl Pts',(21.9515338786954,-8.5042820521619,49.9407041085403));
#29284=CARTESIAN_POINT('Ctrl Pts',(21.930616886141,-8.59771167169906,50.0824317919394));
#29285=CARTESIAN_POINT('Ctrl Pts',(21.876342196488,-8.75963242031969,50.0824317919394));
#29286=CARTESIAN_POINT('Ctrl Pts',(21.7919948253829,-8.46983068145907,49.9725521390571));
#29287=CARTESIAN_POINT('Ctrl Pts',(21.757315388682,-8.55674861132668,50.0824317919394));
#29288=CARTESIAN_POINT('Ctrl Pts',(21.7038295264614,-8.69080155057986,50.0824317919394));
#29289=CARTESIAN_POINT('Origin',(21.7038295264614,-8.69080155057986,49.7699317919394));
#29290=CARTESIAN_POINT('Origin',(-44.2914734316384,-8.87385981233827,44.457431791939));
#29291=CARTESIAN_POINT('Origin',(-44.2914734316384,-8.87385981233827,49.769931791939));
#29292=CARTESIAN_POINT('Origin',(-39.4190920287332,-8.24885981233827,37.8172834360675));
#29293=CARTESIAN_POINT('Origin',(-39.4190920287332,-8.24885981233827,37.8172834360675));
#29294=CARTESIAN_POINT('Origin',(-34.9989290209756,12.8136401876617,36.9326543342427));
#29295=CARTESIAN_POINT('Origin',(-34.9989290209756,12.8136401876617,36.9326543342427));
#29296=CARTESIAN_POINT('Origin',(34.5439318808756,11.9341984494201,36.3106040574193));
#29297=CARTESIAN_POINT('Origin',(34.5439318808756,11.9341984494201,36.3106040574193));
#29298=CARTESIAN_POINT('Origin',(37.8183782124906,-8.24885981233827,39.5850503890343));
#29299=CARTESIAN_POINT('Origin',(37.8183782124906,-8.24885981233827,39.5850503890343));
#29300=CARTESIAN_POINT('Ctrl Pts',(-21.7449659867426,-8.77420095360317,
50.0824317919394));
#29301=CARTESIAN_POINT('Ctrl Pts',(-21.798926229011,-8.64003310969503,50.0824317919394));
#29302=CARTESIAN_POINT('Ctrl Pts',(-21.8338566105543,-8.55319446981481,
49.9721960693566));
#29303=CARTESIAN_POINT('Ctrl Pts',(-18.2490305748135,-7.36815837377856,
50.0824317919394));
#29304=CARTESIAN_POINT('Ctrl Pts',(-18.3130464386012,-7.24249091567042,
50.0824317919394));
#29305=CARTESIAN_POINT('Ctrl Pts',(-18.3259998716927,-7.14715496161882,
49.9774388543335));
#29306=CARTESIAN_POINT('Ctrl Pts',(-14.6840632078164,-6.21561709199713,
50.0824317919394));
#29307=CARTESIAN_POINT('Ctrl Pts',(-14.7335250825033,-6.08656532570595,
50.0824317919394));
#29308=CARTESIAN_POINT('Ctrl Pts',(-14.7474057099706,-5.99460855782839,
49.9821571538487));
#29309=CARTESIAN_POINT('Ctrl Pts',(-9.22874352618438,-5.02557369219655,
50.0824317919394));
#29310=CARTESIAN_POINT('Ctrl Pts',(-9.25561217772287,-4.89581925234152,
50.0824317919394));
#29311=CARTESIAN_POINT('Ctrl Pts',(-9.26953608557641,-4.8045652666467,49.9871995617052));
#29312=CARTESIAN_POINT('Ctrl Pts',(-7.41133500973276,-4.71947214408047,
50.0824317919394));
#29313=CARTESIAN_POINT('Ctrl Pts',(-7.43234648598233,-4.58961053626118,
50.0824317919394));
#29314=CARTESIAN_POINT('Ctrl Pts',(-7.44435366976549,-4.4984637156113,49.9885338203398));
#29315=CARTESIAN_POINT('Ctrl Pts',(-4.64537610952596,-4.40691837826605,
50.0824317919394));
#29316=CARTESIAN_POINT('Ctrl Pts',(-4.65806729858047,-4.27725721313721,
50.0824317919394));
#29317=CARTESIAN_POINT('Ctrl Pts',(-4.66632727320178,-4.18590981848828,
49.9899065809487));
#29318=CARTESIAN_POINT('Ctrl Pts',(-3.71666105631754,-4.327158062246,50.0824317919394));
#29319=CARTESIAN_POINT('Ctrl Pts',(-3.72675911584482,-4.19755005843067,
50.0824317919394));
#29320=CARTESIAN_POINT('Ctrl Pts',(-3.73352231198055,-4.1061494680647,49.9902596193181));
#29321=CARTESIAN_POINT('Ctrl Pts',(-1.84550713430984,-4.21946011836696,
50.0824317919394));
#29322=CARTESIAN_POINT('Ctrl Pts',(-1.8507435419627,-4.08996813963968,50.0824317919394));
#29323=CARTESIAN_POINT('Ctrl Pts',(-1.85408687661129,-3.99845145937572,
49.9907371683897));
#29324=CARTESIAN_POINT('Ctrl Pts',(-0.912269960149392,-4.19205938565825,
50.0824317919394));
#29325=CARTESIAN_POINT('Ctrl Pts',(-0.914869480160837,-4.06258497561498,
50.0824317919394));
#29326=CARTESIAN_POINT('Ctrl Pts',(-0.91669922368614,-3.9710507150748,49.9908592564268));
#29327=CARTESIAN_POINT('Ctrl Pts',(3.74233330481107,-4.18598197768416,50.0824317919394));
#29328=CARTESIAN_POINT('Ctrl Pts',(3.75179154006485,-4.05651422028119,50.0824317919394));
#29329=CARTESIAN_POINT('Ctrl Pts',(3.75860756853322,-3.96497330343863,49.9908862940722));
#29330=CARTESIAN_POINT('Ctrl Pts',(7.42861042436576,-4.60394036704883,50.0824317919394));
#29331=CARTESIAN_POINT('Ctrl Pts',(7.45931217637961,-4.47650762044643,50.0824317919394));
#29332=CARTESIAN_POINT('Ctrl Pts',(7.46124533724433,-4.38293092071028,49.9889892256309));
#29333=CARTESIAN_POINT('Ctrl Pts',(11.9953617287628,-5.59091481619281,50.0824317919394));
#29334=CARTESIAN_POINT('Ctrl Pts',(12.0266282204217,-5.46011080390181,50.0824317919394));
#29335=CARTESIAN_POINT('Ctrl Pts',(12.0469073010734,-5.36990690683472,49.984803391475));
#29336=CARTESIAN_POINT('Ctrl Pts',(12.9059760664518,-5.81129472998947,50.0824317919394));
#29337=CARTESIAN_POINT('Ctrl Pts',(12.9396172744353,-5.68032983292117,50.0824317919394));
#29338=CARTESIAN_POINT('Ctrl Pts',(12.9612247995486,-5.59028691905869,49.9838785470594));
#29339=CARTESIAN_POINT('Ctrl Pts',(14.7061033059095,-6.29050753230872,50.0824317919394));
#29340=CARTESIAN_POINT('Ctrl Pts',(14.7441427204447,-6.15904772772697,50.0824317919394));
#29341=CARTESIAN_POINT('Ctrl Pts',(14.7685229600323,-6.06949999371254,49.9818976821262));
#29342=CARTESIAN_POINT('Ctrl Pts',(15.5979075859762,-6.54980455615392,50.0824317919394));
#29343=CARTESIAN_POINT('Ctrl Pts',(15.6381893611325,-6.41814737484953,50.0824317919394));
#29344=CARTESIAN_POINT('Ctrl Pts',(15.6638045210804,-6.32879713521949,49.9808397055944));
#29345=CARTESIAN_POINT('Ctrl Pts',(18.2508522029681,-7.38126084278977,50.0824317919394));
#29346=CARTESIAN_POINT('Ctrl Pts',(18.3002836337393,-7.24964619597268,50.0824317919394));
#29347=CARTESIAN_POINT('Ctrl Pts',(18.3268527946815,-7.16025352121961,49.9775040185271));
#29348=CARTESIAN_POINT('Ctrl Pts',(19.9895860300914,-8.00683451481104,50.0824317919394));
#29349=CARTESIAN_POINT('Ctrl Pts',(20.043507385477,-7.87510646586172,50.0824317919394));
#29350=CARTESIAN_POINT('Ctrl Pts',(20.0718858539989,-7.78582757943738,49.9750659873749));
#29351=CARTESIAN_POINT('Ctrl Pts',(21.7038295264614,-8.69080155057986,50.0824317919394));
#29352=CARTESIAN_POINT('Ctrl Pts',(21.7573285588578,-8.55671560258926,50.0824317919394));
#29353=CARTESIAN_POINT('Ctrl Pts',(21.7920088993551,-8.46979540751453,49.9725075380777));
#29354=CARTESIAN_POINT('Origin',(-21.5367763897373,-8.69080155057986,49.7699317919394));
#29355=CARTESIAN_POINT('Origin',(0.0835265683620476,-8.87385981233827,49.7699317919394));
#29356=CARTESIAN_POINT('Origin',(-22.6217205869088,-8.87385981233827,49.7699317919394));
#29357=CARTESIAN_POINT('Origin',(-41.2380259572272,-8.24885981233827,39.6362173645615));
#29358=CARTESIAN_POINT('Origin',(-40.5751133498648,-8.24885981233827,38.9733047571991));
#29359=CARTESIAN_POINT('Origin',(-34.6879038942329,12.3739193162068,36.621629186931));
#29360=CARTESIAN_POINT('Origin',(-34.3768787441519,11.9341984494201,36.310604057419));
#29361=CARTESIAN_POINT('Origin',(34.5439318808756,11.4830954176946,36.3106040574193));
#29362=CARTESIAN_POINT('Origin',(34.5439318808756,-3.61941807409669,36.3106040574193));
#29363=CARTESIAN_POINT('Ctrl Pts',(37.6657443451356,-8.46983068145905,39.4252660733575));
#29364=CARTESIAN_POINT('Ctrl Pts',(37.8856271521297,-8.46631238203734,39.2103575904319));
#29365=CARTESIAN_POINT('Ctrl Pts',(38.0393490816113,-8.24885981233825,39.3640795199135));
#29366=CARTESIAN_POINT('Ctrl Pts',(36.5743787698899,-6.92666471828331,38.3336985130867));
#29367=CARTESIAN_POINT('Ctrl Pts',(36.7944751038716,-6.92339564388109,38.1192055421283));
#29368=CARTESIAN_POINT('Ctrl Pts',(36.9478802019155,-6.70569384850732,38.2726106402177));
#29369=CARTESIAN_POINT('Ctrl Pts',(35.4830099546367,-5.38351572788366,37.2421107447585));
#29370=CARTESIAN_POINT('Ctrl Pts',(35.7031187964357,-5.38020745678172,37.0278492347378));
#29371=CARTESIAN_POINT('Ctrl Pts',(35.8563993091415,-5.16254485803843,37.1811297474436));
#29372=CARTESIAN_POINT('Ctrl Pts',(34.3916369666324,-3.84038894321749,36.1504966431761));
#29373=CARTESIAN_POINT('Ctrl Pts',(34.6114148933596,-3.8365505471153,35.9361453316618));
#29374=CARTESIAN_POINT('Ctrl Pts',(34.7649027499964,-3.61941807409669,36.0896331882986));
#29375=CARTESIAN_POINT('Origin',(34.5439318808756,-3.61941807409668,36.3106040574193));
#29376=CARTESIAN_POINT('Ctrl Pts',(-22.6217205869088,-8.87385981233827,
50.0824317919394));
#29377=CARTESIAN_POINT('Ctrl Pts',(-22.6217205869088,-8.56135981233826,
50.0824317919394));
#29378=CARTESIAN_POINT('Ctrl Pts',(-22.6217205869088,-8.56135981233827,
49.7699317919394));
#29379=CARTESIAN_POINT('Ctrl Pts',(-22.438990136685,-8.87385981115686,50.0824317919394));
#29380=CARTESIAN_POINT('Ctrl Pts',(-22.4634538292487,-8.59410214473108,
50.0824317919394));
#29381=CARTESIAN_POINT('Ctrl Pts',(-22.4547771519531,-8.56135981233827,
49.8044691746351));
#29382=CARTESIAN_POINT('Ctrl Pts',(-22.2528965670481,-8.86016990857445,
50.0824317919394));
#29383=CARTESIAN_POINT('Ctrl Pts',(-22.2867063988249,-8.61269267441879,
50.0824317919388));
#29384=CARTESIAN_POINT('Ctrl Pts',(-22.2842668072145,-8.55451485837127,
49.8394377011463));
#29385=CARTESIAN_POINT('Ctrl Pts',(-21.8886078761106,-8.80243256293693,
50.0824317919394));
#29386=CARTESIAN_POINT('Ctrl Pts',(-21.9383801137018,-8.61241087733877,
50.08243179194));
#29387=CARTESIAN_POINT('Ctrl Pts',(-21.9495507300761,-8.52564618972366,
49.9074652049407));
#29388=CARTESIAN_POINT('Ctrl Pts',(-21.7095372588941,-8.7597314335958,50.0824317919394));
#29389=CARTESIAN_POINT('Ctrl Pts',(-21.7638279668325,-8.59777411058506,
50.0824317919414));
#29390=CARTESIAN_POINT('Ctrl Pts',(-21.7847313145468,-8.50433615796108,
49.9406540839376));
#29391=CARTESIAN_POINT('Ctrl Pts',(-21.5367763897364,-8.69080155058829,
50.0824317919394));
#29392=CARTESIAN_POINT('Ctrl Pts',(-21.5902622519567,-8.5567486113334,50.0824317919394));
#29393=CARTESIAN_POINT('Ctrl Pts',(-21.624941688657,-8.46983068146548,49.9725521390553));
#29394=CARTESIAN_POINT('Ctrl Pts',(-22.6217205869088,-8.56135981233827,
49.7699317919394));
#29395=CARTESIAN_POINT('Ctrl Pts',(-22.5570649108185,-8.56135981233827,
49.7833078065708));
#29396=CARTESIAN_POINT('Ctrl Pts',(-22.4923868342644,-8.56033639109561,
49.7966425973418));
#29397=CARTESIAN_POINT('Ctrl Pts',(-22.4277520323567,-8.55827526792405,
49.8099240615446));
#29398=CARTESIAN_POINT('Ctrl Pts',(-22.3612333428163,-8.55615406992689,
49.8235926358711));
#29399=CARTESIAN_POINT('Ctrl Pts',(-22.2947577095333,-8.552934288094,49.8372053106334));
#29400=CARTESIAN_POINT('Ctrl Pts',(-22.2283761570625,-8.54855443110404,
49.8507510984659));
#29401=CARTESIAN_POINT('Ctrl Pts',(-22.1925472882174,-8.5461904411729,49.8580623202977));
#29402=CARTESIAN_POINT('Ctrl Pts',(-22.1567457285975,-8.54348767314343,
49.8653540415904));
#29403=CARTESIAN_POINT('Ctrl Pts',(-22.1209815952407,-8.54043032524651,
49.8726238531984));
#29404=CARTESIAN_POINT('Ctrl Pts',(-22.1196238899022,-8.54031425987119,
49.8728998353376));
#29405=CARTESIAN_POINT('Ctrl Pts',(-22.1182662759902,-8.54019768609479,
49.8731757782021));
#29406=CARTESIAN_POINT('Ctrl Pts',(-22.1169087561037,-8.54008060317761,
49.8734516812435));
#29407=CARTESIAN_POINT('Ctrl Pts',(-22.0497247180194,-8.53428613692706,
49.8871061997702));
#29408=CARTESIAN_POINT('Ctrl Pts',(-21.9826706468966,-8.5273633766299,49.9006844600952));
#29409=CARTESIAN_POINT('Ctrl Pts',(-21.9157941683003,-8.51884310578637,
49.914177934353));
#29410=CARTESIAN_POINT('Ctrl Pts',(-21.8545644066734,-8.51104224420251,
49.9265320868094));
#29411=CARTESIAN_POINT('Ctrl Pts',(-21.7934834053665,-8.50190252011177,
49.9388151779388));
#29412=CARTESIAN_POINT('Ctrl Pts',(-21.7326032971608,-8.49102344833061,
49.9510170411214));
#29413=CARTESIAN_POINT('Ctrl Pts',(-21.6966410620796,-8.48459711716286,
49.9582247528869));
#29414=CARTESIAN_POINT('Ctrl Pts',(-21.6607492307147,-8.47756307924556,
49.9654040514526));
#29415=CARTESIAN_POINT('Ctrl Pts',(-21.624941688657,-8.46983068146548,49.9725521390553));
#29416=CARTESIAN_POINT('Origin',(-39.6912298733817,-8.24885981233827,39.8571882336823));
#29417=CARTESIAN_POINT('Origin',(-38.8073463968985,-8.24885981233827,40.7410717101655));
#29418=CARTESIAN_POINT('Origin',(-34.3768787441519,11.9341984494201,36.310604057419));
#29419=CARTESIAN_POINT('Origin',(-34.3768787441519,11.9341984494202,36.310604057419));
#29420=CARTESIAN_POINT('Origin',(34.5439318808756,-3.61941807409668,36.3106040574193));
#29421=CARTESIAN_POINT('Origin',(0.0835265683620477,-8.24885981233827,0.0824317919394229));
#29422=CARTESIAN_POINT('Origin',(-37.6513250757669,-8.24885981233827,39.5850503890339));
#29423=CARTESIAN_POINT('Origin',(-39.4702590042609,-8.24885981233827,41.4039843175279));
#29424=CARTESIAN_POINT('Origin',(-37.6513250757669,-8.24885981233827,39.5850503890339));
#29425=CARTESIAN_POINT('Origin',(-34.3768787441519,11.4830954176946,36.310604057419));
#29426=CARTESIAN_POINT('Origin',(-34.3768787441519,-3.61941807409668,36.310604057419));
#29427=CARTESIAN_POINT('Origin',(-37.6513250757669,-8.24885981233827,39.5850503890339));
#29428=CARTESIAN_POINT('Origin',(-37.6513250757669,-8.24885981233827,39.5850503890339));
#29429=CARTESIAN_POINT('Origin',(-34.3768787441519,-3.61941807409668,36.310604057419));
#29430=CARTESIAN_POINT('Origin',(-34.3768787441519,-3.61941807409669,36.310604057419));
#29431=CARTESIAN_POINT('Ctrl Pts',(-37.8722959448876,-8.24885981233824,
39.3640795199131));
#29432=CARTESIAN_POINT('Ctrl Pts',(-37.718574015406,-8.46631238203733,39.2103575904315));
#29433=CARTESIAN_POINT('Ctrl Pts',(-37.4986912084119,-8.46983068145904,
39.4252660733572));
#29434=CARTESIAN_POINT('Ctrl Pts',(-36.7808270651937,-6.70569384850457,
38.2726106402191));
#29435=CARTESIAN_POINT('Ctrl Pts',(-36.6274219671306,-6.92339564387865,
38.1192055421485));
#29436=CARTESIAN_POINT('Ctrl Pts',(-36.40732563317,-6.92666471828328,38.3336985130827));
#29437=CARTESIAN_POINT('Ctrl Pts',(-35.6893461724109,-5.16254485804842,
37.1811297474364));
#29438=CARTESIAN_POINT('Ctrl Pts',(-35.536065659707,-5.38020745680514,37.0278492347098));
#29439=CARTESIAN_POINT('Ctrl Pts',(-35.3159568179278,-5.38351572788345,
37.2421107447437));
#29440=CARTESIAN_POINT('Ctrl Pts',(-34.5978496132727,-3.61941807409668,
36.0896331882982));
#29441=CARTESIAN_POINT('Ctrl Pts',(-34.4443617566359,-3.83655054711529,
35.9361453316614));
#29442=CARTESIAN_POINT('Ctrl Pts',(-34.2245838299087,-3.84038894321747,
36.1504966431758));
#29443=CARTESIAN_POINT('Ctrl Pts',(0.0835265683646154,11.4728541727075,
48.5199460669665));
#29444=CARTESIAN_POINT('Ctrl Pts',(0.434571873652948,11.47819221482,48.5199461833401));
#29445=CARTESIAN_POINT('Ctrl Pts',(0.78544120302723,11.4874426767152,48.5184889915191));
#29446=CARTESIAN_POINT('Ctrl Pts',(1.48685396299278,11.5143737377395,48.5151613829998));
#29447=CARTESIAN_POINT('Ctrl Pts',(1.83739739358405,11.5320543368685,48.5132909663016));
#29448=CARTESIAN_POINT('Ctrl Pts',(2.88857791675096,11.598649286609,48.5108119661593));
#29449=CARTESIAN_POINT('Ctrl Pts',(3.59085027393415,11.6392592214975,48.506118103167));
#29450=CARTESIAN_POINT('Ctrl Pts',(4.29256572527697,11.6756605207451,48.4959174422581));
#29451=CARTESIAN_POINT('Ctrl Pts',(0.0835265683646867,11.4942063411577,
48.5199465324602));
#29452=CARTESIAN_POINT('Ctrl Pts',(0.356369924468222,11.4971000233707,48.5198869612823));
#29453=CARTESIAN_POINT('Ctrl Pts',(0.651973539440871,11.5031786713304,48.5195752074941));
#29454=CARTESIAN_POINT('Ctrl Pts',(1.2945339969987,11.5255419633083,48.5183112784645));
#29455=CARTESIAN_POINT('Ctrl Pts',(1.64148768476021,11.5418711528752,48.5173741424329));
#29456=CARTESIAN_POINT('Ctrl Pts',(2.76813631993237,11.6120206208596,48.5172046544328));
#29457=CARTESIAN_POINT('Ctrl Pts',(3.51890802363922,11.6580360440938,48.5141149281054));
#29458=CARTESIAN_POINT('Ctrl Pts',(4.29124902552725,11.6996409410751,48.5059136087032));
#29459=CARTESIAN_POINT('Ctrl Pts',(0.0835265683659855,11.5200575082527,
48.5195892904601));
#29460=CARTESIAN_POINT('Ctrl Pts',(0.356156584738792,11.5200113925674,48.5195869596123));
#29461=CARTESIAN_POINT('Ctrl Pts',(0.651610340351263,11.5245005081763,48.5196902430686));
#29462=CARTESIAN_POINT('Ctrl Pts',(1.29397444549905,11.5448479357178,48.5193460059354));
#29463=CARTESIAN_POINT('Ctrl Pts',(1.6408816402107,11.5607507931991,48.5189135245556));
#29464=CARTESIAN_POINT('Ctrl Pts',(2.76751045405255,11.6290600690807,48.5194534619891));
#29465=CARTESIAN_POINT('Ctrl Pts',(3.51790722899464,11.6785648284704,48.5175683502971));
#29466=CARTESIAN_POINT('Ctrl Pts',(4.28995382479,11.7229366511906,48.5119171961236));
#29467=CARTESIAN_POINT('Ctrl Pts',(0.0835265683637358,11.5731362269332,
48.5213546907495));
#29468=CARTESIAN_POINT('Ctrl Pts',(0.394869806429155,11.5731490589917,48.5213559145826));
#29469=CARTESIAN_POINT('Ctrl Pts',(0.717676140691825,11.5776504745527,48.5214911613194));
#29470=CARTESIAN_POINT('Ctrl Pts',(1.38907005436015,11.5959692446123,48.5214366576315));
#29471=CARTESIAN_POINT('Ctrl Pts',(1.73765605635396,11.6098088718851,48.5212544268118));
#29472=CARTESIAN_POINT('Ctrl Pts',(2.82637284200128,11.6658592241826,48.5212339924692));
#29473=CARTESIAN_POINT('Ctrl Pts',(3.55158573922134,11.7135824344715,48.5204767822115));
#29474=CARTESIAN_POINT('Ctrl Pts',(4.2874400917096,11.7642258753785,48.5189262877417));
#29475=CARTESIAN_POINT('Ctrl Pts',(0.0835265683629213,11.5876793312944,
48.5199317919394));
#29476=CARTESIAN_POINT('Ctrl Pts',(0.433796367851579,11.5876793312944,48.5199317919394));
#29477=CARTESIAN_POINT('Ctrl Pts',(0.784105140124401,11.5930695682598,48.5199317919388));
#29478=CARTESIAN_POINT('Ctrl Pts',(1.48472521472274,11.6126245374907,48.5199317919371));
#29479=CARTESIAN_POINT('Ctrl Pts',(1.83503651704826,11.6267892697562,48.5199317919361));
#29480=CARTESIAN_POINT('Ctrl Pts',(2.88586109583041,11.6794362415569,48.5199317919341));
#29481=CARTESIAN_POINT('Ctrl Pts',(3.58626504409264,11.728071256096,48.5199317919341));
#29482=CARTESIAN_POINT('Ctrl Pts',(4.28622155936646,11.7822193894509,48.5199317919394));
#29483=CARTESIAN_POINT('Ctrl Pts',(0.0835265683619702,11.6131136241746,
48.5199317919394));
#29484=CARTESIAN_POINT('Ctrl Pts',(0.433874220973474,11.6131136241746,48.5199317919394));
#29485=CARTESIAN_POINT('Ctrl Pts',(0.784221873584978,11.6169153282063,48.5199317919388));
#29486=CARTESIAN_POINT('Ctrl Pts',(1.48483467245502,11.6321221443329,48.5199317919372));
#29487=CARTESIAN_POINT('Ctrl Pts',(1.83509981871355,11.6435272564279,48.5199317919363));
#29488=CARTESIAN_POINT('Ctrl Pts',(2.88564773843024,11.689147704808,48.5199317919344));
#29489=CARTESIAN_POINT('Ctrl Pts',(3.58568299282948,11.734768153188,48.5199317919344));
#29490=CARTESIAN_POINT('Ctrl Pts',(4.28505819640496,11.7955954176946,48.5199317919394));
#29491=CARTESIAN_POINT('',(0.0835265683646154,11.4728541727075,48.5199460669665));
#29492=CARTESIAN_POINT('Ctrl Pts',(0.0835265683619702,11.6131136241746,
48.5199317919394));
#29493=CARTESIAN_POINT('Ctrl Pts',(0.0835265683629213,11.5876793312944,
48.5199317919394));
#29494=CARTESIAN_POINT('Ctrl Pts',(0.0835265683637358,11.5731362269332,
48.5213546907495));
#29495=CARTESIAN_POINT('Ctrl Pts',(0.0835265683659855,11.5200575082527,
48.5195892904601));
#29496=CARTESIAN_POINT('Ctrl Pts',(0.0835265683646867,11.4942063411577,
48.5199465324602));
#29497=CARTESIAN_POINT('Ctrl Pts',(0.0835265683646154,11.4728541727075,
48.5199460669665));
#29498=CARTESIAN_POINT('',(4.29256572406856,11.6756605346477,48.4959174087471));
#29499=CARTESIAN_POINT('Ctrl Pts',(4.28505819640497,11.7955954176945,48.5199317919394));
#29500=CARTESIAN_POINT('Ctrl Pts',(4.28563987788572,11.7889074035727,48.5199317866933));
#29501=CARTESIAN_POINT('Ctrl Pts',(4.2862286391617,11.7811426004669,48.51971728124));
#29502=CARTESIAN_POINT('Ctrl Pts',(4.28683031455212,11.7724551591809,48.5190688938798));
#29503=CARTESIAN_POINT('Ctrl Pts',(4.28737989743217,11.7645198686933,48.5184766433099));
#29504=CARTESIAN_POINT('Ctrl Pts',(4.28794027744316,11.7558145072651,48.5175204898844));
#29505=CARTESIAN_POINT('Ctrl Pts',(4.28851223325202,11.746498740511,48.516032617158));
#29506=CARTESIAN_POINT('Ctrl Pts',(4.2890564340326,11.7376350355518,48.5146169457257));
#29507=CARTESIAN_POINT('Ctrl Pts',(4.28961108824049,11.7282190174497,48.5127184771679));
#29508=CARTESIAN_POINT('Ctrl Pts',(4.29017342238365,11.7184280696926,48.510215157354));
#29509=CARTESIAN_POINT('Ctrl Pts',(4.29070902472487,11.7091025563741,48.5078308384051));
#29510=CARTESIAN_POINT('Ctrl Pts',(4.2912515217908,11.6994377386552,48.5048968999018));
#29511=CARTESIAN_POINT('Ctrl Pts',(4.29179604392015,11.6896156896679,48.5013453462893));
#29512=CARTESIAN_POINT('Ctrl Pts',(4.29205239342601,11.6849916766688,48.4996733499378));
#29513=CARTESIAN_POINT('Ctrl Pts',(4.29230916168589,11.6803331677637,48.4978651076034));
#29514=CARTESIAN_POINT('Ctrl Pts',(4.29256572165175,11.675660562453,48.4959173417252));
#29515=CARTESIAN_POINT('Ctrl Pts',(4.29256572527696,11.6756605207451,48.4959174422581));
#29516=CARTESIAN_POINT('Ctrl Pts',(3.59085027393415,11.6392592214975,48.506118103167));
#29517=CARTESIAN_POINT('Ctrl Pts',(2.88857791675096,11.598649286609,48.5108119661593));
#29518=CARTESIAN_POINT('Ctrl Pts',(1.48700388586174,11.5098560202884,48.5141172996824));
#29519=CARTESIAN_POINT('Ctrl Pts',(0.78561717894128,11.4835302569325,48.5199462997137));
#29520=CARTESIAN_POINT('Ctrl Pts',(0.0835265683646154,11.4728541727075,
48.5199460669665));
#29521=CARTESIAN_POINT('Ctrl Pts',(0.0835265683646154,11.4728541727075,
48.5199460669665));
#29522=CARTESIAN_POINT('Ctrl Pts',(0.434571873652913,11.4675161305949,48.5199459505932));
#29523=CARTESIAN_POINT('Ctrl Pts',(0.785669116598665,11.4659265087691,48.5184885224499));
#29524=CARTESIAN_POINT('Ctrl Pts',(1.48799468015646,11.464396632877,48.5087577020976));
#29525=CARTESIAN_POINT('Ctrl Pts',(1.83922300076851,11.4644563788108,48.5004843098885));
#29526=CARTESIAN_POINT('Ctrl Pts',(2.89314538263116,11.4583384590299,48.4595881763738));
#29527=CARTESIAN_POINT('Ctrl Pts',(3.59439815510967,11.4609474762041,48.4163876002293));
#29528=CARTESIAN_POINT('Ctrl Pts',(4.29550794737987,11.4732422824941,48.3603316468569));
#29529=CARTESIAN_POINT('Ctrl Pts',(0.434571873652948,11.47819221482,48.5199461833401));
#29530=CARTESIAN_POINT('Ctrl Pts',(0.707588293934062,11.474986089803,48.5190043349166));
#29531=CARTESIAN_POINT('Ctrl Pts',(0.998676156497516,11.4745419834778,48.5169166777059));
#29532=CARTESIAN_POINT('Ctrl Pts',(1.6137782469759,11.4744825705815,48.5070409830049));
#29533=CARTESIAN_POINT('Ctrl Pts',(1.93779750982841,11.4748353413217,48.4992338111971));
#29534=CARTESIAN_POINT('Ctrl Pts',(2.9544266533864,11.4700074930207,48.4591554550249));
#29535=CARTESIAN_POINT('Ctrl Pts',(3.63137389791096,11.4731609516944,48.4176356670413));
#29536=CARTESIAN_POINT('Ctrl Pts',(4.29556063459987,11.4851966459098,48.3652975204339));
#29537=CARTESIAN_POINT('Ctrl Pts',(0.78544120302723,11.4874426767152,48.5184889915191));
#29538=CARTESIAN_POINT('Ctrl Pts',(0.998330962591659,11.484480312248,48.5172889554747));
#29539=CARTESIAN_POINT('Ctrl Pts',(1.24336152271846,11.4840908039498,48.514900881629));
#29540=CARTESIAN_POINT('Ctrl Pts',(1.78770682159394,11.4843329006938,48.5050013605299));
#29541=CARTESIAN_POINT('Ctrl Pts',(2.08702911274898,11.4849166217029,48.4974612118004));
#29542=CARTESIAN_POINT('Ctrl Pts',(3.05143599908222,11.4818828006799,48.4585450693865));
#29543=CARTESIAN_POINT('Ctrl Pts',(3.69355131246621,11.4863352799679,48.4189800886588));
#29544=CARTESIAN_POINT('Ctrl Pts',(4.29569371583977,11.497472006951,48.3719827330256));
#29545=CARTESIAN_POINT('Ctrl Pts',(1.48685396299278,11.5143737377395,48.5151613829998));
#29546=CARTESIAN_POINT('Ctrl Pts',(1.61221600332869,11.5105174196343,48.5134046445916));
#29547=CARTESIAN_POINT('Ctrl Pts',(1.78640027442033,11.5090816899187,48.5103147764347));
#29548=CARTESIAN_POINT('Ctrl Pts',(2.21034412033182,11.5079260458442,48.4999506929245));
#29549=CARTESIAN_POINT('Ctrl Pts',(2.4601131356596,11.5081462764441,48.4926406007259));
#29550=CARTESIAN_POINT('Ctrl Pts',(3.28969174892232,11.5065304546904,48.456544560029));
#29551=CARTESIAN_POINT('Ctrl Pts',(3.8387134471824,11.5121367174565,48.4216081073346));
#29552=CARTESIAN_POINT('Ctrl Pts',(4.29625434599571,11.5208685373805,48.3864516772668));
#29553=CARTESIAN_POINT('Ctrl Pts',(1.83739739358405,11.5320543368685,48.5132909663016));
#29554=CARTESIAN_POINT('Ctrl Pts',(1.93535675584129,11.5270830007426,48.5112385621713));
#29555=CARTESIAN_POINT('Ctrl Pts',(2.08475123055101,11.5245577996658,48.5077487408488));
#29556=CARTESIAN_POINT('Ctrl Pts',(2.45904980776384,11.5217114161952,48.4969449897084));
#29557=CARTESIAN_POINT('Ctrl Pts',(2.68396272140769,11.5213343690961,48.489597574835));
#29558=CARTESIAN_POINT('Ctrl Pts',(3.43093653349979,11.5193254972085,48.455157285331));
#29559=CARTESIAN_POINT('Ctrl Pts',(3.92169816734333,11.5247638266718,48.4228917043929));
#29560=CARTESIAN_POINT('Ctrl Pts',(4.29668189491177,11.5319897067687,48.3942354089164));
#29561=CARTESIAN_POINT('Ctrl Pts',(2.88857791675096,11.598649286609,48.5108119661593));
#29562=CARTESIAN_POINT('Ctrl Pts',(2.9488036240303,11.5919036248663,48.507599134787));
#29563=CARTESIAN_POINT('Ctrl Pts',(3.0457795460293,11.5859418512212,48.5025662258368));
#29564=CARTESIAN_POINT('Ctrl Pts',(3.28508025551021,11.5755468354636,48.4895414183257));
#29565=CARTESIAN_POINT('Ctrl Pts',(3.42741007792968,11.5710816706623,48.4815303854473));
#29566=CARTESIAN_POINT('Ctrl Pts',(3.8802020832709,11.5598336028535,48.4510874244428));
#29567=CARTESIAN_POINT('Ctrl Pts',(4.15746922938128,11.5581209387927,48.4262709574734));
#29568=CARTESIAN_POINT('Ctrl Pts',(4.29860676262873,11.5609276470972,48.4157241439942));
#29569=CARTESIAN_POINT('Ctrl Pts',(3.59085027393415,11.6392592214975,48.506118103167));
#29570=CARTESIAN_POINT('Ctrl Pts',(3.62682139908161,11.6298708101994,48.5021196906978));
#29571=CARTESIAN_POINT('Ctrl Pts',(3.68879009436557,11.6209827896646,48.4962278199978));
#29572=CARTESIAN_POINT('Ctrl Pts',(3.83438595526553,11.6050189470302,48.4820050859842));
#29573=CARTESIAN_POINT('Ctrl Pts',(3.91801312088154,11.5979431249305,48.4736742226707));
#29574=CARTESIAN_POINT('Ctrl Pts',(4.15587731831616,11.5806510816468,48.447045029582));
#29575=CARTESIAN_POINT('Ctrl Pts',(4.29707247281346,11.5743267261738,48.4278950754016));
#29576=CARTESIAN_POINT('Ctrl Pts',(4.30074630239845,11.5743188502015,48.4275666875517));
#29577=CARTESIAN_POINT('Ctrl Pts',(4.29256572527697,11.6756605207451,48.4959174422581));
#29578=CARTESIAN_POINT('Ctrl Pts',(4.29322407515183,11.6636703105801,48.4909193590355));
#29579=CARTESIAN_POINT('Ctrl Pts',(4.29389281459049,11.6514649415886,48.4847891628829));
#29580=CARTESIAN_POINT('Ctrl Pts',(4.29532858886799,11.6282480883359,48.4713889284475));
#29581=CARTESIAN_POINT('Ctrl Pts',(4.29609562370683,11.6172366040747,48.4641188901648));
#29582=CARTESIAN_POINT('Ctrl Pts',(4.29866044573254,11.588429281961,48.4422855877167));
#29583=CARTESIAN_POINT('Ctrl Pts',(4.30071410004355,11.5746245276893,48.4278763391902));
#29584=CARTESIAN_POINT('Ctrl Pts',(4.30427685533877,11.5746245485738,48.4275653153946));
#29585=CARTESIAN_POINT('Ctrl Pts',(4.29256572527696,11.6756605207451,48.4959174422581));
#29586=CARTESIAN_POINT('Ctrl Pts',(4.2938824250267,11.6516801004151,48.485921275813));
#29587=CARTESIAN_POINT('Ctrl Pts',(4.29524068303159,11.6268390447792,48.4713966576475));
#29588=CARTESIAN_POINT('Ctrl Pts',(4.29866044573254,11.588429281961,48.4422855877167));
#29589=CARTESIAN_POINT('Ctrl Pts',(4.30071410004355,11.5746245276893,48.4278763391902));
#29590=CARTESIAN_POINT('Ctrl Pts',(4.30427685533877,11.5746245485738,48.4275653153946));
#29591=CARTESIAN_POINT('',(4.29550794737987,11.4732422824942,48.360331646857));
#29592=CARTESIAN_POINT('Ctrl Pts',(4.30427685533877,11.5746245485738,48.4275653153946));
#29593=CARTESIAN_POINT('Ctrl Pts',(4.29721574945814,11.5740131518292,48.4275680597088));
#29594=CARTESIAN_POINT('Ctrl Pts',(4.29571869625989,11.5210597361567,48.3801951411647));
#29595=CARTESIAN_POINT('Ctrl Pts',(4.29550794737987,11.4732422824942,48.360331646857));
#29596=CARTESIAN_POINT('Ctrl Pts',(4.29550794737987,11.4732422824942,48.360331646857));
#29597=CARTESIAN_POINT('Ctrl Pts',(3.59439815510967,11.4609474762041,48.4163876002292));
#29598=CARTESIAN_POINT('Ctrl Pts',(2.89314538263116,11.4583384590299,48.4595881763737));
#29599=CARTESIAN_POINT('Ctrl Pts',(1.48791554014763,11.4664956854044,48.5141163543934));
#29600=CARTESIAN_POINT('Ctrl Pts',(0.785617178941208,11.4621780884822,48.5199458342199));
#29601=CARTESIAN_POINT('Ctrl Pts',(0.0835265683646154,11.4728541727075,
48.5199460669665));
#29602=CARTESIAN_POINT('Ctrl Pts',(0.0835265683646154,11.4728541727075,
48.5199460669665));
#29603=CARTESIAN_POINT('Ctrl Pts',(0.0835265683645438,11.4515020042572,
48.5199456014727));
#29604=CARTESIAN_POINT('Ctrl Pts',(0.0835265683631205,11.4284235901226,
48.5195872927698));
#29605=CARTESIAN_POINT('Ctrl Pts',(0.0835265683628376,11.3941472536996,
48.5154826406219));
#29606=CARTESIAN_POINT('Ctrl Pts',(0.0835265683627773,11.3720285904897,
48.5199317919394));
#29607=CARTESIAN_POINT('Ctrl Pts',(0.0835265683619676,11.353653679453,48.5199317919394));
#29608=CARTESIAN_POINT('Ctrl Pts',(0.434571873652913,11.4675161305949,48.5199459505932));
#29609=CARTESIAN_POINT('Ctrl Pts',(0.356716052822661,11.4488974993902,48.51988591043));
#29610=CARTESIAN_POINT('Ctrl Pts',(0.339530012993789,11.4285976962987,48.5196215918845));
#29611=CARTESIAN_POINT('Ctrl Pts',(0.361332410433279,11.3940705712691,48.5154600081738));
#29612=CARTESIAN_POINT('Ctrl Pts',(0.400320847700618,11.3720285904897,48.5199317919394));
#29613=CARTESIAN_POINT('Ctrl Pts',(0.434813981059838,11.353653679453,48.5199317919394));
#29614=CARTESIAN_POINT('Ctrl Pts',(0.785669116598665,11.4659265087691,48.5184885224499));
#29615=CARTESIAN_POINT('Ctrl Pts',(0.652301278511543,11.447718516688,48.5186918880708));
#29616=CARTESIAN_POINT('Ctrl Pts',(0.626534465182239,11.428587933622,48.5182575867036));
#29617=CARTESIAN_POINT('Ctrl Pts',(0.667559641505308,11.3934281614349,48.5133469042742));
#29618=CARTESIAN_POINT('Ctrl Pts',(0.734351631156823,11.3718199008203,48.5168141308044));
#29619=CARTESIAN_POINT('Ctrl Pts',(0.786101399028862,11.353653679453,48.5161104362146));
#29620=CARTESIAN_POINT('Ctrl Pts',(1.48799468015646,11.464396632877,48.5087577020976));
#29621=CARTESIAN_POINT('Ctrl Pts',(1.29495517067291,11.4452664260876,48.5103258778886));
#29622=CARTESIAN_POINT('Ctrl Pts',(1.26276365300082,11.4271829834973,48.5091673912096));
#29623=CARTESIAN_POINT('Ctrl Pts',(1.32724155706699,11.39130385313,48.5020950494664));
#29624=CARTESIAN_POINT('Ctrl Pts',(1.42391097880467,11.3711415135622,48.5026532295396));
#29625=CARTESIAN_POINT('Ctrl Pts',(1.48859334813903,11.353653679453,48.50082319184));
#29626=CARTESIAN_POINT('Ctrl Pts',(1.83922300076851,11.4644563788108,48.5004843098885));
#29627=CARTESIAN_POINT('Ctrl Pts',(1.64203235159374,11.443938017789,48.5030276183437));
#29628=CARTESIAN_POINT('Ctrl Pts',(1.61199486709086,11.425732495649,48.5013148775259));
#29629=CARTESIAN_POINT('Ctrl Pts',(1.68069642943966,11.389794304459,48.4928930593065));
#29630=CARTESIAN_POINT('Ctrl Pts',(1.7794354762909,11.3706718159735,48.491609885926));
#29631=CARTESIAN_POINT('Ctrl Pts',(1.83979788982311,11.353653679453,48.489357302818));
#29632=CARTESIAN_POINT('Ctrl Pts',(2.54183792201028,11.4603777656235,48.4732202208787));
#29633=CARTESIAN_POINT('Ctrl Pts',(2.39436890042523,11.4381382649983,48.4746917382113));
#29634=CARTESIAN_POINT('Ctrl Pts',(2.37286182154143,11.4203247666438,48.4721918658361));
#29635=CARTESIAN_POINT('Ctrl Pts',(2.42513999639859,11.3861758639155,48.4637155121672));
#29636=CARTESIAN_POINT('Ctrl Pts',(2.49892525013932,11.3696277842964,48.4610292841198));
#29637=CARTESIAN_POINT('Ctrl Pts',(2.54204089380268,11.353653679453,48.4587755322629));
#29638=CARTESIAN_POINT('Ctrl Pts',(2.89280484544034,11.4600103666203,48.4556040545901));
#29639=CARTESIAN_POINT('Ctrl Pts',(2.76993041129963,11.4370088609558,48.4559496852932));
#29640=CARTESIAN_POINT('Ctrl Pts',(2.75490259059407,11.4187667259072,48.4528734061814));
#29641=CARTESIAN_POINT('Ctrl Pts',(2.80138061725977,11.3847952022384,48.4445443128281));
#29642=CARTESIAN_POINT('Ctrl Pts',(2.86288646463088,11.369053450208,48.4414922321744));
#29643=CARTESIAN_POINT('Ctrl Pts',(2.89307936664307,11.353653679453,48.439659649984));
#29644=CARTESIAN_POINT('Ctrl Pts',(3.59436241005759,11.4633689234831,48.4131737559223));
#29645=CARTESIAN_POINT('Ctrl Pts',(3.52670827169875,11.4394032486783,48.4096766577646));
#29646=CARTESIAN_POINT('Ctrl Pts',(3.5225115642211,11.4193327724023,48.4051808771548));
#29647=CARTESIAN_POINT('Ctrl Pts',(3.55227792535516,11.3835624194323,48.3973032871378));
#29648=CARTESIAN_POINT('Ctrl Pts',(3.58624099396685,11.3679565169509,48.3944770846954));
#29649=CARTESIAN_POINT('Ctrl Pts',(3.59490640778659,11.353653679453,48.3937688119853));
#29650=CARTESIAN_POINT('Ctrl Pts',(3.94495305124477,11.4670948793491,48.3883596235431));
#29651=CARTESIAN_POINT('Ctrl Pts',(3.90792462122347,11.4429270404433,48.3821456831541));
#29652=CARTESIAN_POINT('Ctrl Pts',(3.90807774441525,11.4214568596339,48.3768070662869));
#29653=CARTESIAN_POINT('Ctrl Pts',(3.9269305664659,11.3837102983034,48.3692339775144));
#29654=CARTESIAN_POINT('Ctrl Pts',(3.94563026532478,11.3674339177823,48.3669995056091));
#29655=CARTESIAN_POINT('Ctrl Pts',(3.94569498663766,11.353653679453,48.3669938551438));
#29656=CARTESIAN_POINT('Ctrl Pts',(4.29550794737987,11.4732422824941,48.3603316468569));
#29657=CARTESIAN_POINT('Ctrl Pts',(4.29540257293986,11.4493335556629,48.3503998997031));
#29658=CARTESIAN_POINT('Ctrl Pts',(4.29560464263433,11.4261172510677,48.3444127441005));
#29659=CARTESIAN_POINT('Ctrl Pts',(4.29606146924328,11.384958159128,48.3374043064722));
#29660=CARTESIAN_POINT('Ctrl Pts',(4.29631622615776,11.3670153717833,48.3363830244465));
#29661=CARTESIAN_POINT('Ctrl Pts',(4.29631622615776,11.353653679453,48.3363830244465));
#29662=CARTESIAN_POINT('Ctrl Pts',(4.29550794737987,11.4732422824942,48.360331646857));
#29663=CARTESIAN_POINT('Ctrl Pts',(4.29546091471024,11.4625708971931,48.3558987257173));
#29664=CARTESIAN_POINT('Ctrl Pts',(4.29547085992706,11.4520014357867,48.3522029429309));
#29665=CARTESIAN_POINT('Ctrl Pts',(4.29551799962758,11.4417444398151,48.3491738175902));
#29666=CARTESIAN_POINT('Ctrl Pts',(4.29556841690108,11.4307742858786,48.3459340804028));
#29667=CARTESIAN_POINT('Ctrl Pts',(4.29566133560236,11.420162601422,48.3434563976416));
#29668=CARTESIAN_POINT('Ctrl Pts',(4.29576766490653,11.4101434346418,48.341598642047));
#29669=CARTESIAN_POINT('Ctrl Pts',(4.29588042424243,11.3995183806997,48.3396285427527));
#29670=CARTESIAN_POINT('Ctrl Pts',(4.29600813145325,11.3895604073049,48.338354073489));
#29671=CARTESIAN_POINT('Ctrl Pts',(4.29611218230524,11.3805081454716,48.3375612325113));
#29672=CARTESIAN_POINT('Ctrl Pts',(4.29622934837385,11.3703148802493,48.3366684569251));
#29673=CARTESIAN_POINT('Ctrl Pts',(4.29631622615776,11.3612705067707,48.3363830244465));
#29674=CARTESIAN_POINT('Ctrl Pts',(4.29631622615776,11.353653679453,48.3363830244465));
#29675=CARTESIAN_POINT('Ctrl Pts',(0.0835265683619891,11.353653679453,48.5199317919394));
#29676=CARTESIAN_POINT('Ctrl Pts',(0.0835265683627773,11.3720285904897,
48.5199317919394));
#29677=CARTESIAN_POINT('Ctrl Pts',(0.0835265683628376,11.3941472536996,
48.5154826406219));
#29678=CARTESIAN_POINT('Ctrl Pts',(0.0835265683631205,11.4284235901226,
48.5195872927698));
#29679=CARTESIAN_POINT('Ctrl Pts',(0.0835265683645438,11.4515020042572,
48.5199456014727));
#29680=CARTESIAN_POINT('Ctrl Pts',(0.0835265683646154,11.4728541727075,
48.5199460669665));
#29681=CARTESIAN_POINT('Ctrl Pts',(0.0835265683646154,11.4728541727075,
48.5199460669665));
#29682=CARTESIAN_POINT('Ctrl Pts',(-0.267518736923717,11.4675161305949,
48.5199459505928));
#29683=CARTESIAN_POINT('Ctrl Pts',(-0.61861597986895,11.4659265087692,48.5184885224493));
#29684=CARTESIAN_POINT('Ctrl Pts',(-1.32094154342462,11.4643966328772,48.5087577020968));
#29685=CARTESIAN_POINT('Ctrl Pts',(-1.67216986403505,11.4644563788108,48.5004843098878));
#29686=CARTESIAN_POINT('Ctrl Pts',(-2.37478478527252,11.4603777656235,48.4732202208791));
#29687=CARTESIAN_POINT('Ctrl Pts',(-2.72575170870462,11.4600103666202,48.4556040545906));
#29688=CARTESIAN_POINT('Ctrl Pts',(-3.4273092733279,11.463368923483,48.4131737559227));
#29689=CARTESIAN_POINT('Ctrl Pts',(-3.77789991451908,11.4670948793491,48.3883596235432));
#29690=CARTESIAN_POINT('Ctrl Pts',(-4.12845481065596,11.4732422824942,48.3603316468569));
#29691=CARTESIAN_POINT('Ctrl Pts',(0.0835265683645438,11.4515020042572,
48.5199456014727));
#29692=CARTESIAN_POINT('Ctrl Pts',(-0.189662916093927,11.4488974993903,
48.5198859104297));
#29693=CARTESIAN_POINT('Ctrl Pts',(-0.485248141782668,11.4477185166882,
48.5186918880704));
#29694=CARTESIAN_POINT('Ctrl Pts',(-1.12790203394243,11.4452664260878,48.5103258778881));
#29695=CARTESIAN_POINT('Ctrl Pts',(-1.47497921486181,11.4439380177892,48.5030276183433));
#29696=CARTESIAN_POINT('Ctrl Pts',(-2.22731576368872,11.4381382649983,48.4746917382118));
#29697=CARTESIAN_POINT('Ctrl Pts',(-2.60287727456489,11.4370088609558,48.4559496852938));
#29698=CARTESIAN_POINT('Ctrl Pts',(-3.35965513496952,11.4394032486783,48.409676657765));
#29699=CARTESIAN_POINT('Ctrl Pts',(-3.74087148449797,11.4429270404433,48.3821456831542));
#29700=CARTESIAN_POINT('Ctrl Pts',(-4.12834943621596,11.4493335556629,48.3503998997031));
#29701=CARTESIAN_POINT('Ctrl Pts',(0.0835265683631205,11.4284235901226,
48.5195872927698));
#29702=CARTESIAN_POINT('Ctrl Pts',(-0.172476876267548,11.4285976962988,
48.5196215918844));
#29703=CARTESIAN_POINT('Ctrl Pts',(-0.459481328455685,11.4285879336221,
48.5182575867033));
#29704=CARTESIAN_POINT('Ctrl Pts',(-1.0957105162727,11.4271829834975,48.5091673912093));
#29705=CARTESIAN_POINT('Ctrl Pts',(-1.44494173036149,11.4257324956491,48.5013148775256));
#29706=CARTESIAN_POINT('Ctrl Pts',(-2.20580868480827,11.4203247666438,48.4721918658365));
#29707=CARTESIAN_POINT('Ctrl Pts',(-2.58784945386211,11.4187667259072,48.4528734061819));
#29708=CARTESIAN_POINT('Ctrl Pts',(-3.35545842749311,11.4193327724023,48.4051808771551));
#29709=CARTESIAN_POINT('Ctrl Pts',(-3.74102460769006,11.4214568596339,48.376807066287));
#29710=CARTESIAN_POINT('Ctrl Pts',(-4.12855150591043,11.4261172510678,48.3444127441005));
#29711=CARTESIAN_POINT('Ctrl Pts',(0.0835265683628376,11.3941472536996,
48.5154826406219));
#29712=CARTESIAN_POINT('Ctrl Pts',(-0.194279273707604,11.3940705712692,
48.5154600081738));
#29713=CARTESIAN_POINT('Ctrl Pts',(-0.500506504779572,11.393428161435,48.5133469042742));
#29714=CARTESIAN_POINT('Ctrl Pts',(-1.16018842034084,11.39130385313,48.5020950494664));
#29715=CARTESIAN_POINT('Ctrl Pts',(-1.51364329271317,11.3897943044591,48.4928930593065));
#29716=CARTESIAN_POINT('Ctrl Pts',(-2.25808685967095,11.3861758639155,48.4637155121674));
#29717=CARTESIAN_POINT('Ctrl Pts',(-2.6343274805326,11.3847952022384,48.4445443128283));
#29718=CARTESIAN_POINT('Ctrl Pts',(-3.38522478862952,11.3835624194324,48.3973032871379));
#29719=CARTESIAN_POINT('Ctrl Pts',(-3.75987742974135,11.3837102983034,48.3692339775145));
#29720=CARTESIAN_POINT('Ctrl Pts',(-4.12900833251936,11.384958159128,48.3374043064722));
#29721=CARTESIAN_POINT('Ctrl Pts',(0.0835265683627773,11.3720285904897,
48.5199317919394));
#29722=CARTESIAN_POINT('Ctrl Pts',(-0.233267710975063,11.3720285904897,
48.5199317919394));
#29723=CARTESIAN_POINT('Ctrl Pts',(-0.567298494431303,11.3718199008203,
48.5168141308044));
#29724=CARTESIAN_POINT('Ctrl Pts',(-1.25685784207929,11.3711415135622,48.5026532295397));
#29725=CARTESIAN_POINT('Ctrl Pts',(-1.61238233956562,11.3706718159735,48.491609885926));
#29726=CARTESIAN_POINT('Ctrl Pts',(-2.33187211341431,11.3696277842964,48.4610292841198));
#29727=CARTESIAN_POINT('Ctrl Pts',(-2.69583332790602,11.369053450208,48.4414922321744));
#29728=CARTESIAN_POINT('Ctrl Pts',(-3.41918785724238,11.3679565169509,48.3944770846954));
#29729=CARTESIAN_POINT('Ctrl Pts',(-3.77857712860057,11.3674339177823,48.3669995056091));
#29730=CARTESIAN_POINT('Ctrl Pts',(-4.12926308943382,11.3670153717833,48.3363830244465));
#29731=CARTESIAN_POINT('Ctrl Pts',(0.0835265683619676,11.353653679453,48.5199317919394));
#29732=CARTESIAN_POINT('Ctrl Pts',(-0.267760844335902,11.353653679453,48.5199317919394));
#29733=CARTESIAN_POINT('Ctrl Pts',(-0.619048262304927,11.3536536794531,
48.5161104362146));
#29734=CARTESIAN_POINT('Ctrl Pts',(-1.32154021141509,11.3536536794531,48.50082319184));
#29735=CARTESIAN_POINT('Ctrl Pts',(-1.67274475309917,11.3536536794531,48.489357302818));
#29736=CARTESIAN_POINT('Ctrl Pts',(-2.37498775707875,11.3536536794531,48.4587755322629));
#29737=CARTESIAN_POINT('Ctrl Pts',(-2.72602622991912,11.3536536794531,48.439659649984));
#29738=CARTESIAN_POINT('Ctrl Pts',(-3.42785327106262,11.3536536794531,48.3937688119853));
#29739=CARTESIAN_POINT('Ctrl Pts',(-3.77864184991372,11.3536536794531,48.3669938551438));
#29740=CARTESIAN_POINT('Ctrl Pts',(-4.12926308943382,11.3536536794531,48.3363830244465));
#29741=CARTESIAN_POINT('',(-4.12845481065596,11.4732422824942,48.360331646857));
#29742=CARTESIAN_POINT('Ctrl Pts',(-4.12926308943382,11.3536536794531,48.3363830244465));
#29743=CARTESIAN_POINT('Ctrl Pts',(-4.12926308943382,11.3608560447969,48.3363830244465));
#29744=CARTESIAN_POINT('Ctrl Pts',(-4.12918541418972,11.3693343502548,48.3366383003061));
#29745=CARTESIAN_POINT('Ctrl Pts',(-4.12907789424658,11.3788543868427,48.3374208419226));
#29746=CARTESIAN_POINT('Ctrl Pts',(-4.1289785687574,11.3876488696476,48.338143743429));
#29747=CARTESIAN_POINT('Ctrl Pts',(-4.12885398245303,11.3973323098416,48.339318986334));
#29748=CARTESIAN_POINT('Ctrl Pts',(-4.12874104374852,11.4076804802594,48.3411521533193));
#29749=CARTESIAN_POINT('Ctrl Pts',(-4.12863183371979,11.4176870054229,48.3429247982243));
#29750=CARTESIAN_POINT('Ctrl Pts',(-4.12853365126042,11.428314631214,48.3453142106815));
#29751=CARTESIAN_POINT('Ctrl Pts',(-4.12847668203915,11.4393255986458,48.3484700316399));
#29752=CARTESIAN_POINT('Ctrl Pts',(-4.12842391816255,11.4495237602834,48.3513928967225));
#29753=CARTESIAN_POINT('Ctrl Pts',(-4.1284065446436,11.460049829507,48.354973634109));
#29754=CARTESIAN_POINT('Ctrl Pts',(-4.12844464232628,11.4706948755439,48.3592865236346));
#29755=CARTESIAN_POINT('Ctrl Pts',(-4.12844767875758,11.4715432985642,48.3596302661365));
#29756=CARTESIAN_POINT('Ctrl Pts',(-4.12845106522601,11.4723924705143,48.3599786327558));
#29757=CARTESIAN_POINT('Ctrl Pts',(-4.12845481065596,11.4732422824942,48.3603316468569));
#29758=CARTESIAN_POINT('Ctrl Pts',(-4.12845481065596,11.4732422824942,48.360331646857));
#29759=CARTESIAN_POINT('Ctrl Pts',(-3.4273450183822,11.4609474762041,48.4163876002295));
#29760=CARTESIAN_POINT('Ctrl Pts',(-2.72609224589126,11.4583384590298,48.4595881763747));
#29761=CARTESIAN_POINT('Ctrl Pts',(-1.32086240341632,11.4664956854045,48.5141163543922));
#29762=CARTESIAN_POINT('Ctrl Pts',(-0.618564042212051,11.4621780884824,
48.5199458342193));
#29763=CARTESIAN_POINT('Ctrl Pts',(0.0835265683646154,11.4728541727075,
48.5199460669665));
#29764=CARTESIAN_POINT('Ctrl Pts',(0.0835265683646154,11.4728541727075,
48.5199460669665));
#29765=CARTESIAN_POINT('Ctrl Pts',(-0.267518736923682,11.47819221482,48.5199461833397));
#29766=CARTESIAN_POINT('Ctrl Pts',(-0.618388066296979,11.4874426767151,
48.5184889915183));
#29767=CARTESIAN_POINT('Ctrl Pts',(-1.31980082625865,11.5143737377389,48.5151613829986));
#29768=CARTESIAN_POINT('Ctrl Pts',(-1.67034425684702,11.5320543368675,48.5132909663004));
#29769=CARTESIAN_POINT('Ctrl Pts',(-2.72152478000237,11.5986492866067,48.5108119661587));
#29770=CARTESIAN_POINT('Ctrl Pts',(-3.42379713716555,11.6392592214936,48.5061181031666));
#29771=CARTESIAN_POINT('Ctrl Pts',(-4.12551258849121,11.6756605207398,48.4959174422581));
#29772=CARTESIAN_POINT('Ctrl Pts',(-0.267518736923717,11.4675161305949,
48.5199459505928));
#29773=CARTESIAN_POINT('Ctrl Pts',(-0.540535157204295,11.4749860898031,
48.5190043349159));
#29774=CARTESIAN_POINT('Ctrl Pts',(-0.831277825861035,11.4844803122479,
48.5172889554738));
#29775=CARTESIAN_POINT('Ctrl Pts',(-1.44516286659434,11.5105174196336,48.5134046445902));
#29776=CARTESIAN_POINT('Ctrl Pts',(-1.76830361910408,11.5270830007414,48.5112385621698));
#29777=CARTESIAN_POINT('Ctrl Pts',(-2.78175048727934,11.5919036248635,48.5075991347862));
#29778=CARTESIAN_POINT('Ctrl Pts',(-3.45976826230679,11.6298708101947,48.5021196906972));
#29779=CARTESIAN_POINT('Ctrl Pts',(-4.12617093834983,11.6636703105734,48.4909193590356));
#29780=CARTESIAN_POINT('Ctrl Pts',(-0.61861597986895,11.4659265087692,48.5184885224493));
#29781=CARTESIAN_POINT('Ctrl Pts',(-0.831623019767032,11.4745419834779,
48.5169166777051));
#29782=CARTESIAN_POINT('Ctrl Pts',(-1.07630838598628,11.4840908039496,48.5149008816279));
#29783=CARTESIAN_POINT('Ctrl Pts',(-1.6193471376818,11.5090816899177,48.5103147764332));
#29784=CARTESIAN_POINT('Ctrl Pts',(-1.91769809380781,11.5245577996642,48.5077487408472));
#29785=CARTESIAN_POINT('Ctrl Pts',(-2.87872640926596,11.5859418512174,48.5025662258359));
#29786=CARTESIAN_POINT('Ctrl Pts',(-3.52173695757365,11.6209827896584,48.496227819997));
#29787=CARTESIAN_POINT('Ctrl Pts',(-4.12683967776745,11.6514649415801,48.4847891628829));
#29788=CARTESIAN_POINT('Ctrl Pts',(-1.32094154342462,11.4643966328772,48.5087577020968));
#29789=CARTESIAN_POINT('Ctrl Pts',(-1.4467251102432,11.4744825705815,48.507040983004));
#29790=CARTESIAN_POINT('Ctrl Pts',(-1.6206536848576,11.4843329006934,48.5050013605288));
#29791=CARTESIAN_POINT('Ctrl Pts',(-2.04329098358324,11.5079260458424,48.499950692923));
#29792=CARTESIAN_POINT('Ctrl Pts',(-2.29199667100668,11.5217114161924,48.4969449897068));
#29793=CARTESIAN_POINT('Ctrl Pts',(-3.1180271187208,11.5755468354576,48.4895414183245));
#29794=CARTESIAN_POINT('Ctrl Pts',(-3.66733281844084,11.6050189470212,48.4820050859833));
#29795=CARTESIAN_POINT('Ctrl Pts',(-4.12827545201166,11.6282480883245,48.4713889284476));
#29796=CARTESIAN_POINT('Ctrl Pts',(-1.67216986403505,11.4644563788108,48.5004843098878));
#29797=CARTESIAN_POINT('Ctrl Pts',(-1.7707443730942,11.4748353413217,48.4992338111963));
#29798=CARTESIAN_POINT('Ctrl Pts',(-1.91997597601002,11.4849166217024,48.4974612117994));
#29799=CARTESIAN_POINT('Ctrl Pts',(-2.29305999890518,11.5081462764419,48.4926406007247));
#29800=CARTESIAN_POINT('Ctrl Pts',(-2.51690958464257,11.5213343690928,48.4895975748336));
#29801=CARTESIAN_POINT('Ctrl Pts',(-3.2603569411266,11.5710816706553,48.4815303854461));
#29802=CARTESIAN_POINT('Ctrl Pts',(-3.75095998404117,11.5979431249203,48.4736742226698));
#29803=CARTESIAN_POINT('Ctrl Pts',(-4.12904248683824,11.6172366040622,48.4641188901649));
#29804=CARTESIAN_POINT('Ctrl Pts',(-2.72609224589126,11.4583384590298,48.4595881763747));
#29805=CARTESIAN_POINT('Ctrl Pts',(-2.78737351664595,11.4700074930205,48.4591554550258));
#29806=CARTESIAN_POINT('Ctrl Pts',(-2.88438286233575,11.4818828006791,48.4585450693872));
#29807=CARTESIAN_POINT('Ctrl Pts',(-3.12263861215733,11.5065304546877,48.4565445600294));
#29808=CARTESIAN_POINT('Ctrl Pts',(-3.26388339672229,11.5193254972046,48.4551572853311));
#29809=CARTESIAN_POINT('Ctrl Pts',(-3.71314894645291,11.5598336028455,48.4510874244425));
#29810=CARTESIAN_POINT('Ctrl Pts',(-3.98882418146572,11.5806510816358,48.4470450295816));
#29811=CARTESIAN_POINT('Ctrl Pts',(-4.13160730886785,11.5884292819489,48.4422855877167));
#29812=CARTESIAN_POINT('Ctrl Pts',(-3.4273450183822,11.4609474762041,48.4163876002295));
#29813=CARTESIAN_POINT('Ctrl Pts',(-3.46432076118331,11.4731609516943,48.4176356670416));
#29814=CARTESIAN_POINT('Ctrl Pts',(-3.52649817573868,11.4863352799677,48.4189800886591));
#29815=CARTESIAN_POINT('Ctrl Pts',(-3.67166031045544,11.5121367174564,48.4216081073348));
#29816=CARTESIAN_POINT('Ctrl Pts',(-3.75464503061683,11.5247638266717,48.422891704393));
#29817=CARTESIAN_POINT('Ctrl Pts',(-3.99041609265622,11.5581209387927,48.4262709574735));
#29818=CARTESIAN_POINT('Ctrl Pts',(-4.13001933608946,11.5743267261738,48.4278950754016));
#29819=CARTESIAN_POINT('Ctrl Pts',(-4.13366096331961,11.5746245276893,48.4278763391902));
#29820=CARTESIAN_POINT('Ctrl Pts',(-4.12845481065596,11.4732422824942,48.3603316468569));
#29821=CARTESIAN_POINT('Ctrl Pts',(-4.12850749787596,11.4851966459098,48.3652975204339));
#29822=CARTESIAN_POINT('Ctrl Pts',(-4.12864057911585,11.4974720069511,48.3719827330256));
#29823=CARTESIAN_POINT('Ctrl Pts',(-4.12920120927179,11.5208685373805,48.3864516772668));
#29824=CARTESIAN_POINT('Ctrl Pts',(-4.12962875818784,11.5319897067687,48.3942354089164));
#29825=CARTESIAN_POINT('Ctrl Pts',(-4.13155362590479,11.5609276470972,48.4157241439943));
#29826=CARTESIAN_POINT('Ctrl Pts',(-4.13369316567451,11.5743188502015,48.4275666875517));
#29827=CARTESIAN_POINT('Ctrl Pts',(-4.13722371861482,11.5746245485739,48.4275653153946));
#29828=CARTESIAN_POINT('Ctrl Pts',(-4.12845481065596,11.4732422824942,48.360331646857));
#29829=CARTESIAN_POINT('Ctrl Pts',(-4.12866555953595,11.5210597361567,48.3801951411646));
#29830=CARTESIAN_POINT('Ctrl Pts',(-4.13016261273423,11.5740131518293,48.4275680597092));
#29831=CARTESIAN_POINT('Ctrl Pts',(-4.13722371861483,11.5746245485739,48.4275653153946));
#29832=CARTESIAN_POINT('',(-4.12551258849077,11.6756605207468,48.495917442261));
#29833=CARTESIAN_POINT('Ctrl Pts',(-4.12551258849121,11.6756605207397,48.4959174422581));
#29834=CARTESIAN_POINT('Ctrl Pts',(-4.1258953594032,11.6686892977337,48.4930115088121));
#29835=CARTESIAN_POINT('Ctrl Pts',(-4.12627095135831,11.661843965821,48.4898115000955));
#29836=CARTESIAN_POINT('Ctrl Pts',(-4.12665447322118,11.6551189469296,48.4863820761544));
#29837=CARTESIAN_POINT('Ctrl Pts',(-4.1269487006233,11.649959697799,48.4837511166327));
#29838=CARTESIAN_POINT('Ctrl Pts',(-4.12724744290251,11.6448712703663,48.4809834473072));
#29839=CARTESIAN_POINT('Ctrl Pts',(-4.12755756488955,11.6398565149523,48.4780890456653));
#29840=CARTESIAN_POINT('Ctrl Pts',(-4.12790255670227,11.6342779051378,48.4748692002144));
#29841=CARTESIAN_POINT('Ctrl Pts',(-4.12826137312859,11.6287898949969,48.4714928657208));
#29842=CARTESIAN_POINT('Ctrl Pts',(-4.12864636713521,11.6234078109081,48.4679547934975));
#29843=CARTESIAN_POINT('Ctrl Pts',(-4.12882718134101,11.6208800903635,48.4662931216062));
#29844=CARTESIAN_POINT('Ctrl Pts',(-4.12901382912469,11.6183759600391,48.4645955090256));
#29845=CARTESIAN_POINT('Ctrl Pts',(-4.12920813507089,11.6158985300687,48.4628595640575));
#29846=CARTESIAN_POINT('Ctrl Pts',(-4.1293455880544,11.6141459839037,48.4616315480357));
#29847=CARTESIAN_POINT('Ctrl Pts',(-4.12948687798054,11.6124070235617,48.4603843962804));
#29848=CARTESIAN_POINT('Ctrl Pts',(-4.12963227160581,11.6106893807938,48.4591215269354));
#29849=CARTESIAN_POINT('Ctrl Pts',(-4.1297189685603,11.609665165347,48.4583684889261));
#29850=CARTESIAN_POINT('Ctrl Pts',(-4.12980723187199,11.6086472141289,48.457608922056));
#29851=CARTESIAN_POINT('Ctrl Pts',(-4.12989742751478,11.6076341633577,48.4568411226821));
#29852=CARTESIAN_POINT('Ctrl Pts',(-4.13014206460896,11.6048864719033,48.4547586251031));
#29853=CARTESIAN_POINT('Ctrl Pts',(-4.13040049692275,11.60216730197,48.4526172688089));
#29854=CARTESIAN_POINT('Ctrl Pts',(-4.1306843553102,11.599476279665,48.4504226933436));
#29855=CARTESIAN_POINT('Ctrl Pts',(-4.13087962948455,11.5976250496786,48.4489129831114));
#29856=CARTESIAN_POINT('Ctrl Pts',(-4.13108698032367,11.5957876815349,48.4473783076307));
#29857=CARTESIAN_POINT('Ctrl Pts',(-4.13131145786228,11.593976786229,48.4458307104849));
#29858=CARTESIAN_POINT('Ctrl Pts',(-4.13153926000086,11.5921390708566,48.4442601928212));
#29859=CARTESIAN_POINT('Ctrl Pts',(-4.13178482689973,11.5903229945745,48.442671860598));
#29860=CARTESIAN_POINT('Ctrl Pts',(-4.13206214386908,11.5885243391444,48.4410617399059));
#29861=CARTESIAN_POINT('Ctrl Pts',(-4.13233279400564,11.5867689242525,48.4394903272866));
#29862=CARTESIAN_POINT('Ctrl Pts',(-4.13263186492608,11.5850314713388,48.4378995371871));
#29863=CARTESIAN_POINT('Ctrl Pts',(-4.13299116528337,11.5833150139726,48.4362882720692));
#29864=CARTESIAN_POINT('Ctrl Pts',(-4.13323220081251,11.5821635338777,48.4352073598675));
#29865=CARTESIAN_POINT('Ctrl Pts',(-4.1334993953209,11.5810211498778,48.4341169808742));
#29866=CARTESIAN_POINT('Ctrl Pts',(-4.13382303553132,11.5798920643606,48.433017017294));
#29867=CARTESIAN_POINT('Ctrl Pts',(-4.13401325610055,11.5792284407351,48.4323705101802));
#29868=CARTESIAN_POINT('Ctrl Pts',(-4.13422283309914,11.5785688892838,48.4317201905913));
#29869=CARTESIAN_POINT('Ctrl Pts',(-4.13447082538378,11.577917245021,48.431067393103));
#29870=CARTESIAN_POINT('Ctrl Pts',(-4.13463747005405,11.5774793562235,48.4306287293665));
#29871=CARTESIAN_POINT('Ctrl Pts',(-4.13482261192084,11.5770415637595,48.4301854309067));
#29872=CARTESIAN_POINT('Ctrl Pts',(-4.13503924470767,11.576616631166,48.4297484868059));
#29873=CARTESIAN_POINT('Ctrl Pts',(-4.13517769151791,11.5763450630299,48.4294692422931));
#29874=CARTESIAN_POINT('Ctrl Pts',(-4.13533045467977,11.576074686727,48.429188484864));
#29875=CARTESIAN_POINT('Ctrl Pts',(-4.13551152790242,11.5758096277524,48.4289088568648));
#29876=CARTESIAN_POINT('Ctrl Pts',(-4.13563658855657,11.5756265612103,48.42871572803));
#29877=CARTESIAN_POINT('Ctrl Pts',(-4.13577439313221,11.5754472102307,48.4285243589121));
#29878=CARTESIAN_POINT('Ctrl Pts',(-4.13593295017201,11.5752795116543,48.4283419921649));
#29879=CARTESIAN_POINT('Ctrl Pts',(-4.13600396520959,11.5752044022759,48.4282603131589));
#29880=CARTESIAN_POINT('Ctrl Pts',(-4.13608017351886,11.5751304213442,48.4281791399513));
#29881=CARTESIAN_POINT('Ctrl Pts',(-4.13616638889705,11.5750574234697,48.4280978870178));
#29882=CARTESIAN_POINT('Ctrl Pts',(-4.13623123833384,11.5750025159677,48.42803677023));
#29883=CARTESIAN_POINT('Ctrl Pts',(-4.13629784753377,11.574949303433,48.427977124616));
#29884=CARTESIAN_POINT('Ctrl Pts',(-4.13639939779102,11.5748837650914,48.4279017477846));
#29885=CARTESIAN_POINT('Ctrl Pts',(-4.13645017291964,11.5748509959206,48.4278640593689));
#29886=CARTESIAN_POINT('Ctrl Pts',(-4.13650742313086,11.5748147554917,48.4278222495093));
#29887=CARTESIAN_POINT('Ctrl Pts',(-4.13660866417317,11.5747669664098,48.4277647101541));
#29888=CARTESIAN_POINT('Ctrl Pts',(-4.13665928465917,11.5747430718855,48.4277359404965));
#29889=CARTESIAN_POINT('Ctrl Pts',(-4.13671884717098,11.5747164083803,48.4277035354777));
#29890=CARTESIAN_POINT('Ctrl Pts',(-4.13681243800998,11.5746874268168,48.4276657143528));
#29891=CARTESIAN_POINT('Ctrl Pts',(-4.13689467272046,11.5746619618193,48.4276324823688));
#29892=CARTESIAN_POINT('Ctrl Pts',(-4.13700306041443,11.5746336393858,48.4275939402689));
#29893=CARTESIAN_POINT('Ctrl Pts',(-4.13715717683536,11.5746261598313,48.4275727843802));
#29894=CARTESIAN_POINT('Ctrl Pts',(-4.13717845940415,11.5746251269489,48.4275698628768));
#29895=CARTESIAN_POINT('Ctrl Pts',(-4.13720062027767,11.5746245484517,48.4275673318624));
#29896=CARTESIAN_POINT('Ctrl Pts',(-4.13722371782189,11.5746245485739,48.4275653154638));
#29897=CARTESIAN_POINT('Ctrl Pts',(-4.12551258849121,11.6756605207397,48.4959174422581));
#29898=CARTESIAN_POINT('Ctrl Pts',(-3.42379713716555,11.6392592214936,48.5061181031666));
#29899=CARTESIAN_POINT('Ctrl Pts',(-2.72152478000237,11.5986492866067,48.5108119661587));
#29900=CARTESIAN_POINT('Ctrl Pts',(-1.31995074912857,11.5098560202878,48.5141172996809));
#29901=CARTESIAN_POINT('Ctrl Pts',(-0.618564042211977,11.4835302569326,
48.5199462997129));
#29902=CARTESIAN_POINT('Ctrl Pts',(0.0835265683646154,11.4728541727075,
48.5199460669665));
#29903=CARTESIAN_POINT('Ctrl Pts',(48.5210408433891,11.4728541727075,0.0824317919368853));
#29904=CARTESIAN_POINT('Ctrl Pts',(48.5210413088829,11.4942063411577,0.0824317919368136));
#29905=CARTESIAN_POINT('Ctrl Pts',(48.5206840668827,11.5200575082527,0.082431791935498));
#29906=CARTESIAN_POINT('Ctrl Pts',(48.5224494671721,11.5731362269333,0.0824317919377551));
#29907=CARTESIAN_POINT('Ctrl Pts',(48.521026568362,11.5876793312944,0.082431791938572));
#29908=CARTESIAN_POINT('Ctrl Pts',(48.521026568362,11.6131136241746,0.0824317919395203));
#29909=CARTESIAN_POINT('Ctrl Pts',(48.5210409597623,11.4781922148201,0.4334770972252));
#29910=CARTESIAN_POINT('Ctrl Pts',(48.5209817377046,11.4971000233707,0.355275148040153));
#29911=CARTESIAN_POINT('Ctrl Pts',(48.5206817360346,11.5200113925674,0.355061808308312));
#29912=CARTESIAN_POINT('Ctrl Pts',(48.5224506910052,11.5731490589917,0.393775030003177));
#29913=CARTESIAN_POINT('Ctrl Pts',(48.521026568362,11.5876793312944,0.432701591427231));
#29914=CARTESIAN_POINT('Ctrl Pts',(48.521026568362,11.6131136241746,0.432779444551026));
#29915=CARTESIAN_POINT('Ctrl Pts',(48.5195837679409,11.4874426767152,0.784346426598513));
#29916=CARTESIAN_POINT('Ctrl Pts',(48.5206699839161,11.5031786713302,0.650878763011595));
#29917=CARTESIAN_POINT('Ctrl Pts',(48.520785019491,11.5245005081761,0.650515563920166));
#29918=CARTESIAN_POINT('Ctrl Pts',(48.5225859377424,11.5776504745526,0.716581364265669));
#29919=CARTESIAN_POINT('Ctrl Pts',(48.521026568362,11.5930695682598,0.783010363700175));
#29920=CARTESIAN_POINT('Ctrl Pts',(48.521026568362,11.6169153282063,0.783127097162531));
#29921=CARTESIAN_POINT('Ctrl Pts',(48.5162561594212,11.5143737377389,1.48575918656021));
#29922=CARTESIAN_POINT('Ctrl Pts',(48.5194060548862,11.5255419633077,1.29343922056592));
#29923=CARTESIAN_POINT('Ctrl Pts',(48.520440782358,11.5448479357173,1.29287966906623));
#29924=CARTESIAN_POINT('Ctrl Pts',(48.5225314340558,11.595969244612,1.38797527793364));
#29925=CARTESIAN_POINT('Ctrl Pts',(48.5210265683621,11.6126245374907,1.48363043829888));
#29926=CARTESIAN_POINT('Ctrl Pts',(48.5210265683621,11.632122144333,1.48373989603257));
#29927=CARTESIAN_POINT('Ctrl Pts',(48.5143857427228,11.5320543368676,1.83630261714859));
#29928=CARTESIAN_POINT('Ctrl Pts',(48.5184689188545,11.5418711528743,1.64039290832512));
#29929=CARTESIAN_POINT('Ctrl Pts',(48.5200083009784,11.5607507931985,1.63978686377675));
#29930=CARTESIAN_POINT('Ctrl Pts',(48.5223492032368,11.6098088718849,1.73656127992728));
#29931=CARTESIAN_POINT('Ctrl Pts',(48.5210265683621,11.6267892697561,1.83394174062464));
#29932=CARTESIAN_POINT('Ctrl Pts',(48.5210265683621,11.643527256428,1.83400504229111));
#29933=CARTESIAN_POINT('Ctrl Pts',(48.5119067425813,11.5986492866067,2.88748314030395));
#29934=CARTESIAN_POINT('Ctrl Pts',(48.5182994308552,11.612020620858,2.7670415434901));
#29935=CARTESIAN_POINT('Ctrl Pts',(48.5205482384131,11.6290600690796,2.76641567761564));
#29936=CARTESIAN_POINT('Ctrl Pts',(48.522328768896,11.6658592241822,2.82527806557464));
#29937=CARTESIAN_POINT('Ctrl Pts',(48.521026568362,11.6794362415567,2.88476631940751));
#29938=CARTESIAN_POINT('Ctrl Pts',(48.521026568362,11.689147704808,2.8845529620078));
#29939=CARTESIAN_POINT('Ctrl Pts',(48.5072128795892,11.6392592214936,3.58975549746708));
#29940=CARTESIAN_POINT('Ctrl Pts',(48.5152097045281,11.6580360440914,3.51781324718459));
#29941=CARTESIAN_POINT('Ctrl Pts',(48.5186631267213,11.6785648284689,3.51681245255117));
#29942=CARTESIAN_POINT('Ctrl Pts',(48.5215715586383,11.7135824344711,3.55049096279398));
#29943=CARTESIAN_POINT('Ctrl Pts',(48.521026568362,11.7280712560958,3.58517026767022));
#29944=CARTESIAN_POINT('Ctrl Pts',(48.521026568362,11.734768153188,3.58458821640705));
#29945=CARTESIAN_POINT('Ctrl Pts',(48.4970122186807,11.6756605207398,4.29147094879272));
#29946=CARTESIAN_POINT('Ctrl Pts',(48.5070083851258,11.6996409410726,4.29015424907548));
#29947=CARTESIAN_POINT('Ctrl Pts',(48.5130119725461,11.7229366511894,4.28885904835369));
#29948=CARTESIAN_POINT('Ctrl Pts',(48.5200210641643,11.7642258753785,4.28634531528796));
#29949=CARTESIAN_POINT('Ctrl Pts',(48.521026568362,11.7822193894509,4.28512678294403));
#29950=CARTESIAN_POINT('Ctrl Pts',(48.521026568362,11.7955954176946,4.28396341998253));
#29951=CARTESIAN_POINT('',(48.4970121852286,11.675660534618,4.29147094758644));
#29952=CARTESIAN_POINT('',(48.5210408433891,11.4728541727075,0.0824317919368853));
#29953=CARTESIAN_POINT('Ctrl Pts',(48.4970122186807,11.6756605207397,4.29147094879272));
#29954=CARTESIAN_POINT('Ctrl Pts',(48.5072128795892,11.6392592214936,3.58975549746708));
#29955=CARTESIAN_POINT('Ctrl Pts',(48.5119067425813,11.5986492866067,2.88748314030395));
#29956=CARTESIAN_POINT('Ctrl Pts',(48.5152120761034,11.5098560202879,1.48590910943014));
#29957=CARTESIAN_POINT('Ctrl Pts',(48.5210410761356,11.4835302569327,0.784522402513517));
#29958=CARTESIAN_POINT('Ctrl Pts',(48.5210408433891,11.4728541727075,0.0824317919368853));
#29959=CARTESIAN_POINT('Ctrl Pts',(48.4970121183243,11.6756605623744,4.29147094517387));
#29960=CARTESIAN_POINT('Ctrl Pts',(48.5011284587564,11.6855354834088,4.29092874030659));
#29961=CARTESIAN_POINT('Ctrl Pts',(48.5046183464519,11.6953464500614,4.29038568916614));
#29962=CARTESIAN_POINT('Ctrl Pts',(48.5075262052002,11.7049048876128,4.28984737507277));
#29963=CARTESIAN_POINT('Ctrl Pts',(48.5106115103027,11.7150466099943,4.28927621142185));
#29964=CARTESIAN_POINT('Ctrl Pts',(48.5130422894378,11.7249027978756,4.28871048915178));
#29965=CARTESIAN_POINT('Ctrl Pts',(48.5149248520449,11.734276287982,4.2881544780866));
#29966=CARTESIAN_POINT('Ctrl Pts',(48.5168934367235,11.7440780916189,4.28757306057625));
#29967=CARTESIAN_POINT('Ctrl Pts',(48.5182641071096,11.7533514160685,4.28700232059462));
#29968=CARTESIAN_POINT('Ctrl Pts',(48.5191968155257,11.7619163369651,4.2864432162865));
#29969=CARTESIAN_POINT('Ctrl Pts',(48.5202107580794,11.7712272187112,4.28583541684976));
#29970=CARTESIAN_POINT('Ctrl Pts',(48.5207093509836,11.779700856982,4.28524137620842));
#29971=CARTESIAN_POINT('Ctrl Pts',(48.5209120861297,11.787166042447,4.28465712816846));
#29972=CARTESIAN_POINT('Ctrl Pts',(48.5209927949347,11.7901379306939,4.28442453918706));
#29973=CARTESIAN_POINT('Ctrl Pts',(48.5210265662916,11.7929506159592,4.28419344823332));
#29974=CARTESIAN_POINT('Ctrl Pts',(48.5210265683619,11.7955954176946,4.28396341998252));
#29975=CARTESIAN_POINT('Ctrl Pts',(48.5210265683621,11.6131136241746,0.0824317919395203));
#29976=CARTESIAN_POINT('Ctrl Pts',(48.521026568362,11.5876793312944,0.082431791938572));
#29977=CARTESIAN_POINT('Ctrl Pts',(48.5224494671721,11.5731362269333,0.0824317919377551));
#29978=CARTESIAN_POINT('Ctrl Pts',(48.5206840668827,11.5200575082527,0.082431791935498));
#29979=CARTESIAN_POINT('Ctrl Pts',(48.5210413088829,11.4942063411577,0.0824317919368136));
#29980=CARTESIAN_POINT('Ctrl Pts',(48.5210408433891,11.4728541727075,0.0824317919368853));
#29981=CARTESIAN_POINT('Ctrl Pts',(48.5210408433891,11.4728541727075,0.0824317919368853));
#29982=CARTESIAN_POINT('Ctrl Pts',(48.5210409597627,11.4781922148199,-0.268613513351465));
#29983=CARTESIAN_POINT('Ctrl Pts',(48.5195837679418,11.4874426767152,-0.619482842725758));
#29984=CARTESIAN_POINT('Ctrl Pts',(48.5162561594226,11.5143737377394,-1.32089560269132));
#29985=CARTESIAN_POINT('Ctrl Pts',(48.5143857427244,11.5320543368685,-1.67143903328259));
#29986=CARTESIAN_POINT('Ctrl Pts',(48.5119067425819,11.598649286609,-2.72261955644951));
#29987=CARTESIAN_POINT('Ctrl Pts',(48.5072128795897,11.6392592214975,-3.42489191363272));
#29988=CARTESIAN_POINT('Ctrl Pts',(48.4970122186807,11.6756605207451,-4.1266073649755));
#29989=CARTESIAN_POINT('Ctrl Pts',(48.5210413088829,11.4942063411577,0.0824317919368136));
#29990=CARTESIAN_POINT('Ctrl Pts',(48.520981737705,11.4971000233707,-0.190411564166736));
#29991=CARTESIAN_POINT('Ctrl Pts',(48.5206699839168,11.5031786713304,-0.486015179139394));
#29992=CARTESIAN_POINT('Ctrl Pts',(48.5194060548872,11.5255419633083,-1.12857563669724));
#29993=CARTESIAN_POINT('Ctrl Pts',(48.5184689188556,11.5418711528751,-1.47552932445875));
#29994=CARTESIAN_POINT('Ctrl Pts',(48.5182994308554,11.6120206208596,-2.6021779596309));
#29995=CARTESIAN_POINT('Ctrl Pts',(48.5152097045281,11.6580360440938,-3.35294966333778));
#29996=CARTESIAN_POINT('Ctrl Pts',(48.5070083851259,11.6996409410751,-4.12529066522578));
#29997=CARTESIAN_POINT('Ctrl Pts',(48.5206840668827,11.5200575082527,0.082431791935498));
#29998=CARTESIAN_POINT('Ctrl Pts',(48.5206817360349,11.5200113925674,-0.190198224437316));
#29999=CARTESIAN_POINT('Ctrl Pts',(48.5207850194913,11.5245005081763,-0.485651980049793));
#30000=CARTESIAN_POINT('Ctrl Pts',(48.5204407823581,11.5448479357178,-1.12801608519759));
#30001=CARTESIAN_POINT('Ctrl Pts',(48.5200083009782,11.5607507931991,-1.47492327990924));
#30002=CARTESIAN_POINT('Ctrl Pts',(48.5205482384117,11.6290600690807,-2.60155209375108));
#30003=CARTESIAN_POINT('Ctrl Pts',(48.5186631267198,11.6785648284704,-3.35194886869318));
#30004=CARTESIAN_POINT('Ctrl Pts',(48.5130119725462,11.7229366511906,-4.12399546448852));
#30005=CARTESIAN_POINT('Ctrl Pts',(48.5224494671721,11.5731362269333,0.0824317919377551));
#30006=CARTESIAN_POINT('Ctrl Pts',(48.5224506910053,11.5731490589917,-0.228911446127667));
#30007=CARTESIAN_POINT('Ctrl Pts',(48.5225859377421,11.5776504745527,-0.551717780390339));
#30008=CARTESIAN_POINT('Ctrl Pts',(48.5225314340542,11.5959692446123,-1.22311169405866));
#30009=CARTESIAN_POINT('Ctrl Pts',(48.5223492032345,11.6098088718852,-1.57169769605248));
#30010=CARTESIAN_POINT('Ctrl Pts',(48.5223287688919,11.6658592241826,-2.6604144816998));
#30011=CARTESIAN_POINT('Ctrl Pts',(48.5215715586341,11.7135824344715,-3.38562737891988));
#30012=CARTESIAN_POINT('Ctrl Pts',(48.5200210641643,11.7642258753785,-4.12148173140813));
#30013=CARTESIAN_POINT('Ctrl Pts',(48.521026568362,11.5876793312944,0.082431791938572));
#30014=CARTESIAN_POINT('Ctrl Pts',(48.521026568362,11.5876793312944,-0.267838007550087));
#30015=CARTESIAN_POINT('Ctrl Pts',(48.5210265683614,11.5930695682598,-0.618146779822911));
#30016=CARTESIAN_POINT('Ctrl Pts',(48.5210265683597,11.6126245374908,-1.31876685442126));
#30017=CARTESIAN_POINT('Ctrl Pts',(48.5210265683587,11.6267892697563,-1.66907815674678));
#30018=CARTESIAN_POINT('Ctrl Pts',(48.5210265683567,11.6794362415569,-2.71990273552893));
#30019=CARTESIAN_POINT('Ctrl Pts',(48.5210265683567,11.728071256096,-3.42030668379117));
#30020=CARTESIAN_POINT('Ctrl Pts',(48.5210265683621,11.7822193894509,-4.12026319906499));
#30021=CARTESIAN_POINT('Ctrl Pts',(48.521026568362,11.6131136241746,0.0824317919395203));
#30022=CARTESIAN_POINT('Ctrl Pts',(48.521026568362,11.6131136241746,-0.267915860671985));
#30023=CARTESIAN_POINT('Ctrl Pts',(48.5210265683614,11.6169153282063,-0.618263513283491));
#30024=CARTESIAN_POINT('Ctrl Pts',(48.5210265683599,11.6321221443329,-1.31887631215353));
#30025=CARTESIAN_POINT('Ctrl Pts',(48.5210265683589,11.643527256428,-1.66914145841207));
#30026=CARTESIAN_POINT('Ctrl Pts',(48.521026568357,11.689147704808,-2.71968937812876));
#30027=CARTESIAN_POINT('Ctrl Pts',(48.521026568357,11.734768153188,-3.41972463252801));
#30028=CARTESIAN_POINT('Ctrl Pts',(48.5210265683621,11.7955954176946,-4.11909983610349));
#30029=CARTESIAN_POINT('',(48.4970121851698,11.6756605346477,-4.12660736376709));
#30030=CARTESIAN_POINT('Ctrl Pts',(48.521026568362,11.7955954176945,-4.11909983610349));
#30031=CARTESIAN_POINT('Ctrl Pts',(48.5210265631159,11.7889074035727,-4.11968151758424));
#30032=CARTESIAN_POINT('Ctrl Pts',(48.5208120576626,11.7811426004669,-4.12027027886023));
#30033=CARTESIAN_POINT('Ctrl Pts',(48.5201636703024,11.7724551591809,-4.12087195425065));
#30034=CARTESIAN_POINT('Ctrl Pts',(48.5195714197326,11.7645198686933,-4.12142153713069));
#30035=CARTESIAN_POINT('Ctrl Pts',(48.5186152663071,11.7558145072651,-4.12198191714169));
#30036=CARTESIAN_POINT('Ctrl Pts',(48.5171273935807,11.746498740511,-4.12255387295054));
#30037=CARTESIAN_POINT('Ctrl Pts',(48.5157117221484,11.7376350355518,-4.12309807373113));
#30038=CARTESIAN_POINT('Ctrl Pts',(48.5138132535906,11.7282190174497,-4.12365272793901));
#30039=CARTESIAN_POINT('Ctrl Pts',(48.5113099337767,11.7184280696927,-4.12421506208217));
#30040=CARTESIAN_POINT('Ctrl Pts',(48.5089256148278,11.7091025563742,-4.12475066442339));
#30041=CARTESIAN_POINT('Ctrl Pts',(48.5059916763245,11.6994377386554,-4.12529316148933));
#30042=CARTESIAN_POINT('Ctrl Pts',(48.502440122712,11.6896156896681,-4.12583768361868));
#30043=CARTESIAN_POINT('Ctrl Pts',(48.5007681263605,11.6849916766689,-4.12609403312455));
#30044=CARTESIAN_POINT('Ctrl Pts',(48.4989598840261,11.6803331677638,-4.12635080138442));
#30045=CARTESIAN_POINT('Ctrl Pts',(48.4970121181478,11.675660562453,-4.12660736135028));
#30046=CARTESIAN_POINT('Ctrl Pts',(48.4970122186807,11.6756605207451,-4.12660736497549));
#30047=CARTESIAN_POINT('Ctrl Pts',(48.5072128795897,11.6392592214975,-3.42489191363272));
#30048=CARTESIAN_POINT('Ctrl Pts',(48.5119067425819,11.598649286609,-2.72261955644951));
#30049=CARTESIAN_POINT('Ctrl Pts',(48.5152120761052,11.5098560202883,-1.32104552556029));
#30050=CARTESIAN_POINT('Ctrl Pts',(48.5210410761364,11.4835302569324,-0.619658818639818));
#30051=CARTESIAN_POINT('Ctrl Pts',(48.5210408433891,11.4728541727075,0.0824317919368853));
#30052=CARTESIAN_POINT('Ctrl Pts',(48.5210408433891,11.4728541727075,0.0824317919368853));
#30053=CARTESIAN_POINT('Ctrl Pts',(48.5210407270158,11.4675161305948,-0.268613513351429));
#30054=CARTESIAN_POINT('Ctrl Pts',(48.5195832988726,11.465926508769,-0.619710756297191));
#30055=CARTESIAN_POINT('Ctrl Pts',(48.5098524785203,11.464396632877,-1.32203631985499));
#30056=CARTESIAN_POINT('Ctrl Pts',(48.5015790863112,11.4644563788107,-1.67326464046703));
#30057=CARTESIAN_POINT('Ctrl Pts',(48.4606829527964,11.4583384590299,-2.72718702232965));
#30058=CARTESIAN_POINT('Ctrl Pts',(48.4174823766519,11.4609474762042,-3.42843979480817));
#30059=CARTESIAN_POINT('Ctrl Pts',(48.3614264232796,11.4732422824942,-4.1295495870784));
#30060=CARTESIAN_POINT('Ctrl Pts',(48.5210409597627,11.4781922148199,-0.268613513351465));
#30061=CARTESIAN_POINT('Ctrl Pts',(48.5200991113392,11.474986089803,-0.541629933632588));
#30062=CARTESIAN_POINT('Ctrl Pts',(48.5180114541286,11.4745419834777,-0.832717796196048));
#30063=CARTESIAN_POINT('Ctrl Pts',(48.5081357594276,11.4744825705814,-1.44781988667443));
#30064=CARTESIAN_POINT('Ctrl Pts',(48.5003285876198,11.4748353413217,-1.77183914952693));
#30065=CARTESIAN_POINT('Ctrl Pts',(48.4602502314476,11.4700074930207,-2.78846829308488));
#30066=CARTESIAN_POINT('Ctrl Pts',(48.4187304434639,11.4731609516944,-3.46541553760946));
#30067=CARTESIAN_POINT('Ctrl Pts',(48.3663922968565,11.4851966459098,-4.1296022742984));
#30068=CARTESIAN_POINT('Ctrl Pts',(48.5195837679418,11.4874426767152,-0.619482842725758));
#30069=CARTESIAN_POINT('Ctrl Pts',(48.5183837318974,11.4844803122479,-0.832372602290194));
#30070=CARTESIAN_POINT('Ctrl Pts',(48.5159956580517,11.4840908039498,-1.077403162417));
#30071=CARTESIAN_POINT('Ctrl Pts',(48.5060961369527,11.4843329006937,-1.62174846129248));
#30072=CARTESIAN_POINT('Ctrl Pts',(48.4985559882231,11.4849166217029,-1.92107075244751));
#30073=CARTESIAN_POINT('Ctrl Pts',(48.4596398458091,11.4818828006799,-2.8854776387807));
#30074=CARTESIAN_POINT('Ctrl Pts',(48.4200748650815,11.4863352799679,-3.52759295216471));
#30075=CARTESIAN_POINT('Ctrl Pts',(48.3730775094482,11.4974720069511,-4.1297353555383));
#30076=CARTESIAN_POINT('Ctrl Pts',(48.5162561594226,11.5143737377394,-1.32089560269132));
#30077=CARTESIAN_POINT('Ctrl Pts',(48.5144994210143,11.5105174196342,-1.44625764302723));
#30078=CARTESIAN_POINT('Ctrl Pts',(48.5114095528574,11.5090816899186,-1.62044191411888));
#30079=CARTESIAN_POINT('Ctrl Pts',(48.5010454693472,11.5079260458441,-2.04438576003036));
#30080=CARTESIAN_POINT('Ctrl Pts',(48.4937353771487,11.5081462764441,-2.29415477535813));
#30081=CARTESIAN_POINT('Ctrl Pts',(48.4576393364517,11.5065304546904,-3.12373338862082));
#30082=CARTESIAN_POINT('Ctrl Pts',(48.4227028837573,11.5121367174566,-3.6727550868809));
#30083=CARTESIAN_POINT('Ctrl Pts',(48.3875464536895,11.5208685373805,-4.13029598569424));
#30084=CARTESIAN_POINT('Ctrl Pts',(48.5143857427244,11.5320543368685,-1.67143903328259));
#30085=CARTESIAN_POINT('Ctrl Pts',(48.512333338594,11.5270830007425,-1.76939839553984));
#30086=CARTESIAN_POINT('Ctrl Pts',(48.5088435172715,11.5245577996658,-1.91879287024956));
#30087=CARTESIAN_POINT('Ctrl Pts',(48.4980397661311,11.5217114161951,-2.29309144746239));
#30088=CARTESIAN_POINT('Ctrl Pts',(48.4906923512577,11.5213343690961,-2.51800436110623));
#30089=CARTESIAN_POINT('Ctrl Pts',(48.4562520617536,11.5193254972085,-3.26497817319829));
#30090=CARTESIAN_POINT('Ctrl Pts',(48.4239864808155,11.5247638266718,-3.75573980704184));
#30091=CARTESIAN_POINT('Ctrl Pts',(48.395330185339,11.5319897067687,-4.13072353461029));
#30092=CARTESIAN_POINT('Ctrl Pts',(48.5119067425819,11.598649286609,-2.72261955644951));
#30093=CARTESIAN_POINT('Ctrl Pts',(48.5086939112097,11.5919036248663,-2.78284526372885));
#30094=CARTESIAN_POINT('Ctrl Pts',(48.5036610022595,11.5859418512212,-2.87982118572785));
#30095=CARTESIAN_POINT('Ctrl Pts',(48.4906361947483,11.5755468354635,-3.11912189520875));
#30096=CARTESIAN_POINT('Ctrl Pts',(48.4826251618699,11.5710816706623,-3.26145171762822));
#30097=CARTESIAN_POINT('Ctrl Pts',(48.4521822008654,11.5598336028535,-3.71424372296942));
#30098=CARTESIAN_POINT('Ctrl Pts',(48.4273657338961,11.5581209387927,-3.9915108690798));
#30099=CARTESIAN_POINT('Ctrl Pts',(48.4168189204169,11.5609276470972,-4.13264840232726));
#30100=CARTESIAN_POINT('Ctrl Pts',(48.5072128795897,11.6392592214975,-3.42489191363272));
#30101=CARTESIAN_POINT('Ctrl Pts',(48.5032144671204,11.6298708101994,-3.46086303878018));
#30102=CARTESIAN_POINT('Ctrl Pts',(48.4973225964204,11.6209827896646,-3.52283173406414));
#30103=CARTESIAN_POINT('Ctrl Pts',(48.4830998624069,11.6050189470302,-3.6684275949641));
#30104=CARTESIAN_POINT('Ctrl Pts',(48.4747689990933,11.5979431249305,-3.75205476058009));
#30105=CARTESIAN_POINT('Ctrl Pts',(48.4481398060047,11.5806510816468,-3.9899189580147));
#30106=CARTESIAN_POINT('Ctrl Pts',(48.4289898518242,11.5743267261738,-4.13111411251199));
#30107=CARTESIAN_POINT('Ctrl Pts',(48.4286614639744,11.5743188502015,-4.13478794209698));
#30108=CARTESIAN_POINT('Ctrl Pts',(48.4970122186807,11.6756605207451,-4.1266073649755));
#30109=CARTESIAN_POINT('Ctrl Pts',(48.4920141354582,11.6636703105801,-4.12726571485037));
#30110=CARTESIAN_POINT('Ctrl Pts',(48.4858839393056,11.6514649415887,-4.12793445428902));
#30111=CARTESIAN_POINT('Ctrl Pts',(48.4724837048702,11.6282480883359,-4.12937022856651));
#30112=CARTESIAN_POINT('Ctrl Pts',(48.4652136665875,11.6172366040747,-4.13013726340536));
#30113=CARTESIAN_POINT('Ctrl Pts',(48.4433803641393,11.588429281961,-4.13270208543106));
#30114=CARTESIAN_POINT('Ctrl Pts',(48.4289711156128,11.5746245276893,-4.13475573974208));
#30115=CARTESIAN_POINT('Ctrl Pts',(48.4286600918172,11.5746245485739,-4.13831849503729));
#30116=CARTESIAN_POINT('Ctrl Pts',(48.4970122186807,11.6756605207451,-4.12660736497549));
#30117=CARTESIAN_POINT('Ctrl Pts',(48.4870160522356,11.6516801004151,-4.12792406472524));
#30118=CARTESIAN_POINT('Ctrl Pts',(48.4724914340702,11.6268390447793,-4.12928232273011));
#30119=CARTESIAN_POINT('Ctrl Pts',(48.4433803641393,11.588429281961,-4.13270208543106));
#30120=CARTESIAN_POINT('Ctrl Pts',(48.4289711156128,11.5746245276893,-4.13475573974208));
#30121=CARTESIAN_POINT('Ctrl Pts',(48.4286600918172,11.5746245485739,-4.13831849503729));
#30122=CARTESIAN_POINT('',(48.3614264232796,11.4732422824942,-4.1295495870784));
#30123=CARTESIAN_POINT('Ctrl Pts',(48.4286600918172,11.5746245485739,-4.13831849503729));
#30124=CARTESIAN_POINT('Ctrl Pts',(48.4286628361315,11.5740131518292,-4.13125738915667));
#30125=CARTESIAN_POINT('Ctrl Pts',(48.3812899175873,11.5210597361567,-4.12976033595841));
#30126=CARTESIAN_POINT('Ctrl Pts',(48.3614264232796,11.4732422824942,-4.1295495870784));
#30127=CARTESIAN_POINT('Ctrl Pts',(48.3614264232796,11.4732422824942,-4.1295495870784));
#30128=CARTESIAN_POINT('Ctrl Pts',(48.4174823766519,11.4609474762041,-3.42843979480816));
#30129=CARTESIAN_POINT('Ctrl Pts',(48.4606829527965,11.45833845903,-2.72718702232965));
#30130=CARTESIAN_POINT('Ctrl Pts',(48.5152111308162,11.4664956854043,-1.32195717984616));
#30131=CARTESIAN_POINT('Ctrl Pts',(48.5210406106426,11.4621780884822,-0.619658818639743));
#30132=CARTESIAN_POINT('Ctrl Pts',(48.5210408433891,11.4728541727075,0.0824317919368853));
#30133=CARTESIAN_POINT('Ctrl Pts',(48.5210408433891,11.4728541727075,0.0824317919368853));
#30134=CARTESIAN_POINT('Ctrl Pts',(48.5210403778953,11.4515020042572,0.0824317919369568));
#30135=CARTESIAN_POINT('Ctrl Pts',(48.5206820691924,11.4284235901226,0.0824317919383984));
#30136=CARTESIAN_POINT('Ctrl Pts',(48.5165774170445,11.3941472536996,0.0824317919386741));
#30137=CARTESIAN_POINT('Ctrl Pts',(48.521026568362,11.3720285904897,0.0824317919387195));
#30138=CARTESIAN_POINT('Ctrl Pts',(48.521026568362,11.353653679453,0.0824317919395275));
#30139=CARTESIAN_POINT('Ctrl Pts',(48.5210407270158,11.4675161305948,-0.268613513351429));
#30140=CARTESIAN_POINT('Ctrl Pts',(48.5209806868526,11.4488974993901,-0.19075769252117));
#30141=CARTESIAN_POINT('Ctrl Pts',(48.5207163683071,11.4285976962987,-0.173571652692277));
#30142=CARTESIAN_POINT('Ctrl Pts',(48.5165547845964,11.3940705712691,-0.195374050131769));
#30143=CARTESIAN_POINT('Ctrl Pts',(48.521026568362,11.3720285904897,-0.234362487399122));
#30144=CARTESIAN_POINT('Ctrl Pts',(48.521026568362,11.353653679453,-0.268855620758342));
#30145=CARTESIAN_POINT('Ctrl Pts',(48.5195832988726,11.465926508769,-0.619710756297191));
#30146=CARTESIAN_POINT('Ctrl Pts',(48.5197866644935,11.447718516688,-0.486342918210061));
#30147=CARTESIAN_POINT('Ctrl Pts',(48.5193523631262,11.428587933622,-0.460576104880735));
#30148=CARTESIAN_POINT('Ctrl Pts',(48.5144416806968,11.3934281614349,-0.501601281203803));
#30149=CARTESIAN_POINT('Ctrl Pts',(48.517908907227,11.3718199008203,-0.568393270855329));
#30150=CARTESIAN_POINT('Ctrl Pts',(48.5172052126372,11.3536536794531,-0.620143038727369));
#30151=CARTESIAN_POINT('Ctrl Pts',(48.5098524785203,11.464396632877,-1.32203631985499));
#30152=CARTESIAN_POINT('Ctrl Pts',(48.5114206543114,11.4452664260876,-1.12899681037143));
#30153=CARTESIAN_POINT('Ctrl Pts',(48.5102621676323,11.4271829834973,-1.09680529269933));
#30154=CARTESIAN_POINT('Ctrl Pts',(48.503189825889,11.3913038531299,-1.16128319676548));
#30155=CARTESIAN_POINT('Ctrl Pts',(48.5037480059623,11.3711415135622,-1.25795261850317));
#30156=CARTESIAN_POINT('Ctrl Pts',(48.5019179682627,11.3536536794531,-1.32263498783753));
#30157=CARTESIAN_POINT('Ctrl Pts',(48.5015790863112,11.4644563788107,-1.67326464046703));
#30158=CARTESIAN_POINT('Ctrl Pts',(48.5041223947664,11.443938017789,-1.47607399129227));
#30159=CARTESIAN_POINT('Ctrl Pts',(48.5024096539486,11.4257324956489,-1.44603650678937));
#30160=CARTESIAN_POINT('Ctrl Pts',(48.4939878357291,11.389794304459,-1.51473806913817));
#30161=CARTESIAN_POINT('Ctrl Pts',(48.4927046623486,11.3706718159735,-1.61347711598941));
#30162=CARTESIAN_POINT('Ctrl Pts',(48.4904520792406,11.3536536794531,-1.67383952952162));
#30163=CARTESIAN_POINT('Ctrl Pts',(48.4743149973013,11.4603777656235,-2.37587956170877));
#30164=CARTESIAN_POINT('Ctrl Pts',(48.475786514634,11.4381382649982,-2.22841054012373));
#30165=CARTESIAN_POINT('Ctrl Pts',(48.4732866422588,11.4203247666438,-2.20690346123993));
#30166=CARTESIAN_POINT('Ctrl Pts',(48.4648102885898,11.3861758639155,-2.25918163609709));
#30167=CARTESIAN_POINT('Ctrl Pts',(48.4621240605424,11.3696277842964,-2.33296688983783));
#30168=CARTESIAN_POINT('Ctrl Pts',(48.4598703086856,11.3536536794531,-2.3760825335012));
#30169=CARTESIAN_POINT('Ctrl Pts',(48.4566988310128,11.4600103666203,-2.72684648513884));
#30170=CARTESIAN_POINT('Ctrl Pts',(48.4570444617159,11.4370088609558,-2.60397205099813));
#30171=CARTESIAN_POINT('Ctrl Pts',(48.4539681826041,11.4187667259072,-2.58894423029257));
#30172=CARTESIAN_POINT('Ctrl Pts',(48.4456390892507,11.3847952022384,-2.63542225695827));
#30173=CARTESIAN_POINT('Ctrl Pts',(48.442587008597,11.369053450208,-2.69692810432937));
#30174=CARTESIAN_POINT('Ctrl Pts',(48.4407544264067,11.3536536794531,-2.72712100634157));
#30175=CARTESIAN_POINT('Ctrl Pts',(48.4142685323449,11.4633689234831,-3.42840404975609));
#30176=CARTESIAN_POINT('Ctrl Pts',(48.4107714341872,11.4394032486783,-3.36074991139726));
#30177=CARTESIAN_POINT('Ctrl Pts',(48.4062756535774,11.4193327724023,-3.3565532039196));
#30178=CARTESIAN_POINT('Ctrl Pts',(48.3983980635604,11.3835624194323,-3.38631956505366));
#30179=CARTESIAN_POINT('Ctrl Pts',(48.395571861118,11.3679565169509,-3.42028263366534));
#30180=CARTESIAN_POINT('Ctrl Pts',(48.3948635884079,11.3536536794531,-3.42894804748508));
#30181=CARTESIAN_POINT('Ctrl Pts',(48.3894543999657,11.4670948793492,-3.77899469094328));
#30182=CARTESIAN_POINT('Ctrl Pts',(48.3832404595767,11.4429270404433,-3.74196626092199));
#30183=CARTESIAN_POINT('Ctrl Pts',(48.3779018427096,11.4214568596339,-3.74211938411377));
#30184=CARTESIAN_POINT('Ctrl Pts',(48.3703287539371,11.3837102983034,-3.76097220616443));
#30185=CARTESIAN_POINT('Ctrl Pts',(48.3680942820317,11.3674339177823,-3.7796719050233));
#30186=CARTESIAN_POINT('Ctrl Pts',(48.3680886315664,11.3536536794531,-3.77973662633619));
#30187=CARTESIAN_POINT('Ctrl Pts',(48.3614264232796,11.4732422824942,-4.1295495870784));
#30188=CARTESIAN_POINT('Ctrl Pts',(48.3514946761257,11.4493335556629,-4.12944421263839));
#30189=CARTESIAN_POINT('Ctrl Pts',(48.3455075205231,11.4261172510678,-4.12964628233286));
#30190=CARTESIAN_POINT('Ctrl Pts',(48.3384990828948,11.384958159128,-4.13010310894181));
#30191=CARTESIAN_POINT('Ctrl Pts',(48.3374778008691,11.3670153717833,-4.13035786585628));
#30192=CARTESIAN_POINT('Ctrl Pts',(48.3374778008691,11.3536536794531,-4.13035786585628));
#30193=CARTESIAN_POINT('Ctrl Pts',(48.3614264232796,11.4732422824942,-4.1295495870784));
#30194=CARTESIAN_POINT('Ctrl Pts',(48.35699350214,11.4625708971931,-4.12950255440878));
#30195=CARTESIAN_POINT('Ctrl Pts',(48.3532977193535,11.4520014357868,-4.12951249962561));
#30196=CARTESIAN_POINT('Ctrl Pts',(48.3502685940128,11.4417444398152,-4.12955963932613));
#30197=CARTESIAN_POINT('Ctrl Pts',(48.3470288568254,11.4307742858787,-4.12961005659963));
#30198=CARTESIAN_POINT('Ctrl Pts',(48.3445511740643,11.4201626014222,-4.12970297530091));
#30199=CARTESIAN_POINT('Ctrl Pts',(48.3426934184697,11.410143434642,-4.12980930460507));
#30200=CARTESIAN_POINT('Ctrl Pts',(48.3407233191754,11.3995183806998,-4.12992206394097));
#30201=CARTESIAN_POINT('Ctrl Pts',(48.3394488499117,11.389560407305,-4.13004977115178));
#30202=CARTESIAN_POINT('Ctrl Pts',(48.3386560089339,11.3805081454717,-4.13015382200378));
#30203=CARTESIAN_POINT('Ctrl Pts',(48.3377632333477,11.3703148802494,-4.13027098807239));
#30204=CARTESIAN_POINT('Ctrl Pts',(48.3374778008691,11.3612705067707,-4.13035786585628));
#30205=CARTESIAN_POINT('Ctrl Pts',(48.3374778008691,11.3536536794531,-4.13035786585629));
#30206=CARTESIAN_POINT('Ctrl Pts',(48.5210265683621,11.353653679453,0.0824317919395275));
#30207=CARTESIAN_POINT('Ctrl Pts',(48.521026568362,11.3720285904897,0.0824317919387195));
#30208=CARTESIAN_POINT('Ctrl Pts',(48.5165774170445,11.3941472536996,0.0824317919386741));
#30209=CARTESIAN_POINT('Ctrl Pts',(48.5206820691924,11.4284235901226,0.0824317919383984));
#30210=CARTESIAN_POINT('Ctrl Pts',(48.5210403778953,11.4515020042572,0.0824317919369568));
#30211=CARTESIAN_POINT('Ctrl Pts',(48.5210408433891,11.4728541727075,0.0824317919368853));
#30212=CARTESIAN_POINT('Ctrl Pts',(48.5210408433891,11.4728541727075,0.0824317919368853));
#30213=CARTESIAN_POINT('Ctrl Pts',(48.5210407270154,11.467516130595,0.433477097225236));
#30214=CARTESIAN_POINT('Ctrl Pts',(48.5195832988718,11.4659265087693,0.784574340170486));
#30215=CARTESIAN_POINT('Ctrl Pts',(48.5098524785193,11.4643966328772,1.48689990372619));
#30216=CARTESIAN_POINT('Ctrl Pts',(48.5015790863104,11.4644563788109,1.83812822433663));
#30217=CARTESIAN_POINT('Ctrl Pts',(48.4743149973016,11.4603777656235,2.54074314557413));
#30218=CARTESIAN_POINT('Ctrl Pts',(48.4566988310132,11.4600103666202,2.89171006900623));
#30219=CARTESIAN_POINT('Ctrl Pts',(48.4142685323453,11.463368923483,3.59326763362947));
#30220=CARTESIAN_POINT('Ctrl Pts',(48.3894543999659,11.4670948793491,3.94385827482061));
#30221=CARTESIAN_POINT('Ctrl Pts',(48.3614264232796,11.4732422824942,4.29441317095744));
#30222=CARTESIAN_POINT('Ctrl Pts',(48.5210403778953,11.4515020042572,0.0824317919369568));
#30223=CARTESIAN_POINT('Ctrl Pts',(48.5209806868523,11.4488974993903,0.355621276395441));
#30224=CARTESIAN_POINT('Ctrl Pts',(48.519786664493,11.4477185166882,0.651206502084196));
#30225=CARTESIAN_POINT('Ctrl Pts',(48.5114206543107,11.4452664260879,1.29386039424399));
#30226=CARTESIAN_POINT('Ctrl Pts',(48.5041223947658,11.4439380177892,1.64093757516338));
#30227=CARTESIAN_POINT('Ctrl Pts',(48.4757865146344,11.4381382649983,2.39327412399031));
#30228=CARTESIAN_POINT('Ctrl Pts',(48.4570444617164,11.4370088609558,2.76883563486649));
#30229=CARTESIAN_POINT('Ctrl Pts',(48.4107714341876,11.4394032486783,3.52561349527108));
#30230=CARTESIAN_POINT('Ctrl Pts',(48.3832404595769,11.4429270404433,3.90682984479949));
#30231=CARTESIAN_POINT('Ctrl Pts',(48.3514946761257,11.4493335556629,4.29430779651743));
#30232=CARTESIAN_POINT('Ctrl Pts',(48.5206820691924,11.4284235901226,0.0824317919383984));
#30233=CARTESIAN_POINT('Ctrl Pts',(48.5207163683069,11.4285976962988,0.338435236569074));
#30234=CARTESIAN_POINT('Ctrl Pts',(48.5193523631259,11.4285879336221,0.62543968875722));
#30235=CARTESIAN_POINT('Ctrl Pts',(48.5102621676319,11.4271829834975,1.26166887657425));
#30236=CARTESIAN_POINT('Ctrl Pts',(48.5024096539482,11.4257324956491,1.61090009066305));
#30237=CARTESIAN_POINT('Ctrl Pts',(48.4732866422591,11.4203247666438,2.37176704510986));
#30238=CARTESIAN_POINT('Ctrl Pts',(48.4539681826045,11.4187667259072,2.75380781416369));
#30239=CARTESIAN_POINT('Ctrl Pts',(48.4062756535777,11.4193327724023,3.52141678779466));
#30240=CARTESIAN_POINT('Ctrl Pts',(48.3779018427096,11.4214568596339,3.90698296799157));
#30241=CARTESIAN_POINT('Ctrl Pts',(48.3455075205231,11.4261172510677,4.2945098662119));
#30242=CARTESIAN_POINT('Ctrl Pts',(48.5165774170445,11.3941472536996,0.0824317919386741));
#30243=CARTESIAN_POINT('Ctrl Pts',(48.5165547845964,11.3940705712691,0.360237634009118));
#30244=CARTESIAN_POINT('Ctrl Pts',(48.5144416806968,11.393428161435,0.666464865081089));
#30245=CARTESIAN_POINT('Ctrl Pts',(48.503189825889,11.39130385313,1.32614678064237));
#30246=CARTESIAN_POINT('Ctrl Pts',(48.4939878357291,11.389794304459,1.6796016530147));
#30247=CARTESIAN_POINT('Ctrl Pts',(48.46481028859,11.3861758639155,2.42404521997249));
#30248=CARTESIAN_POINT('Ctrl Pts',(48.4456390892509,11.3847952022384,2.80028584083416));
#30249=CARTESIAN_POINT('Ctrl Pts',(48.3983980635606,11.3835624194323,3.55118314893107));
#30250=CARTESIAN_POINT('Ctrl Pts',(48.3703287539371,11.3837102983034,3.92583579004287));
#30251=CARTESIAN_POINT('Ctrl Pts',(48.3384990828948,11.384958159128,4.29496669282085));
#30252=CARTESIAN_POINT('Ctrl Pts',(48.521026568362,11.3720285904897,0.0824317919387195));
#30253=CARTESIAN_POINT('Ctrl Pts',(48.5210265683621,11.3720285904897,0.399226071276561));
#30254=CARTESIAN_POINT('Ctrl Pts',(48.517908907227,11.3718199008203,0.733256854732802));
#30255=CARTESIAN_POINT('Ctrl Pts',(48.5037480059623,11.3711415135622,1.42281620238079));
#30256=CARTESIAN_POINT('Ctrl Pts',(48.4927046623486,11.3706718159735,1.77834069986712));
#30257=CARTESIAN_POINT('Ctrl Pts',(48.4621240605424,11.3696277842964,2.49783047371582));
#30258=CARTESIAN_POINT('Ctrl Pts',(48.4425870085971,11.369053450208,2.86179168820756));
#30259=CARTESIAN_POINT('Ctrl Pts',(48.395571861118,11.3679565169509,3.58514621754392));
#30260=CARTESIAN_POINT('Ctrl Pts',(48.3680942820317,11.3674339177823,3.94453548890209));
#30261=CARTESIAN_POINT('Ctrl Pts',(48.3374778008691,11.3670153717833,4.29522144973533));
#30262=CARTESIAN_POINT('Ctrl Pts',(48.521026568362,11.353653679453,0.0824317919395275));
#30263=CARTESIAN_POINT('Ctrl Pts',(48.521026568362,11.353653679453,0.433719204637397));
#30264=CARTESIAN_POINT('Ctrl Pts',(48.5172052126372,11.353653679453,0.785006622606423));
#30265=CARTESIAN_POINT('Ctrl Pts',(48.5019179682626,11.353653679453,1.48749857171659));
#30266=CARTESIAN_POINT('Ctrl Pts',(48.4904520792406,11.353653679453,1.83870311340066));
#30267=CARTESIAN_POINT('Ctrl Pts',(48.4598703086855,11.353653679453,2.54094611738025));
#30268=CARTESIAN_POINT('Ctrl Pts',(48.4407544264066,11.353653679453,2.89198459022065));
#30269=CARTESIAN_POINT('Ctrl Pts',(48.3948635884079,11.353653679453,3.59381163136416));
#30270=CARTESIAN_POINT('Ctrl Pts',(48.3680886315664,11.353653679453,3.94460021021523));
#30271=CARTESIAN_POINT('Ctrl Pts',(48.3374778008691,11.353653679453,4.29522144973533));
#30272=CARTESIAN_POINT('',(48.3614264232796,11.4732422824942,4.29441317095745));
#30273=CARTESIAN_POINT('Origin',(48.6500773750264,11.3534224546478,4.32103607292982));
#30274=CARTESIAN_POINT('Ctrl Pts',(48.3614264232796,11.4732422824942,4.29441317095745));
#30275=CARTESIAN_POINT('Ctrl Pts',(48.4174823766521,11.4609474762041,3.59330337868377));
#30276=CARTESIAN_POINT('Ctrl Pts',(48.4606829527973,11.4583384590298,2.89205060619289));
#30277=CARTESIAN_POINT('Ctrl Pts',(48.5152111308147,11.4664956854046,1.48682076371788));
#30278=CARTESIAN_POINT('Ctrl Pts',(48.5210406106418,11.4621780884825,0.784522402513595));
#30279=CARTESIAN_POINT('Ctrl Pts',(48.5210408433891,11.4728541727075,0.0824317919368853));
#30280=CARTESIAN_POINT('Ctrl Pts',(-48.353987706665,11.4728541727075,0.0824317919420715));
#30281=CARTESIAN_POINT('Ctrl Pts',(-48.3539875902914,11.4675161305949,-0.268613513346274));
#30282=CARTESIAN_POINT('Ctrl Pts',(-48.3525301621478,11.4659265087692,-0.619710756291519));
#30283=CARTESIAN_POINT('Ctrl Pts',(-48.3427993417953,11.4643966328771,-1.32203631984721));
#30284=CARTESIAN_POINT('Ctrl Pts',(-48.3345259495864,11.4644563788108,-1.67326464045766));
#30285=CARTESIAN_POINT('Ctrl Pts',(-48.3072618605776,11.4603777656235,-2.37587956169515));
#30286=CARTESIAN_POINT('Ctrl Pts',(-48.2896456942891,11.4600103666202,-2.72684648512726));
#30287=CARTESIAN_POINT('Ctrl Pts',(-48.2472153956212,11.463368923483,-3.42840404975053));
#30288=CARTESIAN_POINT('Ctrl Pts',(-48.2224012632418,11.4670948793491,-3.77899469094169));
#30289=CARTESIAN_POINT('Ctrl Pts',(-48.1943732865555,11.4732422824942,-4.12954958707854));
#30290=CARTESIAN_POINT('Ctrl Pts',(-48.3539872411712,11.4515020042572,0.0824317919420012));
#30291=CARTESIAN_POINT('Ctrl Pts',(-48.3539275501283,11.4488974993903,-0.19075769251648));
#30292=CARTESIAN_POINT('Ctrl Pts',(-48.352733527769,11.4477185166882,-0.486342918205233));
#30293=CARTESIAN_POINT('Ctrl Pts',(-48.3443675175867,11.4452664260878,-1.12899681036502));
#30294=CARTESIAN_POINT('Ctrl Pts',(-48.3370692580418,11.4439380177892,-1.47607399128441));
#30295=CARTESIAN_POINT('Ctrl Pts',(-48.3087333779103,11.4381382649983,-2.22841054011135));
#30296=CARTESIAN_POINT('Ctrl Pts',(-48.2899913249923,11.4370088609558,-2.60397205098753));
#30297=CARTESIAN_POINT('Ctrl Pts',(-48.2437182974635,11.4394032486783,-3.36074991139214));
#30298=CARTESIAN_POINT('Ctrl Pts',(-48.2161873228528,11.4429270404433,-3.74196626092057));
#30299=CARTESIAN_POINT('Ctrl Pts',(-48.1844415394016,11.4493335556629,-4.12944421263853));
#30300=CARTESIAN_POINT('Ctrl Pts',(-48.3536289324683,11.4284235901226,0.0824317919405622));
#30301=CARTESIAN_POINT('Ctrl Pts',(-48.3536632315829,11.4285976962988,-0.173571652690114));
#30302=CARTESIAN_POINT('Ctrl Pts',(-48.3522992264019,11.4285879336221,-0.460576104878249));
#30303=CARTESIAN_POINT('Ctrl Pts',(-48.3432090309079,11.4271829834975,-1.09680529269528));
#30304=CARTESIAN_POINT('Ctrl Pts',(-48.3353565172242,11.4257324956491,-1.4460365067841));
#30305=CARTESIAN_POINT('Ctrl Pts',(-48.3062335055351,11.4203247666438,-2.20690346123091));
#30306=CARTESIAN_POINT('Ctrl Pts',(-48.2869150458804,11.4187667259072,-2.58894423028474));
#30307=CARTESIAN_POINT('Ctrl Pts',(-48.2392225168536,11.4193327724023,-3.35655320391572));
#30308=CARTESIAN_POINT('Ctrl Pts',(-48.2108487059856,11.4214568596339,-3.74211938411265));
#30309=CARTESIAN_POINT('Ctrl Pts',(-48.178454383799,11.4261172510678,-4.129646282333));
#30310=CARTESIAN_POINT('Ctrl Pts',(-48.3495242803204,11.3941472536996,0.0824317919402862));
#30311=CARTESIAN_POINT('Ctrl Pts',(-48.3495016478723,11.3940705712692,-0.195374050130163));
#30312=CARTESIAN_POINT('Ctrl Pts',(-48.3473885439727,11.393428161435,-0.501601281202104));
#30313=CARTESIAN_POINT('Ctrl Pts',(-48.3361366891649,11.39130385313,-1.16128319676337));
#30314=CARTESIAN_POINT('Ctrl Pts',(-48.326934699005,11.3897943044591,-1.51473806913577));
#30315=CARTESIAN_POINT('Ctrl Pts',(-48.2977571518659,11.3861758639155,-2.25918163609357));
#30316=CARTESIAN_POINT('Ctrl Pts',(-48.2785859525268,11.3847952022384,-2.6354222569552));
#30317=CARTESIAN_POINT('Ctrl Pts',(-48.2313449268365,11.3835624194323,-3.38631956505211));
#30318=CARTESIAN_POINT('Ctrl Pts',(-48.203275617213,11.3837102983034,-3.76097220616396));
#30319=CARTESIAN_POINT('Ctrl Pts',(-48.1714459461707,11.384958159128,-4.13010310894195));
#30320=CARTESIAN_POINT('Ctrl Pts',(-48.3539734316379,11.3720285904897,0.08243179194024));
#30321=CARTESIAN_POINT('Ctrl Pts',(-48.353973431638,11.3720285904897,-0.234362487397608));
#30322=CARTESIAN_POINT('Ctrl Pts',(-48.350855770503,11.3718199008203,-0.56839327085381));
#30323=CARTESIAN_POINT('Ctrl Pts',(-48.3366948692382,11.3711415135622,-1.25795261850178));
#30324=CARTESIAN_POINT('Ctrl Pts',(-48.3256515256246,11.3706718159735,-1.6134771159882));
#30325=CARTESIAN_POINT('Ctrl Pts',(-48.2950709238183,11.3696277842964,-2.33296688983691));
#30326=CARTESIAN_POINT('Ctrl Pts',(-48.275533871873,11.369053450208,-2.69692810432859));
#30327=CARTESIAN_POINT('Ctrl Pts',(-48.2285187243939,11.3679565169509,-3.42028263366496));
#30328=CARTESIAN_POINT('Ctrl Pts',(-48.2010411453076,11.3674339177823,-3.77967190502318));
#30329=CARTESIAN_POINT('Ctrl Pts',(-48.170424664145,11.3670153717833,-4.13035786585643));
#30330=CARTESIAN_POINT('Ctrl Pts',(-48.3539734316379,11.3536536794531,0.0824317919394318));
#30331=CARTESIAN_POINT('Ctrl Pts',(-48.3539734316379,11.3536536794531,-0.268855620758443));
#30332=CARTESIAN_POINT('Ctrl Pts',(-48.3501520759131,11.3536536794531,-0.620143038727429));
#30333=CARTESIAN_POINT('Ctrl Pts',(-48.3348648315386,11.3536536794531,-1.32263498783758));
#30334=CARTESIAN_POINT('Ctrl Pts',(-48.3233989425165,11.3536536794531,-1.67383952952175));
#30335=CARTESIAN_POINT('Ctrl Pts',(-48.2928171719614,11.3536536794531,-2.37608253350134));
#30336=CARTESIAN_POINT('Ctrl Pts',(-48.2737012896825,11.3536536794531,-2.72712100634169));
#30337=CARTESIAN_POINT('Ctrl Pts',(-48.2278104516838,11.3536536794531,-3.42894804748519));
#30338=CARTESIAN_POINT('Ctrl Pts',(-48.2010354948423,11.3536536794531,-3.77973662633633));
#30339=CARTESIAN_POINT('Ctrl Pts',(-48.170424664145,11.3536536794531,-4.13035786585643));
#30340=CARTESIAN_POINT('',(-48.353987706665,11.4728541727075,0.0824317919420715));
#30341=CARTESIAN_POINT('Ctrl Pts',(-48.3539734316379,11.3536536794531,0.0824317919394318));
#30342=CARTESIAN_POINT('Ctrl Pts',(-48.3539734316379,11.3720285904897,0.08243179194024));
#30343=CARTESIAN_POINT('Ctrl Pts',(-48.3495242803204,11.3941472536996,0.0824317919402862));
#30344=CARTESIAN_POINT('Ctrl Pts',(-48.3536289324683,11.4284235901226,0.0824317919405622));
#30345=CARTESIAN_POINT('Ctrl Pts',(-48.3539872411712,11.4515020042572,0.0824317919420012));
#30346=CARTESIAN_POINT('Ctrl Pts',(-48.353987706665,11.4728541727075,0.0824317919420715));
#30347=CARTESIAN_POINT('',(-48.1943732865555,11.4732422824942,-4.1295495870785));
#30348=CARTESIAN_POINT('Ctrl Pts',(-48.170424664145,11.3536536794531,-4.13035786585642));
#30349=CARTESIAN_POINT('Ctrl Pts',(-48.170424664145,11.3608560447969,-4.13035786585642));
#30350=CARTESIAN_POINT('Ctrl Pts',(-48.1706799400046,11.3693343502548,-4.13028019061231));
#30351=CARTESIAN_POINT('Ctrl Pts',(-48.1714624816211,11.3788543868427,-4.13017267066916));
#30352=CARTESIAN_POINT('Ctrl Pts',(-48.1721853831276,11.3876488696476,-4.13007334517998));
#30353=CARTESIAN_POINT('Ctrl Pts',(-48.1733606260326,11.3973323098415,-4.12994875887561));
#30354=CARTESIAN_POINT('Ctrl Pts',(-48.1751937930179,11.4076804802593,-4.12983582017109));
#30355=CARTESIAN_POINT('Ctrl Pts',(-48.1769664379229,11.4176870054229,-4.12972661014235));
#30356=CARTESIAN_POINT('Ctrl Pts',(-48.1793558503801,11.428314631214,-4.12962842768296));
#30357=CARTESIAN_POINT('Ctrl Pts',(-48.1825116713384,11.4393255986458,-4.12957145846169));
#30358=CARTESIAN_POINT('Ctrl Pts',(-48.1854345364211,11.4495237602833,-4.12951869458509));
#30359=CARTESIAN_POINT('Ctrl Pts',(-48.1890152738075,11.4600498295069,-4.12950132106614));
#30360=CARTESIAN_POINT('Ctrl Pts',(-48.1933281633331,11.4706948755438,-4.12953941874883));
#30361=CARTESIAN_POINT('Ctrl Pts',(-48.193671905835,11.4715432985641,-4.12954245518013));
#30362=CARTESIAN_POINT('Ctrl Pts',(-48.1940202724543,11.4723924705143,-4.12954584164855));
#30363=CARTESIAN_POINT('Ctrl Pts',(-48.1943732865555,11.4732422824942,-4.1295495870785));
#30364=CARTESIAN_POINT('Ctrl Pts',(-48.1943732865555,11.4732422824942,-4.1295495870785));
#30365=CARTESIAN_POINT('Ctrl Pts',(-48.2504292399281,11.4609474762041,-3.42843979480483));
#30366=CARTESIAN_POINT('Ctrl Pts',(-48.2936298160732,11.4583384590298,-2.7271870223139));
#30367=CARTESIAN_POINT('Ctrl Pts',(-48.3481579940908,11.4664956854045,-1.32195717983891));
#30368=CARTESIAN_POINT('Ctrl Pts',(-48.3539874739178,11.4621780884824,-0.619658818634619));
#30369=CARTESIAN_POINT('Ctrl Pts',(-48.353987706665,11.4728541727075,0.0824317919420715));
#30370=CARTESIAN_POINT('Ctrl Pts',(-48.353987706665,11.4728541727075,0.0824317919420715));
#30371=CARTESIAN_POINT('Ctrl Pts',(-48.3539878230383,11.47819221482,-0.268613513346239));
#30372=CARTESIAN_POINT('Ctrl Pts',(-48.3525306312169,11.4874426767151,-0.619482842719547));
#30373=CARTESIAN_POINT('Ctrl Pts',(-48.3492030226972,11.5143737377389,-1.32089560268123));
#30374=CARTESIAN_POINT('Ctrl Pts',(-48.3473326059989,11.5320543368675,-1.67143903326961));
#30375=CARTESIAN_POINT('Ctrl Pts',(-48.3448536058572,11.5986492866067,-2.72261955642498));
#30376=CARTESIAN_POINT('Ctrl Pts',(-48.3401597428651,11.6392592214936,-3.42489191358813));
#30377=CARTESIAN_POINT('Ctrl Pts',(-48.3299590819566,11.6756605207398,-4.12660736491379));
#30378=CARTESIAN_POINT('Ctrl Pts',(-48.3539875902914,11.4675161305949,-0.268613513346274));
#30379=CARTESIAN_POINT('Ctrl Pts',(-48.3530459746145,11.4749860898031,-0.541629933626861));
#30380=CARTESIAN_POINT('Ctrl Pts',(-48.3513305951723,11.4844803122479,-0.832372602283611));
#30381=CARTESIAN_POINT('Ctrl Pts',(-48.3474462842888,11.5105174196336,-1.44625764301694));
#30382=CARTESIAN_POINT('Ctrl Pts',(-48.3452802018684,11.5270830007414,-1.76939839552668));
#30383=CARTESIAN_POINT('Ctrl Pts',(-48.3416407744847,11.5919036248635,-2.78284526370196));
#30384=CARTESIAN_POINT('Ctrl Pts',(-48.3361613303957,11.6298708101947,-3.46086303872938));
#30385=CARTESIAN_POINT('Ctrl Pts',(-48.3249609987341,11.6636703105734,-4.12726571477241));
#30386=CARTESIAN_POINT('Ctrl Pts',(-48.3525301621478,11.4659265087692,-0.619710756291519));
#30387=CARTESIAN_POINT('Ctrl Pts',(-48.3509583174037,11.4745419834778,-0.832717796189608));
#30388=CARTESIAN_POINT('Ctrl Pts',(-48.3489425213265,11.4840908039496,-1.07740316240887));
#30389=CARTESIAN_POINT('Ctrl Pts',(-48.3443564161318,11.5090816899176,-1.62044191410439));
#30390=CARTESIAN_POINT('Ctrl Pts',(-48.3417903805458,11.5245577996642,-1.91879287023042));
#30391=CARTESIAN_POINT('Ctrl Pts',(-48.3366078655344,11.5859418512174,-2.87982118568858));
#30392=CARTESIAN_POINT('Ctrl Pts',(-48.3302694596955,11.6209827896584,-3.52283173399625));
#30393=CARTESIAN_POINT('Ctrl Pts',(-48.3188308025814,11.6514649415801,-4.12793445419003));
#30394=CARTESIAN_POINT('Ctrl Pts',(-48.3427993417953,11.4643966328771,-1.32203631984721));
#30395=CARTESIAN_POINT('Ctrl Pts',(-48.3410826227025,11.4744825705815,-1.44781988666579));
#30396=CARTESIAN_POINT('Ctrl Pts',(-48.3390430002274,11.4843329006933,-1.62174846128019));
#30397=CARTESIAN_POINT('Ctrl Pts',(-48.3339923326216,11.5079260458424,-2.04438576000585));
#30398=CARTESIAN_POINT('Ctrl Pts',(-48.3309866294054,11.5217114161924,-2.29309144742929));
#30399=CARTESIAN_POINT('Ctrl Pts',(-48.323583058023,11.5755468354576,-3.11912189514342));
#30400=CARTESIAN_POINT('Ctrl Pts',(-48.3160467256819,11.6050189470212,-3.66842759486343));
#30401=CARTESIAN_POINT('Ctrl Pts',(-48.3054305681461,11.6282480883245,-4.12937022843424));
#30402=CARTESIAN_POINT('Ctrl Pts',(-48.3345259495864,11.4644563788108,-1.67326464045766));
#30403=CARTESIAN_POINT('Ctrl Pts',(-48.3332754508949,11.4748353413217,-1.7718391495168));
#30404=CARTESIAN_POINT('Ctrl Pts',(-48.331502851498,11.4849166217024,-1.92107075243263));
#30405=CARTESIAN_POINT('Ctrl Pts',(-48.3266822404233,11.5081462764419,-2.29415477532779));
#30406=CARTESIAN_POINT('Ctrl Pts',(-48.3236392145321,11.5213343690928,-2.51800436106519));
#30407=CARTESIAN_POINT('Ctrl Pts',(-48.3155720251447,11.5710816706553,-3.26145171754922));
#30408=CARTESIAN_POINT('Ctrl Pts',(-48.3077158623684,11.5979431249203,-3.75205476046376));
#30409=CARTESIAN_POINT('Ctrl Pts',(-48.2981605298634,11.6172366040622,-4.13013726326082));
#30410=CARTESIAN_POINT('Ctrl Pts',(-48.2936298160732,11.4583384590298,-2.7271870223139));
#30411=CARTESIAN_POINT('Ctrl Pts',(-48.2931970947244,11.4700074930205,-2.7884682930686));
#30412=CARTESIAN_POINT('Ctrl Pts',(-48.2925867090858,11.481882800679,-2.88547763875839));
#30413=CARTESIAN_POINT('Ctrl Pts',(-48.2905861997279,11.5065304546877,-3.12373338857996));
#30414=CARTESIAN_POINT('Ctrl Pts',(-48.2891989250297,11.5193254972046,-3.26497817314492));
#30415=CARTESIAN_POINT('Ctrl Pts',(-48.2851290641411,11.5598336028455,-3.71424372287552));
#30416=CARTESIAN_POINT('Ctrl Pts',(-48.2810866692801,11.5806510816358,-3.98991895788831));
#30417=CARTESIAN_POINT('Ctrl Pts',(-48.2763272274152,11.5884292819489,-4.13270208529043));
#30418=CARTESIAN_POINT('Ctrl Pts',(-48.2504292399281,11.4609474762041,-3.42843979480483));
#30419=CARTESIAN_POINT('Ctrl Pts',(-48.2516773067401,11.4731609516943,-3.46541553760594));
#30420=CARTESIAN_POINT('Ctrl Pts',(-48.2530217283576,11.4863352799677,-3.52759295216131));
#30421=CARTESIAN_POINT('Ctrl Pts',(-48.2556497470334,11.5121367174564,-3.67275508687807));
#30422=CARTESIAN_POINT('Ctrl Pts',(-48.2569333440916,11.5247638266717,-3.75573980703945));
#30423=CARTESIAN_POINT('Ctrl Pts',(-48.260312597172,11.5581209387927,-3.99151086907883));
#30424=CARTESIAN_POINT('Ctrl Pts',(-48.2619367151001,11.5743267261738,-4.13111411251207));
#30425=CARTESIAN_POINT('Ctrl Pts',(-48.2619179788887,11.5746245276893,-4.13475573974222));
#30426=CARTESIAN_POINT('Ctrl Pts',(-48.1943732865555,11.4732422824942,-4.12954958707854));
#30427=CARTESIAN_POINT('Ctrl Pts',(-48.1993391601324,11.4851966459098,-4.12960227429855));
#30428=CARTESIAN_POINT('Ctrl Pts',(-48.2060243727241,11.4974720069511,-4.12973535553844));
#30429=CARTESIAN_POINT('Ctrl Pts',(-48.2204933169654,11.5208685373805,-4.13029598569439));
#30430=CARTESIAN_POINT('Ctrl Pts',(-48.2282770486149,11.5319897067687,-4.13072353461044));
#30431=CARTESIAN_POINT('Ctrl Pts',(-48.2497657836928,11.5609276470972,-4.1326484023274));
#30432=CARTESIAN_POINT('Ctrl Pts',(-48.2616083272502,11.5743188502015,-4.13478794209711));
#30433=CARTESIAN_POINT('Ctrl Pts',(-48.2616069550931,11.5746245485739,-4.13831849503743));
#30434=CARTESIAN_POINT('Ctrl Pts',(-48.1943732865555,11.4732422824942,-4.1295495870785));
#30435=CARTESIAN_POINT('Ctrl Pts',(-48.2142367808631,11.5210597361567,-4.1297603359587));
#30436=CARTESIAN_POINT('Ctrl Pts',(-48.2616096994078,11.5740131518293,-4.13125738915642));
#30437=CARTESIAN_POINT('Ctrl Pts',(-48.2616069550931,11.5746245485739,-4.13831849503741));
#30438=CARTESIAN_POINT('',(-48.3299590485044,11.675660534618,-4.12660736370751));
#30439=CARTESIAN_POINT('Ctrl Pts',(-48.2616069550931,11.5746245485739,-4.13831849503741));
#30440=CARTESIAN_POINT('Ctrl Pts',(-48.2619179788887,11.5746245276893,-4.13475573974222));
#30441=CARTESIAN_POINT('Ctrl Pts',(-48.2763272274152,11.5884292819489,-4.13270208529043));
#30442=CARTESIAN_POINT('Ctrl Pts',(-48.3054382973461,11.6268390447666,-4.12928232258428));
#30443=CARTESIAN_POINT('Ctrl Pts',(-48.3199629155115,11.6516801004069,-4.12792406463103));
#30444=CARTESIAN_POINT('Ctrl Pts',(-48.3299590819566,11.6756605207397,-4.1266073649138));
#30445=CARTESIAN_POINT('Ctrl Pts',(-48.3299590819566,11.6756605207397,-4.1266073649138));
#30446=CARTESIAN_POINT('Ctrl Pts',(-48.3401597428651,11.6392592214936,-3.42489191358813));
#30447=CARTESIAN_POINT('Ctrl Pts',(-48.3448536058572,11.5986492866067,-2.72261955642498));
#30448=CARTESIAN_POINT('Ctrl Pts',(-48.3481589393795,11.5098560202878,-1.32104552555116));
#30449=CARTESIAN_POINT('Ctrl Pts',(-48.3539879394116,11.4835302569326,-0.619658818634546));
#30450=CARTESIAN_POINT('Ctrl Pts',(-48.353987706665,11.4728541727075,0.0824317919420715));
#30451=CARTESIAN_POINT('Ctrl Pts',(-48.353987706665,11.4728541727075,0.0824317919420715));
#30452=CARTESIAN_POINT('Ctrl Pts',(-48.3539881721588,11.4942063411577,0.082431791942142));
#30453=CARTESIAN_POINT('Ctrl Pts',(-48.3536309301586,11.5200575082527,0.0824317919434549));
#30454=CARTESIAN_POINT('Ctrl Pts',(-48.355396330448,11.5731362269333,0.0824317919411931));
#30455=CARTESIAN_POINT('Ctrl Pts',(-48.3539734316379,11.5876793312944,0.0824317919403744));
#30456=CARTESIAN_POINT('Ctrl Pts',(-48.3539734316379,11.6131136241746,0.0824317919394229));
#30457=CARTESIAN_POINT('Ctrl Pts',(-48.3539878230383,11.47819221482,-0.268613513346239));
#30458=CARTESIAN_POINT('Ctrl Pts',(-48.3539286009805,11.4971000233706,-0.190411564161195));
#30459=CARTESIAN_POINT('Ctrl Pts',(-48.3536285993105,11.5200113925673,-0.190198224429358));
#30460=CARTESIAN_POINT('Ctrl Pts',(-48.3553975542811,11.5731490589916,-0.228911446124229));
#30461=CARTESIAN_POINT('Ctrl Pts',(-48.3539734316379,11.5876793312944,-0.267838007548286));
#30462=CARTESIAN_POINT('Ctrl Pts',(-48.3539734316379,11.6131136241746,-0.267915860672084));
#30463=CARTESIAN_POINT('Ctrl Pts',(-48.3525306312169,11.4874426767151,-0.619482842719547));
#30464=CARTESIAN_POINT('Ctrl Pts',(-48.3536168471921,11.5031786713302,-0.486015179132629));
#30465=CARTESIAN_POINT('Ctrl Pts',(-48.353731882767,11.524500508176,-0.485651980041206));
#30466=CARTESIAN_POINT('Ctrl Pts',(-48.3555328010184,11.5776504745526,-0.55171778038672));
#30467=CARTESIAN_POINT('Ctrl Pts',(-48.3539734316379,11.5930695682598,-0.618146779821232));
#30468=CARTESIAN_POINT('Ctrl Pts',(-48.3539734316379,11.6169153282063,-0.61826351328359));
#30469=CARTESIAN_POINT('Ctrl Pts',(-48.3492030226972,11.5143737377389,-1.32089560268123));
#30470=CARTESIAN_POINT('Ctrl Pts',(-48.3523529181622,11.5255419633076,-1.12857563668694));
#30471=CARTESIAN_POINT('Ctrl Pts',(-48.3533876456339,11.5448479357173,-1.12801608518725));
#30472=CARTESIAN_POINT('Ctrl Pts',(-48.3554782973317,11.595969244612,-1.22311169405469));
#30473=CARTESIAN_POINT('Ctrl Pts',(-48.3539734316379,11.6126245374907,-1.31876685441994));
#30474=CARTESIAN_POINT('Ctrl Pts',(-48.3539734316379,11.632122144333,-1.31887631215363));
#30475=CARTESIAN_POINT('Ctrl Pts',(-48.3473326059989,11.5320543368675,-1.67143903326961));
#30476=CARTESIAN_POINT('Ctrl Pts',(-48.3514157821305,11.5418711528743,-1.47552932444613));
#30477=CARTESIAN_POINT('Ctrl Pts',(-48.3529551642544,11.5607507931984,-1.47492327989778));
#30478=CARTESIAN_POINT('Ctrl Pts',(-48.3552960665127,11.6098088718848,-1.57169769604833));
#30479=CARTESIAN_POINT('Ctrl Pts',(-48.353973431638,11.6267892697561,-1.6690781567457));
#30480=CARTESIAN_POINT('Ctrl Pts',(-48.353973431638,11.643527256428,-1.66914145841217));
#30481=CARTESIAN_POINT('Ctrl Pts',(-48.3448536058572,11.5986492866067,-2.72261955642498));
#30482=CARTESIAN_POINT('Ctrl Pts',(-48.3512462941311,11.612020620858,-2.6021779596111));
#30483=CARTESIAN_POINT('Ctrl Pts',(-48.353495101689,11.6290600690796,-2.60155209373665));
#30484=CARTESIAN_POINT('Ctrl Pts',(-48.3552756321719,11.6658592241822,-2.66041448169569));
#30485=CARTESIAN_POINT('Ctrl Pts',(-48.353973431638,11.6794362415567,-2.71990273552858));
#30486=CARTESIAN_POINT('Ctrl Pts',(-48.353973431638,11.689147704808,-2.71968937812887));
#30487=CARTESIAN_POINT('Ctrl Pts',(-48.3401597428651,11.6392592214936,-3.42489191358813));
#30488=CARTESIAN_POINT('Ctrl Pts',(-48.348156567804,11.6580360440914,-3.35294966330561));
#30489=CARTESIAN_POINT('Ctrl Pts',(-48.3516099899972,11.6785648284689,-3.3519488686722));
#30490=CARTESIAN_POINT('Ctrl Pts',(-48.3545184219142,11.7135824344711,-3.38562737891504));
#30491=CARTESIAN_POINT('Ctrl Pts',(-48.353973431638,11.7280712560958,-3.42030668379129));
#30492=CARTESIAN_POINT('Ctrl Pts',(-48.353973431638,11.734768153188,-3.41972463252812));
#30493=CARTESIAN_POINT('Ctrl Pts',(-48.3299590819566,11.6756605207398,-4.12660736491379));
#30494=CARTESIAN_POINT('Ctrl Pts',(-48.3399552484017,11.6996409410726,-4.12529066519656));
#30495=CARTESIAN_POINT('Ctrl Pts',(-48.3459588358221,11.7229366511894,-4.12399546447476));
#30496=CARTESIAN_POINT('Ctrl Pts',(-48.3529679274402,11.7642258753786,-4.12148173140903));
#30497=CARTESIAN_POINT('Ctrl Pts',(-48.3539734316379,11.7822193894509,-4.1202631990651));
#30498=CARTESIAN_POINT('Ctrl Pts',(-48.3539734316379,11.7955954176946,-4.1190998361036));
#30499=CARTESIAN_POINT('Ctrl Pts',(-48.3299589815999,11.6756605623745,-4.12660736129494));
#30500=CARTESIAN_POINT('Ctrl Pts',(-48.334075322032,11.685535483409,-4.12606515642765));
#30501=CARTESIAN_POINT('Ctrl Pts',(-48.3375652097276,11.6953464500616,-4.12552210528721));
#30502=CARTESIAN_POINT('Ctrl Pts',(-48.3404730684758,11.704904887613,-4.12498379119384));
#30503=CARTESIAN_POINT('Ctrl Pts',(-48.3435583735783,11.7150466099945,-4.12441262754291));
#30504=CARTESIAN_POINT('Ctrl Pts',(-48.3459891527135,11.7249027978758,-4.12384690527284));
#30505=CARTESIAN_POINT('Ctrl Pts',(-48.3478717153206,11.7342762879822,-4.12329089420766));
#30506=CARTESIAN_POINT('Ctrl Pts',(-48.3498402999992,11.7440780916192,-4.12270947669732));
#30507=CARTESIAN_POINT('Ctrl Pts',(-48.3512109703853,11.7533514160688,-4.12213873671569));
#30508=CARTESIAN_POINT('Ctrl Pts',(-48.3521436788015,11.7619163369653,-4.12157963240757));
#30509=CARTESIAN_POINT('Ctrl Pts',(-48.3531576213552,11.7712272187115,-4.12097183297083));
#30510=CARTESIAN_POINT('Ctrl Pts',(-48.3536562142594,11.7797008569823,-4.12037779232948));
#30511=CARTESIAN_POINT('Ctrl Pts',(-48.3538589494056,11.7871660424472,-4.11979354428953));
#30512=CARTESIAN_POINT('Ctrl Pts',(-48.3539396582106,11.7901379306941,-4.11956095530813));
#30513=CARTESIAN_POINT('Ctrl Pts',(-48.3539734295675,11.7929506159593,-4.1193298643544));
#30514=CARTESIAN_POINT('Ctrl Pts',(-48.3539734316378,11.7955954176947,-4.11909983610361));
#30515=CARTESIAN_POINT('Ctrl Pts',(-48.3539734316379,11.6131136241746,0.0824317919394229));
#30516=CARTESIAN_POINT('Ctrl Pts',(-48.3539734316379,11.5876793312944,0.0824317919403744));
#30517=CARTESIAN_POINT('Ctrl Pts',(-48.355396330448,11.5731362269333,0.0824317919411931));
#30518=CARTESIAN_POINT('Ctrl Pts',(-48.3536309301586,11.5200575082527,0.0824317919434549));
#30519=CARTESIAN_POINT('Ctrl Pts',(-48.3539881721588,11.4942063411577,0.082431791942142));
#30520=CARTESIAN_POINT('Ctrl Pts',(-48.353987706665,11.4728541727075,0.0824317919420715));
#30521=CARTESIAN_POINT('Ctrl Pts',(-48.353987706665,11.4728541727075,0.0824317919420715));
#30522=CARTESIAN_POINT('Ctrl Pts',(-48.3539878230386,11.47819221482,0.433477097230417));
#30523=CARTESIAN_POINT('Ctrl Pts',(-48.3525306312176,11.4874426767153,0.784346426604709));
#30524=CARTESIAN_POINT('Ctrl Pts',(-48.3492030226983,11.5143737377395,1.48575918657027));
#30525=CARTESIAN_POINT('Ctrl Pts',(-48.3473326060001,11.5320543368686,1.83630261716154));
#30526=CARTESIAN_POINT('Ctrl Pts',(-48.3448536058578,11.5986492866091,2.88748314032846));
#30527=CARTESIAN_POINT('Ctrl Pts',(-48.3401597428655,11.6392592214975,3.58975549751167));
#30528=CARTESIAN_POINT('Ctrl Pts',(-48.3299590819566,11.6756605207451,4.29147094885445));
#30529=CARTESIAN_POINT('Ctrl Pts',(-48.3539881721588,11.4942063411577,0.082431791942142));
#30530=CARTESIAN_POINT('Ctrl Pts',(-48.3539286009808,11.4971000233708,0.355275148045688));
#30531=CARTESIAN_POINT('Ctrl Pts',(-48.3536168471926,11.5031786713304,0.650878763018348));
#30532=CARTESIAN_POINT('Ctrl Pts',(-48.352352918163,11.5255419633083,1.2934392205762));
#30533=CARTESIAN_POINT('Ctrl Pts',(-48.3514157821314,11.5418711528752,1.64039290833772));
#30534=CARTESIAN_POINT('Ctrl Pts',(-48.3512462941313,11.6120206208596,2.76704154350989));
#30535=CARTESIAN_POINT('Ctrl Pts',(-48.348156567804,11.6580360440938,3.51781324721676));
#30536=CARTESIAN_POINT('Ctrl Pts',(-48.3399552484018,11.6996409410751,4.29015424910472));
#30537=CARTESIAN_POINT('Ctrl Pts',(-48.3536309301586,11.5200575082527,0.0824317919434549));
#30538=CARTESIAN_POINT('Ctrl Pts',(-48.3536285993108,11.5200113925675,0.355061808316268));
#30539=CARTESIAN_POINT('Ctrl Pts',(-48.3537318827671,11.5245005081763,0.650515563928747));
#30540=CARTESIAN_POINT('Ctrl Pts',(-48.3533876456339,11.5448479357178,1.29287966907655));
#30541=CARTESIAN_POINT('Ctrl Pts',(-48.352955164254,11.5607507931992,1.63978686378821));
#30542=CARTESIAN_POINT('Ctrl Pts',(-48.3534951016876,11.6290600690807,2.76641567763006));
#30543=CARTESIAN_POINT('Ctrl Pts',(-48.3516099899957,11.6785648284704,3.51681245257216));
#30544=CARTESIAN_POINT('Ctrl Pts',(-48.3459588358221,11.7229366511906,4.28885904836748));
#30545=CARTESIAN_POINT('Ctrl Pts',(-48.355396330448,11.5731362269333,0.0824317919411931));
#30546=CARTESIAN_POINT('Ctrl Pts',(-48.3553975542812,11.5731490589917,0.393775030006615));
#30547=CARTESIAN_POINT('Ctrl Pts',(-48.355532801018,11.5776504745527,0.716581364269289));
#30548=CARTESIAN_POINT('Ctrl Pts',(-48.35547829733,11.5959692446123,1.38797527793762));
#30549=CARTESIAN_POINT('Ctrl Pts',(-48.3552960665103,11.6098088718852,1.73656127993144));
#30550=CARTESIAN_POINT('Ctrl Pts',(-48.3552756321677,11.6658592241826,2.82527806557877));
#30551=CARTESIAN_POINT('Ctrl Pts',(-48.35451842191,11.7135824344715,3.55049096279885));
#30552=CARTESIAN_POINT('Ctrl Pts',(-48.3529679274402,11.7642258753785,4.28634531528709));
#30553=CARTESIAN_POINT('Ctrl Pts',(-48.3539734316379,11.5876793312944,0.0824317919403744));
#30554=CARTESIAN_POINT('Ctrl Pts',(-48.3539734316379,11.5876793312944,0.432701591429034));
#30555=CARTESIAN_POINT('Ctrl Pts',(-48.3539734316373,11.5930695682598,0.783010363701859));
#30556=CARTESIAN_POINT('Ctrl Pts',(-48.3539734316356,11.6126245374908,1.48363043830021));
#30557=CARTESIAN_POINT('Ctrl Pts',(-48.3539734316346,11.6267892697563,1.83394174062573));
#30558=CARTESIAN_POINT('Ctrl Pts',(-48.3539734316326,11.6794362415569,2.88476631940789));
#30559=CARTESIAN_POINT('Ctrl Pts',(-48.3539734316326,11.728071256096,3.58517026767012));
#30560=CARTESIAN_POINT('Ctrl Pts',(-48.3539734316379,11.7822193894509,4.28512678294395));
#30561=CARTESIAN_POINT('Ctrl Pts',(-48.3539734316379,11.6131136241746,0.0824317919394229));
#30562=CARTESIAN_POINT('Ctrl Pts',(-48.3539734316379,11.6131136241746,0.432779444550929));
#30563=CARTESIAN_POINT('Ctrl Pts',(-48.3539734316373,11.6169153282063,0.783127097162436));
#30564=CARTESIAN_POINT('Ctrl Pts',(-48.3539734316357,11.632122144333,1.48373989603248));
#30565=CARTESIAN_POINT('Ctrl Pts',(-48.3539734316348,11.643527256428,1.83400504229102));
#30566=CARTESIAN_POINT('Ctrl Pts',(-48.3539734316329,11.689147704808,2.88455296200771));
#30567=CARTESIAN_POINT('Ctrl Pts',(-48.3539734316329,11.734768153188,3.58458821640696));
#30568=CARTESIAN_POINT('Ctrl Pts',(-48.3539734316379,11.7955954176946,4.28396341998245));
#30569=CARTESIAN_POINT('',(-48.3299590484456,11.6756605346478,4.29147094764604));
#30570=CARTESIAN_POINT('Ctrl Pts',(-48.3539734316379,11.7955954176946,4.28396341998245));
#30571=CARTESIAN_POINT('Ctrl Pts',(-48.3539734263918,11.7889074035727,4.2845451014632));
#30572=CARTESIAN_POINT('Ctrl Pts',(-48.3537589209384,11.781142600467,4.28513386273919));
#30573=CARTESIAN_POINT('Ctrl Pts',(-48.3531105335782,11.7724551591809,4.28573553812961));
#30574=CARTESIAN_POINT('Ctrl Pts',(-48.3525182830083,11.7645198686933,4.28628512100966));
#30575=CARTESIAN_POINT('Ctrl Pts',(-48.3515621295827,11.7558145072651,4.28684550102065));
#30576=CARTESIAN_POINT('Ctrl Pts',(-48.3500742568563,11.7464987405109,4.2874174568295));
#30577=CARTESIAN_POINT('Ctrl Pts',(-48.348658585424,11.7376350355516,4.28796165761009));
#30578=CARTESIAN_POINT('Ctrl Pts',(-48.3467601168661,11.7282190174495,4.28851631181798));
#30579=CARTESIAN_POINT('Ctrl Pts',(-48.3442567970522,11.7184280696924,4.28907864596114));
#30580=CARTESIAN_POINT('Ctrl Pts',(-48.3418724781032,11.7091025563739,4.28961424830237));
#30581=CARTESIAN_POINT('Ctrl Pts',(-48.3389385395999,11.6994377386549,4.2901567453683));
#30582=CARTESIAN_POINT('Ctrl Pts',(-48.3353869859874,11.6896156896676,4.29070126749766));
#30583=CARTESIAN_POINT('Ctrl Pts',(-48.3337149896359,11.6849916766686,4.29095761700351));
#30584=CARTESIAN_POINT('Ctrl Pts',(-48.3319067473016,11.6803331677637,4.29121438526338));
#30585=CARTESIAN_POINT('Ctrl Pts',(-48.3299589814234,11.6756605624531,4.29147094522923));
#30586=CARTESIAN_POINT('Ctrl Pts',(-48.3299590819566,11.6756605207451,4.29147094885445));
#30587=CARTESIAN_POINT('Ctrl Pts',(-48.3401597428655,11.6392592214975,3.58975549751167));
#30588=CARTESIAN_POINT('Ctrl Pts',(-48.3448536058578,11.5986492866091,2.88748314032846));
#30589=CARTESIAN_POINT('Ctrl Pts',(-48.3481589393809,11.5098560202884,1.48590910943924));
#30590=CARTESIAN_POINT('Ctrl Pts',(-48.3539879394121,11.4835302569326,0.784522402518766));
#30591=CARTESIAN_POINT('Ctrl Pts',(-48.353987706665,11.4728541727075,0.0824317919420715));
#30592=CARTESIAN_POINT('Ctrl Pts',(-48.353987706665,11.4728541727075,0.0824317919420715));
#30593=CARTESIAN_POINT('Ctrl Pts',(-48.3539875902917,11.4675161305949,0.433477097230381));
#30594=CARTESIAN_POINT('Ctrl Pts',(-48.3525301621484,11.4659265087691,0.784574340176142));
#30595=CARTESIAN_POINT('Ctrl Pts',(-48.3427993417961,11.4643966328771,1.48689990373394));
#30596=CARTESIAN_POINT('Ctrl Pts',(-48.334525949587,11.4644563788108,1.83812822434599));
#30597=CARTESIAN_POINT('Ctrl Pts',(-48.2936298160723,11.4583384590299,2.89205060620861));
#30598=CARTESIAN_POINT('Ctrl Pts',(-48.2504292399278,11.4609474762042,3.59330337868711));
#30599=CARTESIAN_POINT('Ctrl Pts',(-48.1943732865555,11.4732422824942,4.29441317095732));
#30600=CARTESIAN_POINT('Ctrl Pts',(-48.3539878230386,11.47819221482,0.433477097230417));
#30601=CARTESIAN_POINT('Ctrl Pts',(-48.3530459746151,11.4749860898031,0.706493517511539));
#30602=CARTESIAN_POINT('Ctrl Pts',(-48.3509583174044,11.4745419834778,0.997581380074998));
#30603=CARTESIAN_POINT('Ctrl Pts',(-48.3410826227033,11.4744825705815,1.61268347055339));
#30604=CARTESIAN_POINT('Ctrl Pts',(-48.3332754508955,11.4748353413218,1.93670273340589));
#30605=CARTESIAN_POINT('Ctrl Pts',(-48.2931970947235,11.4700074930207,2.95333187696386));
#30606=CARTESIAN_POINT('Ctrl Pts',(-48.2516773067399,11.4731609516944,3.63027912148841));
#30607=CARTESIAN_POINT('Ctrl Pts',(-48.1993391601324,11.4851966459098,4.29446585817733));
#30608=CARTESIAN_POINT('Ctrl Pts',(-48.3525306312176,11.4874426767153,0.784346426604709));
#30609=CARTESIAN_POINT('Ctrl Pts',(-48.3513305951732,11.484480312248,0.997236186169142));
#30610=CARTESIAN_POINT('Ctrl Pts',(-48.3489425213275,11.4840908039499,1.24226674629595));
#30611=CARTESIAN_POINT('Ctrl Pts',(-48.3390430002284,11.4843329006938,1.78661204517143));
#30612=CARTESIAN_POINT('Ctrl Pts',(-48.3315028514989,11.484916621703,2.08593433632647));
#30613=CARTESIAN_POINT('Ctrl Pts',(-48.292586709085,11.4818828006799,3.05034122265968));
#30614=CARTESIAN_POINT('Ctrl Pts',(-48.2530217283574,11.4863352799679,3.69245653604367));
#30615=CARTESIAN_POINT('Ctrl Pts',(-48.2060243727241,11.4974720069511,4.29459893941723));
#30616=CARTESIAN_POINT('Ctrl Pts',(-48.3492030226983,11.5143737377395,1.48575918657027));
#30617=CARTESIAN_POINT('Ctrl Pts',(-48.34744628429,11.5105174196344,1.61112122690618));
#30618=CARTESIAN_POINT('Ctrl Pts',(-48.3443564161332,11.5090816899187,1.78530549799782));
#30619=CARTESIAN_POINT('Ctrl Pts',(-48.3339923326229,11.5079260458442,2.2092493439093));
#30620=CARTESIAN_POINT('Ctrl Pts',(-48.3266822404244,11.5081462764441,2.45901835923708));
#30621=CARTESIAN_POINT('Ctrl Pts',(-48.2905861997275,11.5065304546904,3.28859697249979));
#30622=CARTESIAN_POINT('Ctrl Pts',(-48.2556497470331,11.5121367174566,3.83761867075986));
#30623=CARTESIAN_POINT('Ctrl Pts',(-48.2204933169654,11.5208685373805,4.29515956957318));
#30624=CARTESIAN_POINT('Ctrl Pts',(-48.3473326060001,11.5320543368686,1.83630261716154));
#30625=CARTESIAN_POINT('Ctrl Pts',(-48.3452802018698,11.5270830007426,1.93426197941878));
#30626=CARTESIAN_POINT('Ctrl Pts',(-48.3417903805473,11.5245577996659,2.08365645412851));
#30627=CARTESIAN_POINT('Ctrl Pts',(-48.3309866294069,11.5217114161952,2.45795503134133));
#30628=CARTESIAN_POINT('Ctrl Pts',(-48.3236392145334,11.5213343690961,2.68286794498518));
#30629=CARTESIAN_POINT('Ctrl Pts',(-48.2891989250295,11.5193254972085,3.42984175707725));
#30630=CARTESIAN_POINT('Ctrl Pts',(-48.2569333440914,11.5247638266718,3.9206033909208));
#30631=CARTESIAN_POINT('Ctrl Pts',(-48.2282770486149,11.5319897067687,4.29558711848924));
#30632=CARTESIAN_POINT('Ctrl Pts',(-48.3448536058578,11.5986492866091,2.88748314032846));
#30633=CARTESIAN_POINT('Ctrl Pts',(-48.3416407744856,11.5919036248663,2.94770884760779));
#30634=CARTESIAN_POINT('Ctrl Pts',(-48.3366078655353,11.5859418512212,3.04468476960679));
#30635=CARTESIAN_POINT('Ctrl Pts',(-48.3235830580242,11.5755468354636,3.28398547908769));
#30636=CARTESIAN_POINT('Ctrl Pts',(-48.3155720251457,11.5710816706623,3.42631530150717));
#30637=CARTESIAN_POINT('Ctrl Pts',(-48.2851290641413,11.5598336028535,3.87910730684837));
#30638=CARTESIAN_POINT('Ctrl Pts',(-48.260312597172,11.5581209387927,4.15637445295875));
#30639=CARTESIAN_POINT('Ctrl Pts',(-48.2497657836928,11.5609276470972,4.29751198620621));
#30640=CARTESIAN_POINT('Ctrl Pts',(-48.3401597428655,11.6392592214975,3.58975549751167));
#30641=CARTESIAN_POINT('Ctrl Pts',(-48.3361613303963,11.6298708101994,3.62572662265912));
#30642=CARTESIAN_POINT('Ctrl Pts',(-48.3302694596963,11.6209827896646,3.68769531794308));
#30643=CARTESIAN_POINT('Ctrl Pts',(-48.3160467256828,11.6050189470302,3.83329117884303));
#30644=CARTESIAN_POINT('Ctrl Pts',(-48.3077158623693,11.5979431249306,3.91691834445902));
#30645=CARTESIAN_POINT('Ctrl Pts',(-48.2810866692805,11.5806510816468,4.15478254189364));
#30646=CARTESIAN_POINT('Ctrl Pts',(-48.2619367151001,11.5743267261738,4.29597769639093));
#30647=CARTESIAN_POINT('Ctrl Pts',(-48.2616083272502,11.5743188502015,4.29965152597593));
#30648=CARTESIAN_POINT('Ctrl Pts',(-48.3299590819566,11.6756605207451,4.29147094885445));
#30649=CARTESIAN_POINT('Ctrl Pts',(-48.3249609987341,11.6636703105801,4.29212929872931));
#30650=CARTESIAN_POINT('Ctrl Pts',(-48.3188308025814,11.6514649415887,4.29279803816797));
#30651=CARTESIAN_POINT('Ctrl Pts',(-48.3054305681461,11.6282480883359,4.29423381244547));
#30652=CARTESIAN_POINT('Ctrl Pts',(-48.2981605298634,11.6172366040747,4.29500084728431));
#30653=CARTESIAN_POINT('Ctrl Pts',(-48.2763272274152,11.588429281961,4.29756566931001));
#30654=CARTESIAN_POINT('Ctrl Pts',(-48.2619179788887,11.5746245276893,4.29961932362103));
#30655=CARTESIAN_POINT('Ctrl Pts',(-48.2616069550931,11.5746245485739,4.30318207891624));
#30656=CARTESIAN_POINT('Ctrl Pts',(-48.3299590819566,11.6756605207451,4.29147094885445));
#30657=CARTESIAN_POINT('Ctrl Pts',(-48.3199629155115,11.6516801004151,4.29278764860417));
#30658=CARTESIAN_POINT('Ctrl Pts',(-48.3054382973461,11.6268390447792,4.29414590660908));
#30659=CARTESIAN_POINT('Ctrl Pts',(-48.2763272274152,11.588429281961,4.29756566931001));
#30660=CARTESIAN_POINT('Ctrl Pts',(-48.2619179788887,11.5746245276893,4.29961932362103));
#30661=CARTESIAN_POINT('Ctrl Pts',(-48.2616069550931,11.5746245485739,4.30318207891625));
#30662=CARTESIAN_POINT('',(-48.1943732865555,11.4732422824942,4.29441317095733));
#30663=CARTESIAN_POINT('Ctrl Pts',(-48.1943732865555,11.4732422824942,4.29441317095732));
#30664=CARTESIAN_POINT('Ctrl Pts',(-48.196487864659,11.4783327131562,4.29443560633351));
#30665=CARTESIAN_POINT('Ctrl Pts',(-48.1988424763931,11.4833192247691,4.29447185544362));
#30666=CARTESIAN_POINT('Ctrl Pts',(-48.2013545801683,11.4882155712552,4.2945249560433));
#30667=CARTESIAN_POINT('Ctrl Pts',(-48.204468050974,11.4942840434216,4.29459076827944));
#30668=CARTESIAN_POINT('Ctrl Pts',(-48.2078249701059,11.5002159027501,4.29468221538989));
#30669=CARTESIAN_POINT('Ctrl Pts',(-48.2113461926006,11.5060421521798,4.29480804329398));
#30670=CARTESIAN_POINT('Ctrl Pts',(-48.2119784181535,11.5070882388083,4.29483063533874));
#30671=CARTESIAN_POINT('Ctrl Pts',(-48.2126160717519,11.5081308970756,4.29485434887851));
#30672=CARTESIAN_POINT('Ctrl Pts',(-48.2132588448447,11.5091702721658,4.29487925449521));
#30673=CARTESIAN_POINT('Ctrl Pts',(-48.2172981689735,11.5157019284025,4.29503576673815));
#30674=CARTESIAN_POINT('Ctrl Pts',(-48.2215368905597,11.5221052410797,4.29523764753415));
#30675=CARTESIAN_POINT('Ctrl Pts',(-48.2259211554775,11.5284062451254,4.29551276580963));
#30676=CARTESIAN_POINT('Ctrl Pts',(-48.2290245093856,11.5328663418341,4.29570750526799));
#30677=CARTESIAN_POINT('Ctrl Pts',(-48.2322009933063,11.5372739115821,4.29593860844117));
#30678=CARTESIAN_POINT('Ctrl Pts',(-48.2354399603075,11.5416356868782,4.29622874106156));
#30679=CARTESIAN_POINT('Ctrl Pts',(-48.2381803964523,11.5453261124591,4.29647421744937));
#30680=CARTESIAN_POINT('Ctrl Pts',(-48.2409650173885,11.5489827466928,4.29676073668963));
#30681=CARTESIAN_POINT('Ctrl Pts',(-48.2437875269064,11.5526057362471,4.29712165145316));
#30682=CARTESIAN_POINT('Ctrl Pts',(-48.2458021197089,11.5551916792292,4.29737925777134));
#30683=CARTESIAN_POINT('Ctrl Pts',(-48.2478368856971,11.5577614675671,4.29767390515738));
#30684=CARTESIAN_POINT('Ctrl Pts',(-48.2498887314464,11.5603135612093,4.29803922268809));
#30685=CARTESIAN_POINT('Ctrl Pts',(-48.2513195940382,11.5620932736095,4.29829397828509));
#30686=CARTESIAN_POINT('Ctrl Pts',(-48.2527589064005,11.5638644687507,4.29858198823371));
#30687=CARTESIAN_POINT('Ctrl Pts',(-48.254204885756,11.5656264211453,4.29893754450221));
#30688=CARTESIAN_POINT('Ctrl Pts',(-48.2551766147946,11.5668104908209,4.29917648591561));
#30689=CARTESIAN_POINT('Ctrl Pts',(-48.256151771226,11.5679907811658,4.29944485081465));
#30690=CARTESIAN_POINT('Ctrl Pts',(-48.257126565722,11.5691644697714,4.29977599704979));
#30691=CARTESIAN_POINT('Ctrl Pts',(-48.2577142195889,11.5698720267494,4.29997562821966));
#30692=CARTESIAN_POINT('Ctrl Pts',(-48.2583022378277,11.5705777201803,4.30019764216591));
#30693=CARTESIAN_POINT('Ctrl Pts',(-48.2588872441424,11.5712791301838,4.30046624970369));
#30694=CARTESIAN_POINT('Ctrl Pts',(-48.2592662088748,11.5717335007565,4.30064025258387));
#30695=CARTESIAN_POINT('Ctrl Pts',(-48.2596450908386,11.572187424288,4.30083381477504));
#30696=CARTESIAN_POINT('Ctrl Pts',(-48.2600166453457,11.5726339419601,4.30106614290028));
#30697=CARTESIAN_POINT('Ctrl Pts',(-48.2602186580187,11.5728767118007,4.30119245875618));
#30698=CARTESIAN_POINT('Ctrl Pts',(-48.2604197722893,11.5731188229199,4.3013312052759));
#30699=CARTESIAN_POINT('Ctrl Pts',(-48.2606142273849,11.5733542339528,4.30148923677993));
#30700=CARTESIAN_POINT('Ctrl Pts',(-48.2607720584956,11.5735453072939,4.30161750437682));
#30701=CARTESIAN_POINT('Ctrl Pts',(-48.2609257038798,11.5737321635395,4.30175813254586));
#30702=CARTESIAN_POINT('Ctrl Pts',(-48.2610695236536,11.5739092744934,4.30192109628311));
#30703=CARTESIAN_POINT('Ctrl Pts',(-48.2611414335404,11.5739978299704,4.30200257815174));
#30704=CARTESIAN_POINT('Ctrl Pts',(-48.2612094962467,11.5740821529245,4.30208695578815));
#30705=CARTESIAN_POINT('Ctrl Pts',(-48.261281040375,11.5741721054102,4.30219266734828));
#30706=CARTESIAN_POINT('Ctrl Pts',(-48.2613168124392,11.5742170816531,4.30224552312834));
#30707=CARTESIAN_POINT('Ctrl Pts',(-48.2613523347546,11.5742618826269,4.30229992241309));
#30708=CARTESIAN_POINT('Ctrl Pts',(-48.2614004758006,11.5743239422312,4.30239026429631));
#30709=CARTESIAN_POINT('Ctrl Pts',(-48.2614245463109,11.574354972017,4.30243543521408));
#30710=CARTESIAN_POINT('Ctrl Pts',(-48.2614593265161,11.5743996848319,4.30249945951758));
#30711=CARTESIAN_POINT('Ctrl Pts',(-48.2615035948095,11.5744597225481,4.30261831732649));
#30712=CARTESIAN_POINT('Ctrl Pts',(-48.2615361811056,11.5745039168608,4.30270580964811));
#30713=CARTESIAN_POINT('Ctrl Pts',(-48.2615743374215,11.5745568559738,4.30282296938909));
#30714=CARTESIAN_POINT('Ctrl Pts',(-48.2615948384317,11.5745940265263,4.30298682659291));
#30715=CARTESIAN_POINT('Ctrl Pts',(-48.2616021879244,11.5746073519527,4.30304556844533));
#30716=CARTESIAN_POINT('Ctrl Pts',(-48.2616069829336,11.5746183373345,4.30311034495461));
#30717=CARTESIAN_POINT('Ctrl Pts',(-48.2616069550935,11.5746245484993,4.30318207805534));
#30718=CARTESIAN_POINT('Ctrl Pts',(-48.1943732865555,11.4732422824942,4.29441317095733));
#30719=CARTESIAN_POINT('Ctrl Pts',(-48.2504292399278,11.4609474762042,3.59330337868711));
#30720=CARTESIAN_POINT('Ctrl Pts',(-48.2936298160723,11.4583384590299,2.89205060620861));
#30721=CARTESIAN_POINT('Ctrl Pts',(-48.3481579940919,11.4664956854044,1.48682076372511));
#30722=CARTESIAN_POINT('Ctrl Pts',(-48.3539874739184,11.4621780884823,0.78452240251869));
#30723=CARTESIAN_POINT('Ctrl Pts',(-48.353987706665,11.4728541727075,0.0824317919420715));
#30724=CARTESIAN_POINT('Ctrl Pts',(0.0835265683594526,11.4728541727075,
-48.3550824830876));
#30725=CARTESIAN_POINT('Ctrl Pts',(0.0835265683593817,11.4942063411577,
-48.3550829485814));
#30726=CARTESIAN_POINT('Ctrl Pts',(0.0835265683580835,11.5200575082527,
-48.3547257065812));
#30727=CARTESIAN_POINT('Ctrl Pts',(0.0835265683603323,11.5731362269333,
-48.3564911068706));
#30728=CARTESIAN_POINT('Ctrl Pts',(0.0835265683611482,11.5876793312944,
-48.3550682080606));
#30729=CARTESIAN_POINT('Ctrl Pts',(0.0835265683620996,11.6131136241746,
-48.3550682080606));
#30730=CARTESIAN_POINT('Ctrl Pts',(0.434571873647755,11.4781922148201,-48.3550825994612));
#30731=CARTESIAN_POINT('Ctrl Pts',(0.356369924462715,11.4971000233707,-48.3550233774034));
#30732=CARTESIAN_POINT('Ctrl Pts',(0.356156584730894,11.5200113925674,-48.3547233757333));
#30733=CARTESIAN_POINT('Ctrl Pts',(0.394869806425756,11.5731490589917,-48.3564923307038));
#30734=CARTESIAN_POINT('Ctrl Pts',(0.433796367849811,11.5876793312944,-48.3550682080606));
#30735=CARTESIAN_POINT('Ctrl Pts',(0.433874220973609,11.6131136241746,-48.3550682080606));
#30736=CARTESIAN_POINT('Ctrl Pts',(0.785441203021056,11.4874426767152,-48.3536254076401));
#30737=CARTESIAN_POINT('Ctrl Pts',(0.651973539434153,11.5031786713302,-48.3547116236151));
#30738=CARTESIAN_POINT('Ctrl Pts',(0.651610340342747,11.5245005081761,-48.3548266591899));
#30739=CARTESIAN_POINT('Ctrl Pts',(0.717676140688252,11.5776504745526,-48.3566275774411));
#30740=CARTESIAN_POINT('Ctrl Pts',(0.78410514012276,11.5930695682598,-48.3550682080606));
#30741=CARTESIAN_POINT('Ctrl Pts',(0.784221873585119,11.6169153282063,-48.3550682080606));
#30742=CARTESIAN_POINT('Ctrl Pts',(1.48685396298274,11.5143737377389,-48.3502977991207));
#30743=CARTESIAN_POINT('Ctrl Pts',(1.29453399698848,11.5255419633077,-48.3534476945855));
#30744=CARTESIAN_POINT('Ctrl Pts',(1.29397444548881,11.5448479357173,-48.354482422057));
#30745=CARTESIAN_POINT('Ctrl Pts',(1.38907005435624,11.5959692446121,-48.3565730737545));
#30746=CARTESIAN_POINT('Ctrl Pts',(1.48472521472147,11.6126245374907,-48.3550682080606));
#30747=CARTESIAN_POINT('Ctrl Pts',(1.48483467245517,11.632122144333,-48.3550682080606));
#30748=CARTESIAN_POINT('Ctrl Pts',(1.83739739357112,11.5320543368675,-48.3484273824224));
#30749=CARTESIAN_POINT('Ctrl Pts',(1.64148768474769,11.5418711528743,-48.3525105585539));
#30750=CARTESIAN_POINT('Ctrl Pts',(1.64088164019935,11.5607507931985,-48.3540499406775));
#30751=CARTESIAN_POINT('Ctrl Pts',(1.73765605634988,11.6098088718849,-48.3563908429355));
#30752=CARTESIAN_POINT('Ctrl Pts',(1.83503651704724,11.6267892697561,-48.3550682080606));
#30753=CARTESIAN_POINT('Ctrl Pts',(1.83509981871371,11.643527256428,-48.3550682080606));
#30754=CARTESIAN_POINT('Ctrl Pts',(2.88857791672651,11.5986492866067,-48.3459483822799));
#30755=CARTESIAN_POINT('Ctrl Pts',(2.7681363199127,11.612020620858,-48.3523410705538));
#30756=CARTESIAN_POINT('Ctrl Pts',(2.76751045403826,11.6290600690796,-48.3545898781116));
#30757=CARTESIAN_POINT('Ctrl Pts',(2.82637284199726,11.6658592241822,-48.3563704085945));
#30758=CARTESIAN_POINT('Ctrl Pts',(2.88586109583013,11.6794362415567,-48.3550682080606));
#30759=CARTESIAN_POINT('Ctrl Pts',(2.88564773843041,11.689147704808,-48.3550682080606));
#30760=CARTESIAN_POINT('Ctrl Pts',(3.59085027388967,11.6392592214936,-48.3412545192878));
#30761=CARTESIAN_POINT('Ctrl Pts',(3.51890802360723,11.6580360440914,-48.3492513442266));
#30762=CARTESIAN_POINT('Ctrl Pts',(3.51790722897382,11.6785648284689,-48.3527047664198));
#30763=CARTESIAN_POINT('Ctrl Pts',(3.55158573921662,11.7135824344711,-48.3556131983368));
#30764=CARTESIAN_POINT('Ctrl Pts',(3.58626504409284,11.7280712560958,-48.3550682080606));
#30765=CARTESIAN_POINT('Ctrl Pts',(3.58568299282967,11.734768153188,-48.3550682080606));
#30766=CARTESIAN_POINT('Ctrl Pts',(4.29256572521535,11.6756605207398,-48.3310538583792));
#30767=CARTESIAN_POINT('Ctrl Pts',(4.29124902549811,11.6996409410726,-48.3410500248244));
#30768=CARTESIAN_POINT('Ctrl Pts',(4.28995382477632,11.7229366511894,-48.3470536122447));
#30769=CARTESIAN_POINT('Ctrl Pts',(4.28744009171059,11.7642258753786,-48.3540627038628));
#30770=CARTESIAN_POINT('Ctrl Pts',(4.28622155936666,11.7822193894509,-48.3550682080606));
#30771=CARTESIAN_POINT('Ctrl Pts',(4.28505819640515,11.7955954176946,-48.3550682080606));
#30772=CARTESIAN_POINT('',(4.29256572400907,11.675660534618,-48.3310538249271));
#30773=CARTESIAN_POINT('',(0.0835265683594526,11.4728541727075,-48.3550824830876));
#30774=CARTESIAN_POINT('Ctrl Pts',(4.29256572521535,11.6756605207397,-48.3310538583792));
#30775=CARTESIAN_POINT('Ctrl Pts',(3.59085027388967,11.6392592214936,-48.3412545192878));
#30776=CARTESIAN_POINT('Ctrl Pts',(2.88857791672651,11.5986492866067,-48.3459483822799));
#30777=CARTESIAN_POINT('Ctrl Pts',(1.48700388585266,11.5098560202878,-48.3492537158032));
#30778=CARTESIAN_POINT('Ctrl Pts',(0.785617178936058,11.4835302569327,-48.3550827158346));
#30779=CARTESIAN_POINT('Ctrl Pts',(0.0835265683594526,11.4728541727075,
-48.3550824830876));
#30780=CARTESIAN_POINT('Ctrl Pts',(4.2925657215965,11.6756605623744,-48.3310537580229));
#30781=CARTESIAN_POINT('Ctrl Pts',(4.29202351672922,11.6855354834088,-48.3351700984549));
#30782=CARTESIAN_POINT('Ctrl Pts',(4.29148046558877,11.6953464500614,-48.3386599861505));
#30783=CARTESIAN_POINT('Ctrl Pts',(4.2909421514954,11.7049048876128,-48.3415678448987));
#30784=CARTESIAN_POINT('Ctrl Pts',(4.29037098784448,11.7150466099943,-48.3446531500012));
#30785=CARTESIAN_POINT('Ctrl Pts',(4.28980526557442,11.7249027978756,-48.3470839291363));
#30786=CARTESIAN_POINT('Ctrl Pts',(4.28924925450923,11.734276287982,-48.3489664917434));
#30787=CARTESIAN_POINT('Ctrl Pts',(4.28866783699889,11.7440780916189,-48.350935076422));
#30788=CARTESIAN_POINT('Ctrl Pts',(4.28809709701726,11.7533514160685,-48.3523057468082));
#30789=CARTESIAN_POINT('Ctrl Pts',(4.28753799270913,11.7619163369651,-48.3532384552243));
#30790=CARTESIAN_POINT('Ctrl Pts',(4.28693019327239,11.7712272187112,-48.3542523977779));
#30791=CARTESIAN_POINT('Ctrl Pts',(4.28633615263105,11.779700856982,-48.3547509906821));
#30792=CARTESIAN_POINT('Ctrl Pts',(4.28575190459109,11.7871660424469,-48.3549537258283));
#30793=CARTESIAN_POINT('Ctrl Pts',(4.28551931560969,11.7901379306939,-48.3550344346333));
#30794=CARTESIAN_POINT('Ctrl Pts',(4.28528822465595,11.7929506159592,-48.3550682059901));
#30795=CARTESIAN_POINT('Ctrl Pts',(4.28505819640516,11.7955954176946,-48.3550682080605));
#30796=CARTESIAN_POINT('Ctrl Pts',(0.0835265683620996,11.6131136241746,
-48.3550682080606));
#30797=CARTESIAN_POINT('Ctrl Pts',(0.0835265683611482,11.5876793312944,
-48.3550682080606));
#30798=CARTESIAN_POINT('Ctrl Pts',(0.0835265683603323,11.5731362269333,
-48.3564911068706));
#30799=CARTESIAN_POINT('Ctrl Pts',(0.0835265683580835,11.5200575082527,
-48.3547257065812));
#30800=CARTESIAN_POINT('Ctrl Pts',(0.0835265683593817,11.4942063411577,
-48.3550829485814));
#30801=CARTESIAN_POINT('Ctrl Pts',(0.0835265683594526,11.4728541727075,
-48.3550824830876));
#30802=CARTESIAN_POINT('Ctrl Pts',(0.0835265683594526,11.4728541727075,
-48.3550824830876));
#30803=CARTESIAN_POINT('Ctrl Pts',(-0.267518736928885,11.47819221482,-48.3550825994609));
#30804=CARTESIAN_POINT('Ctrl Pts',(-0.618388066303173,11.4874426767152,
-48.3536254076396));
#30805=CARTESIAN_POINT('Ctrl Pts',(-1.31980082626874,11.5143737377395,-48.3502977991201));
#30806=CARTESIAN_POINT('Ctrl Pts',(-1.67034425686001,11.5320543368685,-48.3484273824219));
#30807=CARTESIAN_POINT('Ctrl Pts',(-2.72152478002693,11.598649286609,-48.3459483822804));
#30808=CARTESIAN_POINT('Ctrl Pts',(-3.42379713721014,11.6392592214975,-48.3412545192881));
#30809=CARTESIAN_POINT('Ctrl Pts',(-4.12551258855296,11.6756605207451,-48.3310538583792));
#30810=CARTESIAN_POINT('Ctrl Pts',(0.0835265683593817,11.4942063411577,
-48.3550829485814));
#30811=CARTESIAN_POINT('Ctrl Pts',(-0.189316787744158,11.4971000233707,
-48.3550233774032));
#30812=CARTESIAN_POINT('Ctrl Pts',(-0.484920402716805,11.5031786713304,
-48.3547116236149));
#30813=CARTESIAN_POINT('Ctrl Pts',(-1.12748086027463,11.5255419633083,-48.353447694585));
#30814=CARTESIAN_POINT('Ctrl Pts',(-1.47443454803614,11.5418711528751,-48.3525105585533));
#30815=CARTESIAN_POINT('Ctrl Pts',(-2.60108318320828,11.6120206208596,-48.3523410705539));
#30816=CARTESIAN_POINT('Ctrl Pts',(-3.35185488691515,11.6580360440938,-48.3492513442266));
#30817=CARTESIAN_POINT('Ctrl Pts',(-4.12419588880323,11.6996409410751,-48.3410500248244));
#30818=CARTESIAN_POINT('Ctrl Pts',(0.0835265683580835,11.5200575082527,
-48.3547257065812));
#30819=CARTESIAN_POINT('Ctrl Pts',(-0.189103448014727,11.5200113925675,
-48.3547233757333));
#30820=CARTESIAN_POINT('Ctrl Pts',(-0.484557203627196,11.5245005081763,
-48.3548266591895));
#30821=CARTESIAN_POINT('Ctrl Pts',(-1.12692130877498,11.5448479357178,-48.354482422056));
#30822=CARTESIAN_POINT('Ctrl Pts',(-1.47382850348662,11.5607507931991,-48.3540499406762));
#30823=CARTESIAN_POINT('Ctrl Pts',(-2.60045731732845,11.6290600690807,-48.3545898781102));
#30824=CARTESIAN_POINT('Ctrl Pts',(-3.35085409227056,11.6785648284704,-48.3527047664183));
#30825=CARTESIAN_POINT('Ctrl Pts',(-4.12290068806598,11.7229366511906,-48.3470536122447));
#30826=CARTESIAN_POINT('Ctrl Pts',(0.0835265683603323,11.5731362269333,
-48.3564911068706));
#30827=CARTESIAN_POINT('Ctrl Pts',(-0.227816669705091,11.5731490589917,
-48.3564923307038));
#30828=CARTESIAN_POINT('Ctrl Pts',(-0.550623003967762,11.5776504745528,
-48.3566275774405));
#30829=CARTESIAN_POINT('Ctrl Pts',(-1.22201691763608,11.5959692446123,-48.3565730737525));
#30830=CARTESIAN_POINT('Ctrl Pts',(-1.5706029196299,11.6098088718852,-48.3563908429328));
#30831=CARTESIAN_POINT('Ctrl Pts',(-2.65931970527722,11.6658592241826,-48.3563704085904));
#30832=CARTESIAN_POINT('Ctrl Pts',(-3.3845326024973,11.7135824344715,-48.3556131983326));
#30833=CARTESIAN_POINT('Ctrl Pts',(-4.12038695498559,11.7642258753785,-48.3540627038628));
#30834=CARTESIAN_POINT('Ctrl Pts',(0.0835265683611482,11.5876793312944,
-48.3550682080606));
#30835=CARTESIAN_POINT('Ctrl Pts',(-0.266743231127515,11.5876793312944,
-48.3550682080606));
#30836=CARTESIAN_POINT('Ctrl Pts',(-0.617052003400343,11.5930695682598,
-48.3550682080599));
#30837=CARTESIAN_POINT('Ctrl Pts',(-1.31767207799869,11.6126245374908,-48.3550682080582));
#30838=CARTESIAN_POINT('Ctrl Pts',(-1.66798338032422,11.6267892697563,-48.3550682080572));
#30839=CARTESIAN_POINT('Ctrl Pts',(-2.71880795910639,11.6794362415569,-48.3550682080552));
#30840=CARTESIAN_POINT('Ctrl Pts',(-3.41921190736862,11.728071256096,-48.3550682080552));
#30841=CARTESIAN_POINT('Ctrl Pts',(-4.11916842264246,11.7822193894509,-48.3550682080606));
#30842=CARTESIAN_POINT('Ctrl Pts',(0.0835265683620996,11.6131136241746,
-48.3550682080606));
#30843=CARTESIAN_POINT('Ctrl Pts',(-0.26682108424941,11.6131136241746,-48.3550682080606));
#30844=CARTESIAN_POINT('Ctrl Pts',(-0.617168736860919,11.6169153282063,
-48.35506820806));
#30845=CARTESIAN_POINT('Ctrl Pts',(-1.31778153573097,11.632122144333,-48.3550682080584));
#30846=CARTESIAN_POINT('Ctrl Pts',(-1.66804668198951,11.643527256428,-48.3550682080574));
#30847=CARTESIAN_POINT('Ctrl Pts',(-2.71859460170621,11.689147704808,-48.3550682080555));
#30848=CARTESIAN_POINT('Ctrl Pts',(-3.41862985610546,11.734768153188,-48.3550682080555));
#30849=CARTESIAN_POINT('Ctrl Pts',(-4.11800505968095,11.7955954176946,-48.3550682080606));
#30850=CARTESIAN_POINT('',(-4.12551258734455,11.6756605346478,-48.3310538248682));
#30851=CARTESIAN_POINT('Ctrl Pts',(-4.11800505968096,11.7955954176946,-48.3550682080605));
#30852=CARTESIAN_POINT('Ctrl Pts',(-4.11858674116171,11.7889074035727,-48.3550682028144));
#30853=CARTESIAN_POINT('Ctrl Pts',(-4.1191755024377,11.7811426004669,-48.3548536973611));
#30854=CARTESIAN_POINT('Ctrl Pts',(-4.11977717782812,11.7724551591809,-48.3542053100008));
#30855=CARTESIAN_POINT('Ctrl Pts',(-4.12032676070816,11.7645198686933,-48.353613059431));
#30856=CARTESIAN_POINT('Ctrl Pts',(-4.12088714071915,11.7558145072651,-48.3526569060054));
#30857=CARTESIAN_POINT('Ctrl Pts',(-4.121459096528,11.746498740511,-48.351169033279));
#30858=CARTESIAN_POINT('Ctrl Pts',(-4.12200329730859,11.7376350355518,-48.3497533618467));
#30859=CARTESIAN_POINT('Ctrl Pts',(-4.12255795151647,11.7282190174497,-48.3478548932889));
#30860=CARTESIAN_POINT('Ctrl Pts',(-4.12312028565963,11.7184280696927,-48.345351573475));
#30861=CARTESIAN_POINT('Ctrl Pts',(-4.12365588800086,11.7091025563741,-48.342967254526));
#30862=CARTESIAN_POINT('Ctrl Pts',(-4.12419838506679,11.6994377386552,-48.3400333160227));
#30863=CARTESIAN_POINT('Ctrl Pts',(-4.12474290719614,11.689615689668,-48.3364817624102));
#30864=CARTESIAN_POINT('Ctrl Pts',(-4.124999256702,11.6849916766689,-48.3348097660587));
#30865=CARTESIAN_POINT('Ctrl Pts',(-4.12525602496188,11.6803331677638,-48.3330015237243));
#30866=CARTESIAN_POINT('Ctrl Pts',(-4.12551258492773,11.6756605624531,-48.3310537578461));
#30867=CARTESIAN_POINT('Ctrl Pts',(-4.12551258855296,11.6756605207451,-48.3310538583792));
#30868=CARTESIAN_POINT('Ctrl Pts',(-3.42379713721014,11.6392592214975,-48.3412545192881));
#30869=CARTESIAN_POINT('Ctrl Pts',(-2.72152478002693,11.598649286609,-48.3459483822803));
#30870=CARTESIAN_POINT('Ctrl Pts',(-1.3199507491377,11.5098560202884,-48.3492537158024));
#30871=CARTESIAN_POINT('Ctrl Pts',(-0.618564042217223,11.4835302569325,
-48.3550827158344));
#30872=CARTESIAN_POINT('Ctrl Pts',(0.0835265683594526,11.4728541727075,
-48.3550824830876));
#30873=CARTESIAN_POINT('Ctrl Pts',(0.0835265683594526,11.4728541727075,
-48.3550824830876));
#30874=CARTESIAN_POINT('Ctrl Pts',(-0.267518736928849,11.4675161305949,
-48.355082366714));
#30875=CARTESIAN_POINT('Ctrl Pts',(-0.618615979874604,11.4659265087691,
-48.3536249385705));
#30876=CARTESIAN_POINT('Ctrl Pts',(-1.32094154343241,11.464396632877,-48.3438941182179));
#30877=CARTESIAN_POINT('Ctrl Pts',(-1.67216986404445,11.4644563788108,-48.3356207260088));
#30878=CARTESIAN_POINT('Ctrl Pts',(-2.7260922459071,11.4583384590299,-48.2947245924949));
#30879=CARTESIAN_POINT('Ctrl Pts',(-3.42734501838564,11.4609474762042,-48.2515240163504));
#30880=CARTESIAN_POINT('Ctrl Pts',(-4.12845481065586,11.4732422824942,-48.1954680629781));
#30881=CARTESIAN_POINT('Ctrl Pts',(-0.267518736928885,11.47819221482,-48.3550825994609));
#30882=CARTESIAN_POINT('Ctrl Pts',(-0.540535157210003,11.474986089803,-48.3541407510372));
#30883=CARTESIAN_POINT('Ctrl Pts',(-0.831623019773455,11.4745419834778,
-48.3520530938263));
#30884=CARTESIAN_POINT('Ctrl Pts',(-1.44672511025184,11.4744825705814,-48.3421773991251));
#30885=CARTESIAN_POINT('Ctrl Pts',(-1.77074437310434,11.4748353413217,-48.3343702273172));
#30886=CARTESIAN_POINT('Ctrl Pts',(-2.78737351666232,11.4700074930206,-48.294291871146));
#30887=CARTESIAN_POINT('Ctrl Pts',(-3.4643207611869,11.4731609516944,-48.2527720831625));
#30888=CARTESIAN_POINT('Ctrl Pts',(-4.12850749787586,11.4851966459098,-48.200433936555));
#30889=CARTESIAN_POINT('Ctrl Pts',(-0.618388066303173,11.4874426767152,
-48.3536254076396));
#30890=CARTESIAN_POINT('Ctrl Pts',(-0.831277825867611,11.484480312248,-48.3524253715951));
#30891=CARTESIAN_POINT('Ctrl Pts',(-1.07630838599441,11.4840908039498,-48.3500372977493));
#30892=CARTESIAN_POINT('Ctrl Pts',(-1.62065368486988,11.4843329006937,-48.3401377766501));
#30893=CARTESIAN_POINT('Ctrl Pts',(-1.91997597602491,11.4849166217029,-48.3325976279206));
#30894=CARTESIAN_POINT('Ctrl Pts',(-2.88438286235813,11.4818828006798,-48.2936814855076));
#30895=CARTESIAN_POINT('Ctrl Pts',(-3.52649817574215,11.4863352799679,-48.25411650478));
#30896=CARTESIAN_POINT('Ctrl Pts',(-4.12864057911575,11.497472006951,-48.2071191491468));
#30897=CARTESIAN_POINT('Ctrl Pts',(-1.31980082626874,11.5143737377395,-48.3502977991201));
#30898=CARTESIAN_POINT('Ctrl Pts',(-1.44516286660466,11.5105174196343,-48.3485410607117));
#30899=CARTESIAN_POINT('Ctrl Pts',(-1.61934713769631,11.5090816899187,-48.3454511925548));
#30900=CARTESIAN_POINT('Ctrl Pts',(-2.04329098360778,11.5079260458441,-48.3350871090446));
#30901=CARTESIAN_POINT('Ctrl Pts',(-2.29305999893556,11.508146276444,-48.3277770168462));
#30902=CARTESIAN_POINT('Ctrl Pts',(-3.12263861219824,11.5065304546903,-48.29168097615));
#30903=CARTESIAN_POINT('Ctrl Pts',(-3.67166031045832,11.5121367174565,-48.2567445234558));
#30904=CARTESIAN_POINT('Ctrl Pts',(-4.1292012092717,11.5208685373805,-48.221588093388));
#30905=CARTESIAN_POINT('Ctrl Pts',(-1.67034425686001,11.5320543368685,-48.3484273824219));
#30906=CARTESIAN_POINT('Ctrl Pts',(-1.76830361911727,11.5270830007426,-48.3463749782915));
#30907=CARTESIAN_POINT('Ctrl Pts',(-1.917698093827,11.5245577996658,-48.342885156969));
#30908=CARTESIAN_POINT('Ctrl Pts',(-2.29199667103983,11.5217114161951,-48.3320814058286));
#30909=CARTESIAN_POINT('Ctrl Pts',(-2.51690958468367,11.521334369096,-48.3247339909552));
#30910=CARTESIAN_POINT('Ctrl Pts',(-3.26388339677572,11.5193254972085,-48.290293701452));
#30911=CARTESIAN_POINT('Ctrl Pts',(-3.75464503061926,11.5247638266718,-48.258028120514));
#30912=CARTESIAN_POINT('Ctrl Pts',(-4.12962875818775,11.5319897067687,-48.2293718250375));
#30913=CARTESIAN_POINT('Ctrl Pts',(-2.72152478002693,11.598649286609,-48.3459483822803));
#30914=CARTESIAN_POINT('Ctrl Pts',(-2.7817504873063,11.5919036248662,-48.3427355509081));
#30915=CARTESIAN_POINT('Ctrl Pts',(-2.87872640930532,11.5859418512212,-48.3377026419578));
#30916=CARTESIAN_POINT('Ctrl Pts',(-3.11802711878623,11.5755468354635,-48.3246778344466));
#30917=CARTESIAN_POINT('Ctrl Pts',(-3.2603569412057,11.5710816706623,-48.3166668015682));
#30918=CARTESIAN_POINT('Ctrl Pts',(-3.71314894654688,11.5598336028535,-48.2862238405639));
#30919=CARTESIAN_POINT('Ctrl Pts',(-3.99041609265724,11.5581209387927,-48.2614073735946));
#30920=CARTESIAN_POINT('Ctrl Pts',(-4.13155362590472,11.5609276470972,-48.2508605601154));
#30921=CARTESIAN_POINT('Ctrl Pts',(-3.42379713721014,11.6392592214975,-48.3412545192881));
#30922=CARTESIAN_POINT('Ctrl Pts',(-3.45976826235763,11.6298708101994,-48.3372561068189));
#30923=CARTESIAN_POINT('Ctrl Pts',(-3.52173695764161,11.6209827896646,-48.3313642361189));
#30924=CARTESIAN_POINT('Ctrl Pts',(-3.66733281854159,11.6050189470302,-48.3171415021054));
#30925=CARTESIAN_POINT('Ctrl Pts',(-3.75095998415758,11.5979431249306,-48.3088106387919));
#30926=CARTESIAN_POINT('Ctrl Pts',(-3.98882418159218,11.5806510816468,-48.2821814457032));
#30927=CARTESIAN_POINT('Ctrl Pts',(-4.13001933608944,11.5743267261738,-48.2630314915227));
#30928=CARTESIAN_POINT('Ctrl Pts',(-4.13369316567444,11.5743188502015,-48.2627031036729));
#30929=CARTESIAN_POINT('Ctrl Pts',(-4.12551258855296,11.6756605207451,-48.3310538583792));
#30930=CARTESIAN_POINT('Ctrl Pts',(-4.12617093842782,11.6636703105801,-48.3260557751567));
#30931=CARTESIAN_POINT('Ctrl Pts',(-4.12683967786648,11.6514649415886,-48.319925579004));
#30932=CARTESIAN_POINT('Ctrl Pts',(-4.12827545214397,11.6282480883359,-48.3065253445687));
#30933=CARTESIAN_POINT('Ctrl Pts',(-4.12904248698282,11.6172366040747,-48.299255306286));
#30934=CARTESIAN_POINT('Ctrl Pts',(-4.13160730900852,11.588429281961,-48.2774220038378));
#30935=CARTESIAN_POINT('Ctrl Pts',(-4.13366096331954,11.5746245276893,-48.2630127553113));
#30936=CARTESIAN_POINT('Ctrl Pts',(-4.13722371861475,11.5746245485739,-48.2627017315157));
#30937=CARTESIAN_POINT('Ctrl Pts',(-4.12551258855296,11.6756605207451,-48.3310538583792));
#30938=CARTESIAN_POINT('Ctrl Pts',(-4.12682928830268,11.6516801004151,-48.3210576919341));
#30939=CARTESIAN_POINT('Ctrl Pts',(-4.12818754630759,11.6268390447792,-48.3065330737686));
#30940=CARTESIAN_POINT('Ctrl Pts',(-4.13160730900852,11.588429281961,-48.2774220038378));
#30941=CARTESIAN_POINT('Ctrl Pts',(-4.13366096331954,11.5746245276893,-48.2630127553113));
#30942=CARTESIAN_POINT('Ctrl Pts',(-4.13722371861476,11.5746245485739,-48.2627017315157));
#30943=CARTESIAN_POINT('',(-4.12845481065586,11.4732422824942,-48.1954680629781));
#30944=CARTESIAN_POINT('Ctrl Pts',(-4.12845481065586,11.4732422824942,-48.1954680629781));
#30945=CARTESIAN_POINT('Ctrl Pts',(-4.12847724604266,11.4783327155669,-48.197582642083));
#30946=CARTESIAN_POINT('Ctrl Pts',(-4.12851349517641,11.4833192294908,-48.1999372550416));
#30947=CARTESIAN_POINT('Ctrl Pts',(-4.12856659581727,11.4882155782114,-48.2024493601598));
#30948=CARTESIAN_POINT('Ctrl Pts',(-4.1286324082246,11.4942840642271,-48.2055628383147));
#30949=CARTESIAN_POINT('Ctrl Pts',(-4.12872385562462,11.5002159367925,-48.2089197658545));
#30950=CARTESIAN_POINT('Ctrl Pts',(-4.12884968400471,11.5060421990484,-48.2124409973493));
#30951=CARTESIAN_POINT('Ctrl Pts',(-4.12887227574559,11.5070882699516,-48.2130732136224));
#30952=CARTESIAN_POINT('Ctrl Pts',(-4.12889598894898,11.5081309125981,-48.213710857774));
#30953=CARTESIAN_POINT('Ctrl Pts',(-4.12892089419373,11.5091702721658,-48.2143536212674));
#30954=CARTESIAN_POINT('Ctrl Pts',(-4.12907740654552,11.515701932945,-48.2183929482053));
#30955=CARTESIAN_POINT('Ctrl Pts',(-4.12927928751034,11.5221052499854,-48.2226316728729));
#30956=CARTESIAN_POINT('Ctrl Pts',(-4.12955440608205,11.5284062582695,-48.2270159410459));
#30957=CARTESIAN_POINT('Ctrl Pts',(-4.12974914542339,11.5328663504957,-48.2301192920516));
#30958=CARTESIAN_POINT('Ctrl Pts',(-4.1299802484247,11.5372739158669,-48.2332957729108));
#30959=CARTESIAN_POINT('Ctrl Pts',(-4.13027038076007,11.5416356868782,-48.2365347367302));
#30960=CARTESIAN_POINT('Ctrl Pts',(-4.13051330836706,11.545287794778,-48.2392467189322));
#30961=CARTESIAN_POINT('Ctrl Pts',(-4.13079649629707,11.5489068236642,-48.2420019879108));
#30962=CARTESIAN_POINT('Ctrl Pts',(-4.13115207407033,11.5524928731301,-48.2447943975055));
#30963=CARTESIAN_POINT('Ctrl Pts',(-4.13140677308046,11.5550615467591,-48.2467945899054));
#30964=CARTESIAN_POINT('Ctrl Pts',(-4.13169781691591,11.5576142914133,-48.2488147085002));
#30965=CARTESIAN_POINT('Ctrl Pts',(-4.13205749655601,11.5601495956737,-48.2508517250196));
#30966=CARTESIAN_POINT('Ctrl Pts',(-4.13230907506287,11.5619229183452,-48.2522765195236));
#30967=CARTESIAN_POINT('Ctrl Pts',(-4.13259322084644,11.5636878343141,-48.253709749953));
#30968=CARTESIAN_POINT('Ctrl Pts',(-4.13294254831288,11.5654435821136,-48.2551496626094));
#30969=CARTESIAN_POINT('Ctrl Pts',(-4.13317705493165,11.5666222311447,-48.2561162887147));
#30970=CARTESIAN_POINT('Ctrl Pts',(-4.13343997566705,11.5677969692623,-48.2570861853592));
#30971=CARTESIAN_POINT('Ctrl Pts',(-4.13376223323209,11.5689658159629,-48.2580563995925));
#30972=CARTESIAN_POINT('Ctrl Pts',(-4.13395686573063,11.5696717592159,-48.2586423756589));
#30973=CARTESIAN_POINT('Ctrl Pts',(-4.13417293995391,11.5703762086922,-48.2592290531955));
#30974=CARTESIAN_POINT('Ctrl Pts',(-4.13443138997987,11.5710757337678,-48.259812391898));
#30975=CARTESIAN_POINT('Ctrl Pts',(-4.13461059905206,11.5715607839794,-48.2602168785575));
#30976=CARTESIAN_POINT('Ctrl Pts',(-4.13481062697808,11.5720464962208,-48.2606223555231));
#30977=CARTESIAN_POINT('Ctrl Pts',(-4.13505139716509,11.5725238643872,-48.2610197986288));
#30978=CARTESIAN_POINT('Ctrl Pts',(-4.13521808348396,11.5728543485863,-48.261294950337));
#30979=CARTESIAN_POINT('Ctrl Pts',(-4.13540552833946,11.5731846562113,-48.2615695100043));
#30980=CARTESIAN_POINT('Ctrl Pts',(-4.1356319850481,11.5734998993923,-48.2618291616974));
#30981=CARTESIAN_POINT('Ctrl Pts',(-4.13573263391391,11.5736400094769,-48.2619445641006));
#30982=CARTESIAN_POINT('Ctrl Pts',(-4.13584148560198,11.5737774981193,-48.2620572934349));
#30983=CARTESIAN_POINT('Ctrl Pts',(-4.13596273598079,11.5739092744925,-48.2621643000755));
#30984=CARTESIAN_POINT('Ctrl Pts',(-4.13604421784951,11.5739978299696,-48.2622362099625));
#30985=CARTESIAN_POINT('Ctrl Pts',(-4.13612859548604,11.5740821529239,-48.2623042726689));
#30986=CARTESIAN_POINT('Ctrl Pts',(-4.13623430704625,11.5741721054098,-48.2623758167973));
#30987=CARTESIAN_POINT('Ctrl Pts',(-4.13628716282636,11.5742170816527,-48.2624115888615));
#30988=CARTESIAN_POINT('Ctrl Pts',(-4.13634156211114,11.5742618826266,-48.2624471111769));
#30989=CARTESIAN_POINT('Ctrl Pts',(-4.13643190399437,11.5743239422309,-48.262495252223));
#30990=CARTESIAN_POINT('Ctrl Pts',(-4.13647707491214,11.5743549720167,-48.2625193227333));
#30991=CARTESIAN_POINT('Ctrl Pts',(-4.13654109921554,11.5743996848316,-48.2625541029385));
#30992=CARTESIAN_POINT('Ctrl Pts',(-4.13665995702445,11.5744597225478,-48.2625983712319));
#30993=CARTESIAN_POINT('Ctrl Pts',(-4.13674744934593,11.5745039168605,-48.262630957528));
#30994=CARTESIAN_POINT('Ctrl Pts',(-4.13686460908674,11.5745568559735,-48.2626691138439));
#30995=CARTESIAN_POINT('Ctrl Pts',(-4.13702846629035,11.5745940265261,-48.2626896148542));
#30996=CARTESIAN_POINT('Ctrl Pts',(-4.13708720814305,11.5746073519526,-48.2626969643469));
#30997=CARTESIAN_POINT('Ctrl Pts',(-4.13715198465268,11.5746183373345,-48.2627017593562));
#30998=CARTESIAN_POINT('Ctrl Pts',(-4.13722371775385,11.5746245484993,-48.2627017315161));
#30999=CARTESIAN_POINT('Ctrl Pts',(-4.12845481065586,11.4732422824942,-48.1954680629781));
#31000=CARTESIAN_POINT('Ctrl Pts',(-3.42734501838564,11.4609474762041,-48.2515240163504));
#31001=CARTESIAN_POINT('Ctrl Pts',(-2.7260922459071,11.45833845903,-48.2947245924949));
#31002=CARTESIAN_POINT('Ctrl Pts',(-1.32086240342357,11.4664956854044,-48.3492527705134));
#31003=CARTESIAN_POINT('Ctrl Pts',(-0.618564042217151,11.4621780884823,
-48.3550822503405));
#31004=CARTESIAN_POINT('Ctrl Pts',(0.0835265683594526,11.4728541727075,
-48.3550824830876));
#31005=CARTESIAN_POINT('Ctrl Pts',(0.0835265683594526,11.4728541727075,
-48.3550824830876));
#31006=CARTESIAN_POINT('Ctrl Pts',(0.0835265683595233,11.4515020042572,
-48.3550820175938));
#31007=CARTESIAN_POINT('Ctrl Pts',(0.0835265683609461,11.4284235901226,
-48.3547237088909));
#31008=CARTESIAN_POINT('Ctrl Pts',(0.083526568361231,11.3941472536996,-48.350619056743));
#31009=CARTESIAN_POINT('Ctrl Pts',(0.0835265683612866,11.3720285904897,
-48.3550682080606));
#31010=CARTESIAN_POINT('Ctrl Pts',(0.0835265683620956,11.3536536794531,
-48.3550682080606));
#31011=CARTESIAN_POINT('Ctrl Pts',(-0.267518736928849,11.4675161305949,
-48.355082366714));
#31012=CARTESIAN_POINT('Ctrl Pts',(-0.189662916098598,11.4488974993902,
-48.3550223265509));
#31013=CARTESIAN_POINT('Ctrl Pts',(-0.172476876269728,11.4285976962987,
-48.3547580080055));
#31014=CARTESIAN_POINT('Ctrl Pts',(-0.19427927370922,11.3940705712691,-48.3505964242949));
#31015=CARTESIAN_POINT('Ctrl Pts',(-0.233267710976564,11.3720285904897,
-48.3550682080606));
#31016=CARTESIAN_POINT('Ctrl Pts',(-0.26776084433578,11.3536536794531,-48.3550682080606));
#31017=CARTESIAN_POINT('Ctrl Pts',(-0.618615979874604,11.4659265087691,
-48.3536249385705));
#31018=CARTESIAN_POINT('Ctrl Pts',(-0.485248141787488,11.447718516688,-48.3538283041916));
#31019=CARTESIAN_POINT('Ctrl Pts',(-0.459481328458187,11.428587933622,-48.3533940028244));
#31020=CARTESIAN_POINT('Ctrl Pts',(-0.500506504781256,11.3934281614349,
-48.3484833203952));
#31021=CARTESIAN_POINT('Ctrl Pts',(-0.567298494432773,11.3718199008203,
-48.3519505469255));
#31022=CARTESIAN_POINT('Ctrl Pts',(-0.619048262304807,11.3536536794531,
-48.3512468523357));
#31023=CARTESIAN_POINT('Ctrl Pts',(-1.32094154343241,11.464396632877,-48.3438941182179));
#31024=CARTESIAN_POINT('Ctrl Pts',(-1.12790203394888,11.4452664260876,-48.3454622940091));
#31025=CARTESIAN_POINT('Ctrl Pts',(-1.09571051627679,11.4271829834973,-48.3443038073303));
#31026=CARTESIAN_POINT('Ctrl Pts',(-1.16018842034295,11.3913038531299,-48.3372314655874));
#31027=CARTESIAN_POINT('Ctrl Pts',(-1.25685784208063,11.3711415135622,-48.3377896456608));
#31028=CARTESIAN_POINT('Ctrl Pts',(-1.32154021141497,11.3536536794531,-48.3359596079612));
#31029=CARTESIAN_POINT('Ctrl Pts',(-1.67216986404445,11.4644563788108,-48.3356207260088));
#31030=CARTESIAN_POINT('Ctrl Pts',(-1.47497921486972,11.443938017789,-48.3381640344641));
#31031=CARTESIAN_POINT('Ctrl Pts',(-1.44494173036685,11.4257324956489,-48.3364512936465));
#31032=CARTESIAN_POINT('Ctrl Pts',(-1.51364329271565,11.389794304459,-48.3280294754275));
#31033=CARTESIAN_POINT('Ctrl Pts',(-1.61238233956687,11.3706718159735,-48.3267463020471));
#31034=CARTESIAN_POINT('Ctrl Pts',(-1.67274475309907,11.3536536794531,-48.3244937189391));
#31035=CARTESIAN_POINT('Ctrl Pts',(-2.37478478528622,11.4603777656235,-48.3083566369995));
#31036=CARTESIAN_POINT('Ctrl Pts',(-2.22731576370123,11.4381382649982,-48.3098281543322));
#31037=CARTESIAN_POINT('Ctrl Pts',(-2.20580868481744,11.4203247666437,-48.307328281957));
#31038=CARTESIAN_POINT('Ctrl Pts',(-2.25808685967459,11.3861758639155,-48.2988519282882));
#31039=CARTESIAN_POINT('Ctrl Pts',(-2.3318721134153,11.3696277842964,-48.2961657002409));
#31040=CARTESIAN_POINT('Ctrl Pts',(-2.37498775707866,11.3536536794531,-48.2939119483841));
#31041=CARTESIAN_POINT('Ctrl Pts',(-2.7257517087163,11.4600103666203,-48.2907404707111));
#31042=CARTESIAN_POINT('Ctrl Pts',(-2.60287727457564,11.4370088609558,-48.2910861014142));
#31043=CARTESIAN_POINT('Ctrl Pts',(-2.58784945387008,11.4187667259072,-48.2880098223025));
#31044=CARTESIAN_POINT('Ctrl Pts',(-2.63432748053576,11.3847952022384,-48.2796807289492));
#31045=CARTESIAN_POINT('Ctrl Pts',(-2.69583332790684,11.369053450208,-48.2766286482955));
#31046=CARTESIAN_POINT('Ctrl Pts',(-2.72602622991903,11.3536536794531,-48.2747960661052));
#31047=CARTESIAN_POINT('Ctrl Pts',(-3.42730927333356,11.4633689234831,-48.2483101720435));
#31048=CARTESIAN_POINT('Ctrl Pts',(-3.35965513497476,11.4394032486783,-48.2448130738858));
#31049=CARTESIAN_POINT('Ctrl Pts',(-3.35545842749711,11.4193327724023,-48.2403172932759));
#31050=CARTESIAN_POINT('Ctrl Pts',(-3.38522478863114,11.3835624194323,-48.232439703259));
#31051=CARTESIAN_POINT('Ctrl Pts',(-3.4191878572428,11.3679565169509,-48.2296135008165));
#31052=CARTESIAN_POINT('Ctrl Pts',(-3.42785327106255,11.3536536794531,-48.2289052281065));
#31053=CARTESIAN_POINT('Ctrl Pts',(-3.77789991452075,11.4670948793492,-48.2234960396643));
#31054=CARTESIAN_POINT('Ctrl Pts',(-3.74087148449948,11.4429270404433,-48.2172820992753));
#31055=CARTESIAN_POINT('Ctrl Pts',(-3.74102460769126,11.4214568596339,-48.2119434824081));
#31056=CARTESIAN_POINT('Ctrl Pts',(-3.7598774297419,11.3837102983034,-48.2043703936356));
#31057=CARTESIAN_POINT('Ctrl Pts',(-3.77857712860076,11.3674339177823,-48.2021359217303));
#31058=CARTESIAN_POINT('Ctrl Pts',(-3.77864184991365,11.3536536794531,-48.2021302712649));
#31059=CARTESIAN_POINT('Ctrl Pts',(-4.12845481065586,11.4732422824942,-48.1954680629781));
#31060=CARTESIAN_POINT('Ctrl Pts',(-4.12834943621585,11.4493335556629,-48.1855363158243));
#31061=CARTESIAN_POINT('Ctrl Pts',(-4.12855150591032,11.4261172510677,-48.1795491602216));
#31062=CARTESIAN_POINT('Ctrl Pts',(-4.12900833251927,11.384958159128,-48.1725407225933));
#31063=CARTESIAN_POINT('Ctrl Pts',(-4.12926308943375,11.3670153717833,-48.1715194405676));
#31064=CARTESIAN_POINT('Ctrl Pts',(-4.12926308943375,11.3536536794531,-48.1715194405676));
#31065=CARTESIAN_POINT('Origin',(-4.155077712629,11.3534224546477,-48.4841190147253));
#31066=CARTESIAN_POINT('Ctrl Pts',(0.0835265683620358,11.3536536794531,
-48.3550682080606));
#31067=CARTESIAN_POINT('Ctrl Pts',(0.0835265683612866,11.3720285904897,
-48.3550682080606));
#31068=CARTESIAN_POINT('Ctrl Pts',(0.083526568361231,11.3941472536996,-48.350619056743));
#31069=CARTESIAN_POINT('Ctrl Pts',(0.0835265683609461,11.4284235901226,
-48.3547237088909));
#31070=CARTESIAN_POINT('Ctrl Pts',(0.0835265683595233,11.4515020042572,
-48.3550820175938));
#31071=CARTESIAN_POINT('Ctrl Pts',(0.0835265683594526,11.4728541727075,
-48.3550824830876));
#31072=CARTESIAN_POINT('Ctrl Pts',(0.0835265683594526,11.4728541727075,
-48.3550824830876));
#31073=CARTESIAN_POINT('Ctrl Pts',(0.43457187364779,11.467516130595,-48.3550823667143));
#31074=CARTESIAN_POINT('Ctrl Pts',(0.785669116593031,11.4659265087692,-48.353624938571));
#31075=CARTESIAN_POINT('Ctrl Pts',(1.48799468014872,11.4643966328772,-48.3438941182188));
#31076=CARTESIAN_POINT('Ctrl Pts',(1.83922300075916,11.4644563788109,-48.3356207260099));
#31077=CARTESIAN_POINT('Ctrl Pts',(2.54183792199666,11.4603777656235,-48.3083566370006));
#31078=CARTESIAN_POINT('Ctrl Pts',(2.89280484542876,11.4600103666202,-48.2907404707119));
#31079=CARTESIAN_POINT('Ctrl Pts',(3.59436241005202,11.463368923483,-48.2483101720439));
#31080=CARTESIAN_POINT('Ctrl Pts',(3.94495305124318,11.4670948793491,-48.2234960396644));
#31081=CARTESIAN_POINT('Ctrl Pts',(4.29550794738005,11.4732422824942,-48.1954680629781));
#31082=CARTESIAN_POINT('Ctrl Pts',(0.0835265683595233,11.4515020042572,
-48.3550820175938));
#31083=CARTESIAN_POINT('Ctrl Pts',(0.356716052817998,11.4488974993903,-48.3550223265511));
#31084=CARTESIAN_POINT('Ctrl Pts',(0.652301278506739,11.4477185166882,-48.353828304192));
#31085=CARTESIAN_POINT('Ctrl Pts',(1.2949551706665,11.4452664260879,-48.34546229401));
#31086=CARTESIAN_POINT('Ctrl Pts',(1.64203235158588,11.4439380177893,-48.3381640344652));
#31087=CARTESIAN_POINT('Ctrl Pts',(2.39436890041279,11.4381382649983,-48.3098281543332));
#31088=CARTESIAN_POINT('Ctrl Pts',(2.76993041128897,11.4370088609558,-48.2910861014151));
#31089=CARTESIAN_POINT('Ctrl Pts',(3.52670827169359,11.4394032486783,-48.2448130738862));
#31090=CARTESIAN_POINT('Ctrl Pts',(3.90792462122203,11.4429270404433,-48.2172820992754));
#31091=CARTESIAN_POINT('Ctrl Pts',(4.29540257294004,11.4493335556629,-48.1855363158243));
#31092=CARTESIAN_POINT('Ctrl Pts',(0.0835265683609461,11.4284235901226,
-48.3547237088909));
#31093=CARTESIAN_POINT('Ctrl Pts',(0.33953001299162,11.4285976962988,-48.3547580080057));
#31094=CARTESIAN_POINT('Ctrl Pts',(0.626534465179757,11.4285879336221,-48.3533940028248));
#31095=CARTESIAN_POINT('Ctrl Pts',(1.26276365299677,11.4271829834975,-48.344303807331));
#31096=CARTESIAN_POINT('Ctrl Pts',(1.61199486708556,11.4257324956492,-48.3364512936473));
#31097=CARTESIAN_POINT('Ctrl Pts',(2.37286182153235,11.4203247666439,-48.3073282819579));
#31098=CARTESIAN_POINT('Ctrl Pts',(2.75490259058618,11.4187667259073,-48.2880098223032));
#31099=CARTESIAN_POINT('Ctrl Pts',(3.52251156421718,11.4193327724023,-48.2403172932763));
#31100=CARTESIAN_POINT('Ctrl Pts',(3.90807774441412,11.4214568596339,-48.2119434824082));
#31101=CARTESIAN_POINT('Ctrl Pts',(4.29560464263451,11.4261172510678,-48.1795491602216));
#31102=CARTESIAN_POINT('Ctrl Pts',(0.083526568361231,11.3941472536996,-48.350619056743));
#31103=CARTESIAN_POINT('Ctrl Pts',(0.361332410431682,11.3940705712691,-48.350596424295));
#31104=CARTESIAN_POINT('Ctrl Pts',(0.667559641503652,11.393428161435,-48.3484833203954));
#31105=CARTESIAN_POINT('Ctrl Pts',(1.32724155706492,11.39130385313,-48.3372314655877));
#31106=CARTESIAN_POINT('Ctrl Pts',(1.68069642943727,11.3897943044591,-48.3280294754278));
#31107=CARTESIAN_POINT('Ctrl Pts',(2.42513999639505,11.3861758639155,-48.2988519282886));
#31108=CARTESIAN_POINT('Ctrl Pts',(2.8013806172567,11.3847952022384,-48.2796807289495));
#31109=CARTESIAN_POINT('Ctrl Pts',(3.55227792535362,11.3835624194324,-48.2324397032591));
#31110=CARTESIAN_POINT('Ctrl Pts',(3.92693056646546,11.3837102983034,-48.2043703936356));
#31111=CARTESIAN_POINT('Ctrl Pts',(4.29606146924347,11.384958159128,-48.1725407225933));
#31112=CARTESIAN_POINT('Ctrl Pts',(0.0835265683612866,11.3720285904897,
-48.3550682080606));
#31113=CARTESIAN_POINT('Ctrl Pts',(0.400320847699137,11.3720285904897,-48.3550682080606));
#31114=CARTESIAN_POINT('Ctrl Pts',(0.734351631155381,11.3718199008203,-48.3519505469256));
#31115=CARTESIAN_POINT('Ctrl Pts',(1.42391097880337,11.3711415135622,-48.3377896456608));
#31116=CARTESIAN_POINT('Ctrl Pts',(1.77943547628973,11.3706718159735,-48.3267463020472));
#31117=CARTESIAN_POINT('Ctrl Pts',(2.49892525013843,11.3696277842964,-48.296165700241));
#31118=CARTESIAN_POINT('Ctrl Pts',(2.86288646463014,11.369053450208,-48.2766286482956));
#31119=CARTESIAN_POINT('Ctrl Pts',(3.58624099396651,11.3679565169509,-48.2296135008166));
#31120=CARTESIAN_POINT('Ctrl Pts',(3.9456302653247,11.3674339177823,-48.2021359217302));
#31121=CARTESIAN_POINT('Ctrl Pts',(4.29631622615795,11.3670153717833,-48.1715194405676));
#31122=CARTESIAN_POINT('Ctrl Pts',(0.0835265683620956,11.3536536794531,
-48.3550682080606));
#31123=CARTESIAN_POINT('Ctrl Pts',(0.434813981059971,11.3536536794531,-48.3550682080606));
#31124=CARTESIAN_POINT('Ctrl Pts',(0.786101399028999,11.3536536794531,-48.3512468523357));
#31125=CARTESIAN_POINT('Ctrl Pts',(1.48859334813917,11.3536536794531,-48.3359596079612));
#31126=CARTESIAN_POINT('Ctrl Pts',(1.83979788982327,11.3536536794531,-48.3244937189391));
#31127=CARTESIAN_POINT('Ctrl Pts',(2.54204089380286,11.3536536794531,-48.293911948384));
#31128=CARTESIAN_POINT('Ctrl Pts',(2.89307936664324,11.3536536794531,-48.2747960661052));
#31129=CARTESIAN_POINT('Ctrl Pts',(3.59490640778675,11.3536536794531,-48.2289052281065));
#31130=CARTESIAN_POINT('Ctrl Pts',(3.94569498663785,11.353653679453,-48.2021302712649));
#31131=CARTESIAN_POINT('Ctrl Pts',(4.29631622615795,11.353653679453,-48.1715194405676));
#31132=CARTESIAN_POINT('',(4.29550794738005,11.4732422824942,-48.1954680629781));
#31133=CARTESIAN_POINT('Origin',(4.32213084935235,11.3534224546478,-48.484119014725));
#31134=CARTESIAN_POINT('Ctrl Pts',(4.29550794738005,11.4732422824942,-48.1954680629781));
#31135=CARTESIAN_POINT('Ctrl Pts',(3.59439815510631,11.4609474762041,-48.2515240163507));
#31136=CARTESIAN_POINT('Ctrl Pts',(2.89314538261541,11.4583384590298,-48.2947245924959));
#31137=CARTESIAN_POINT('Ctrl Pts',(1.48791554014041,11.4664956854045,-48.3492527705145));
#31138=CARTESIAN_POINT('Ctrl Pts',(0.785617178936127,11.4621780884824,-48.355082250341));
#31139=CARTESIAN_POINT('Ctrl Pts',(0.0835265683594526,11.4728541727075,
-48.3550824830876));
#31140=CARTESIAN_POINT('Origin',(-44.291473431638,16.1705954176946,-48.6675682080606));
#31141=CARTESIAN_POINT('Origin',(21.5192211643356,16.1705954176946,-48.6675682080606));
#31142=CARTESIAN_POINT('Origin',(-21.3521680276115,16.1705954176946,-48.6675682080606));
#31143=CARTESIAN_POINT('Ctrl Pts',(21.5192211643355,16.1705954176947,-48.3550682080606));
#31144=CARTESIAN_POINT('Ctrl Pts',(21.5192211643355,16.4830954176946,-48.3550682080606));
#31145=CARTESIAN_POINT('Ctrl Pts',(21.5192211643356,16.4830954176946,-48.6675682080606));
#31146=CARTESIAN_POINT('Ctrl Pts',(21.7183268789094,16.2080049077902,-48.3550682080606));
#31147=CARTESIAN_POINT('Ctrl Pts',(21.7071386526689,16.4830954176967,-48.3903755582775));
#31148=CARTESIAN_POINT('Ctrl Pts',(21.7335478130473,16.4830954176946,-48.6675682080621));
#31149=CARTESIAN_POINT('Ctrl Pts',(21.9153131059641,16.2453260884688,-48.3475889909109));
#31150=CARTESIAN_POINT('Ctrl Pts',(21.911211102576,16.4830954176946,-48.4095570299751));
#31151=CARTESIAN_POINT('Ctrl Pts',(21.9460469728313,16.4830954176946,-48.6526097807597));
#31152=CARTESIAN_POINT('Ctrl Pts',(22.3039820967341,16.3195276817373,-48.3137123018963));
#31153=CARTESIAN_POINT('Ctrl Pts',(22.314923637338,16.4830954176946,-48.4038409245796));
#31154=CARTESIAN_POINT('Ctrl Pts',(22.3661671540024,16.4830954176946,-48.5848563887335));
#31155=CARTESIAN_POINT('Ctrl Pts',(22.4984290660376,16.3569498947425,-48.2880700344635));
#31156=CARTESIAN_POINT('Ctrl Pts',(22.5211470257103,16.4830954176957,-48.3840049109222));
#31157=CARTESIAN_POINT('Ctrl Pts',(22.5772011717386,16.4830954176946,-48.5333831751917));
#31158=CARTESIAN_POINT('Ctrl Pts',(22.6771142305796,16.3915662868148,-48.2427418189135));
#31159=CARTESIAN_POINT('Ctrl Pts',(22.7158795095401,16.4830954176946,-48.3256564433572));
#31160=CARTESIAN_POINT('Ctrl Pts',(22.7707018927952,16.4830954176946,-48.4429154297649));
#31161=CARTESIAN_POINT('Ctrl Pts',(22.6771142305791,16.3915662868147,-48.2427418189136));
#31162=CARTESIAN_POINT('Ctrl Pts',(22.6378911635743,16.3839676712799,-48.2526917941307));
#31163=CARTESIAN_POINT('Ctrl Pts',(22.5984148180719,16.3763319926651,-48.2615688372914));
#31164=CARTESIAN_POINT('Ctrl Pts',(22.558782775705,16.3686778876808,-48.2695704658023));
#31165=CARTESIAN_POINT('Ctrl Pts',(22.5150421675873,16.3602302986439,-48.2784016053575));
#31166=CARTESIAN_POINT('Ctrl Pts',(22.4711116392402,16.3517602066248,-48.286166399441));
#31167=CARTESIAN_POINT('Ctrl Pts',(22.4270762160408,16.3432839722952,-48.2930847735754));
#31168=CARTESIAN_POINT('Ctrl Pts',(22.3795404288295,16.3341339643659,-48.3005530874194));
#31169=CARTESIAN_POINT('Ctrl Pts',(22.3318815956323,16.3249766329787,-48.3070346785341));
#31170=CARTESIAN_POINT('Ctrl Pts',(22.2841643538499,16.3158247537669,-48.312759037465));
#31171=CARTESIAN_POINT('Ctrl Pts',(22.2260558231734,16.3046798880107,-48.3197299786618));
#31172=CARTESIAN_POINT('Ctrl Pts',(22.1678592205032,16.2935427876854,-48.325577982882));
#31173=CARTESIAN_POINT('Ctrl Pts',(22.1096477331681,16.2824290454295,-48.330651463777));
#31174=CARTESIAN_POINT('Ctrl Pts',(22.1068105242813,16.2818873652606,-48.3308987435793));
#31175=CARTESIAN_POINT('Ctrl Pts',(22.1039726872235,16.2813456246246,-48.3311440122853));
#31176=CARTESIAN_POINT('Ctrl Pts',(22.1011341818606,16.2808038159101,-48.3313872793092));
#31177=CARTESIAN_POINT('Ctrl Pts',(21.9836165992224,16.2583722745758,-48.3414588306834));
#31178=CARTESIAN_POINT('Ctrl Pts',(21.8658458886457,16.2359974207799,-48.3480286392735));
#31179=CARTESIAN_POINT('Ctrl Pts',(21.7478614729999,16.2136898071046,-48.3516402651633));
#31180=CARTESIAN_POINT('Ctrl Pts',(21.6717488808251,16.199299005635,-48.3539701509108));
#31181=CARTESIAN_POINT('Ctrl Pts',(21.5955470434192,16.1849361189663,-48.3550678012165));
#31182=CARTESIAN_POINT('Ctrl Pts',(21.5192635553992,16.1706033824536,-48.3550682079476));
#31183=CARTESIAN_POINT('Origin',(22.7707018927938,16.1705954176946,-48.4429154297618));
#31184=CARTESIAN_POINT('Ctrl Pts',(-21.2235932570288,16.4830953098781,-48.6660549524581));
#31185=CARTESIAN_POINT('Ctrl Pts',(-21.2332870627948,16.4833744495148,-48.3301033390522));
#31186=CARTESIAN_POINT('Ctrl Pts',(-21.2326795856286,16.1481826330634,-48.35418182094));
#31187=CARTESIAN_POINT('Ctrl Pts',(-21.4809214109692,16.483095324294,-48.6730692758819));
#31188=CARTESIAN_POINT('Ctrl Pts',(-21.4530298656609,16.483319828549,-48.3811888777417));
#31189=CARTESIAN_POINT('Ctrl Pts',(-21.4719110727632,16.1929802521112,-48.3576973104808));
#31190=CARTESIAN_POINT('Ctrl Pts',(-21.7374879541375,16.4830953387802,-48.6595262778593));
#31191=CARTESIAN_POINT('Ctrl Pts',(-21.7001920947721,16.483273583025,-48.4102189210674));
#31192=CARTESIAN_POINT('Ctrl Pts',(-21.7098307047766,16.2379895254129,-48.3509368618739));
#31193=CARTESIAN_POINT('Ctrl Pts',(-22.2406226301952,16.4830953673845,-48.5783465526032));
#31194=CARTESIAN_POINT('Ctrl Pts',(-22.1840696711221,16.4831976839894,-48.4033925316084));
#31195=CARTESIAN_POINT('Ctrl Pts',(-22.1752787584643,16.3268490737816,-48.3103713569693));
#31196=CARTESIAN_POINT('Ctrl Pts',(-22.4910901849638,16.4830953816853,-48.5139692904343));
#31197=CARTESIAN_POINT('Ctrl Pts',(-22.4296943202957,16.4831654080667,-48.377041868324));
#31198=CARTESIAN_POINT('Ctrl Pts',(-22.405734464261,16.3712675955696,-48.2783677938984));
#31199=CARTESIAN_POINT('Ctrl Pts',(-22.719770248326,16.4830953949244,-48.3828323956905));
#31200=CARTESIAN_POINT('Ctrl Pts',(-22.6621435906265,16.483138027882,-48.2869031393868));
#31201=CARTESIAN_POINT('Ctrl Pts',(-22.6173710027542,16.4123847430247,-48.2125473910278));
#31202=CARTESIAN_POINT('Origin',(-22.6036487560697,16.1705954176946,-48.4429154297618));
#31203=CARTESIAN_POINT('Ctrl Pts',(-21.3522103060312,16.1706033612892,-48.3550682079475));
#31204=CARTESIAN_POINT('Ctrl Pts',(-21.4500468132788,16.1889856471426,-48.3550676843655));
#31205=CARTESIAN_POINT('Ctrl Pts',(-21.547817703659,16.2074307865434,-48.3532530208503));
#31206=CARTESIAN_POINT('Ctrl Pts',(-21.6454352010438,16.2259200040857,-48.3493520545576));
#31207=CARTESIAN_POINT('Ctrl Pts',(-21.7419037370204,16.2441916028814,-48.3454970027766));
#31208=CARTESIAN_POINT('Ctrl Pts',(-21.8382231430226,16.2625063923369,-48.3396050349912));
#31209=CARTESIAN_POINT('Ctrl Pts',(-21.9342849222553,16.2808424439029,-48.3313696581645));
#31210=CARTESIAN_POINT('Ctrl Pts',(-21.937041977193,16.2813687042107,-48.3311332958306));
#31211=CARTESIAN_POINT('Ctrl Pts',(-21.9397986145587,16.2818949414479,-48.3308950166343));
#31212=CARTESIAN_POINT('Ctrl Pts',(-21.9425548449769,16.2824211576432,-48.3306548123709));
#31213=CARTESIAN_POINT('Ctrl Pts',(-22.0014746788088,16.2936700614286,-48.3255199748789));
#31214=CARTESIAN_POINT('Ctrl Pts',(-22.0603976620597,16.3049460203245,-48.3196239637247));
#31215=CARTESIAN_POINT('Ctrl Pts',(-22.1192165044416,16.3162274856631,-48.3125646537137));
#31216=CARTESIAN_POINT('Ctrl Pts',(-22.1732048838581,16.3265824672713,-48.3060850854009));
#31217=CARTESIAN_POINT('Ctrl Pts',(-22.2271060462257,16.3369421989594,-48.2986260138347));
#31218=CARTESIAN_POINT('Ctrl Pts',(-22.2808168332591,16.3472864072055,-48.2898397095524));
#31219=CARTESIAN_POINT('Ctrl Pts',(-22.3299129238807,16.3567418669654,-48.2818083025465));
#31220=CARTESIAN_POINT('Ctrl Pts',(-22.3788501680607,16.3661844046855,-48.2726681344544));
#31221=CARTESIAN_POINT('Ctrl Pts',(-22.4275274387716,16.3755943695789,-48.2621166834727));
#31222=CARTESIAN_POINT('Ctrl Pts',(-22.4551301771965,16.3809303466323,-48.2561334198839));
#31223=CARTESIAN_POINT('Ctrl Pts',(-22.4826488894981,16.3862557688533,-48.2496956543661));
#31224=CARTESIAN_POINT('Ctrl Pts',(-22.5100610938539,16.3915662868154,-48.2427418189112));
#31225=CARTESIAN_POINT('Ctrl Pts',(-23.0849210718625,16.8990456385831,-48.3550682080606));
#31226=CARTESIAN_POINT('Ctrl Pts',(-23.1434946548348,16.7639536069274,-48.3550682080606));
#31227=CARTESIAN_POINT('Ctrl Pts',(-23.1808194403678,16.6779610607098,-48.241518966339));
#31228=CARTESIAN_POINT('Ctrl Pts',(-19.9713351701806,15.5488264548572,-48.3550682080606));
#31229=CARTESIAN_POINT('Ctrl Pts',(-20.0384527840987,15.4217541149126,-48.3550682080606));
#31230=CARTESIAN_POINT('Ctrl Pts',(-20.0567638409257,15.3277344947597,-48.2465561452514));
#31231=CARTESIAN_POINT('Ctrl Pts',(-16.7812848361363,14.382877194386,-48.3550682080606));
#31232=CARTESIAN_POINT('Ctrl Pts',(-16.8373508296582,14.2535943294201,-48.3550682080606));
#31233=CARTESIAN_POINT('Ctrl Pts',(-16.8547673953945,14.1617844335495,-48.2513064297563));
#31234=CARTESIAN_POINT('Ctrl Pts',(-11.9276124411326,13.0662924545649,-48.3550682080606));
#31235=CARTESIAN_POINT('Ctrl Pts',(-11.962050470773,12.935869085436,-48.3550682080606));
#31236=CARTESIAN_POINT('Ctrl Pts',(-11.9812252105756,12.8452005633123,-48.2569136015784));
#31237=CARTESIAN_POINT('Ctrl Pts',(-10.3466638904053,12.7052707111053,-48.3550682080606));
#31238=CARTESIAN_POINT('Ctrl Pts',(-10.3762902134349,12.5748662546358,-48.3550682080606));
#31239=CARTESIAN_POINT('Ctrl Pts',(-10.3935551174996,12.4841786131398,-48.2584966737937));
#31240=CARTESIAN_POINT('Ctrl Pts',(-6.98178065400343,12.0967706273038,-48.3550682080606));
#31241=CARTESIAN_POINT('Ctrl Pts',(-7.00312169292105,11.9671239022574,-48.3550682080606));
#31242=CARTESIAN_POINT('Ctrl Pts',(-7.01396478862274,11.8756772034364,-48.2612025886206));
#31243=CARTESIAN_POINT('Ctrl Pts',(-5.19039787585605,11.86730628845,-48.3550682080606));
#31244=CARTESIAN_POINT('Ctrl Pts',(-5.20558538253443,11.7375302402796,-48.3550682080606));
#31245=CARTESIAN_POINT('Ctrl Pts',(-5.21452165327191,11.6462129991553,-48.2622498619779));
#31246=CARTESIAN_POINT('Ctrl Pts',(-3.39047527149618,11.7377723175973,-48.3550682080606));
#31247=CARTESIAN_POINT('Ctrl Pts',(-3.39980751503421,11.608092893254,-48.3550682080606));
#31248=CARTESIAN_POINT('Ctrl Pts',(-3.40639346140351,11.5166787176219,-48.2628417377604));
#31249=CARTESIAN_POINT('Ctrl Pts',(22.9214777263312,16.4951170325608,-48.2422982426787));
#31250=CARTESIAN_POINT('Ctrl Pts',(22.8846548346438,16.581294328644,-48.3550682080606));
#31251=CARTESIAN_POINT('Ctrl Pts',(22.8270439774155,16.7161293233258,-48.3550682080606));
#31252=CARTESIAN_POINT('Ctrl Pts',(19.9326035269438,15.2224248692786,-48.2470767173395));
#31253=CARTESIAN_POINT('Ctrl Pts',(19.9130757495238,15.3157731473117,-48.3550682080606));
#31254=CARTESIAN_POINT('Ctrl Pts',(19.8482783897377,15.4434377872993,-48.3550682080606));
#31255=CARTESIAN_POINT('Ctrl Pts',(16.8711181780395,14.121138883407,-48.2515673091557));
#31256=CARTESIAN_POINT('Ctrl Pts',(16.8528533641736,14.2126904008502,-48.3550682080606));
#31257=CARTESIAN_POINT('Ctrl Pts',(16.7982643163788,14.3421540062504,-48.3550682080606));
#31258=CARTESIAN_POINT('Ctrl Pts',(12.1478906017067,12.8451845281753,-48.2569973005878));
#31259=CARTESIAN_POINT('Ctrl Pts',(12.1287157575068,12.9358419174557,-48.3550682080606));
#31260=CARTESIAN_POINT('Ctrl Pts',(12.0942956535457,13.066199446441,-48.3550682080606));
#31261=CARTESIAN_POINT('Ctrl Pts',(10.5602837555011,12.484193948824,-48.2585790241695));
#31262=CARTESIAN_POINT('Ctrl Pts',(10.5430188516445,12.5748700381595,-48.3550682080606));
#31263=CARTESIAN_POINT('Ctrl Pts',(10.5134085414344,12.7052089420493,-48.3550682080606));
#31264=CARTESIAN_POINT('Ctrl Pts',(7.33455208025131,11.9034070992466,-48.2611597032935));
#31265=CARTESIAN_POINT('Ctrl Pts',(7.32304238738767,11.9947391319378,-48.3550682080606));
#31266=CARTESIAN_POINT('Ctrl Pts',(7.30170908809363,12.1244225199508,-48.3550682080606));
#31267=CARTESIAN_POINT('Ctrl Pts',(5.69014026513413,11.6863324002422,-48.2621466998951));
#31268=CARTESIAN_POINT('Ctrl Pts',(5.68056395331838,11.7776141662045,-48.3550682080606));
#31269=CARTESIAN_POINT('Ctrl Pts',(5.66464372163471,11.9073477694537,-48.3550682080606));
#31270=CARTESIAN_POINT('Ctrl Pts',(4.03844270956242,11.5522837221933,-48.2627582883049));
#31271=CARTESIAN_POINT('Ctrl Pts',(4.03099382678731,11.6436417585081,-48.3550682080606));
#31272=CARTESIAN_POINT('Ctrl Pts',(4.02042267392571,11.7732992288254,-48.3550682080606));
#31273=CARTESIAN_POINT('Ctrl Pts',(4.30427685533896,11.5746245485739,-48.2627017315157));
#31274=CARTESIAN_POINT('Ctrl Pts',(4.30071410004375,11.5746245276893,-48.2630127553113));
#31275=CARTESIAN_POINT('Ctrl Pts',(4.29866044559197,11.5884292819489,-48.2774220038378));
#31276=CARTESIAN_POINT('Ctrl Pts',(4.29524068288583,11.6268390447666,-48.3065330737687));
#31277=CARTESIAN_POINT('Ctrl Pts',(4.29388242493259,11.651680100407,-48.3210576919341));
#31278=CARTESIAN_POINT('Ctrl Pts',(4.29256572521535,11.6756605207397,-48.3310538583792));
#31279=CARTESIAN_POINT('Origin',(0.0835265683620477,16.1705954176946,0.0824317919394229));
#31280=CARTESIAN_POINT('Origin',(48.6088737900633,16.1705954176946,-22.6047435324922));
#31281=CARTESIAN_POINT('Origin',(48.8335265683622,16.1705954176946,-44.2925682080603));
#31282=CARTESIAN_POINT('Origin',(48.833526568362,16.1705954176946,21.5181263879131));
#31283=CARTESIAN_POINT('Origin',(48.8335265683621,16.1705954176946,-21.353262804034));
#31284=CARTESIAN_POINT('Origin',(0.0835265683620477,16.1705954176946,0.0824317919394229));
#31285=CARTESIAN_POINT('Origin',(-48.4418206533391,16.1705954176946,-22.6047435324924));
#31286=CARTESIAN_POINT('Ctrl Pts',(0.0835265683594526,11.4728541727075,
-48.3550824830876));
#31287=CARTESIAN_POINT('Ctrl Pts',(0.434571873647755,11.4781922148201,-48.3550825994612));
#31288=CARTESIAN_POINT('Ctrl Pts',(0.785441203021056,11.4874426767152,-48.3536254076401));
#31289=CARTESIAN_POINT('Ctrl Pts',(1.48685396298274,11.5143737377389,-48.3502977991207));
#31290=CARTESIAN_POINT('Ctrl Pts',(1.83739739357112,11.5320543368675,-48.3484273824224));
#31291=CARTESIAN_POINT('Ctrl Pts',(2.88857791672651,11.5986492866067,-48.3459483822799));
#31292=CARTESIAN_POINT('Ctrl Pts',(3.59085027388967,11.6392592214936,-48.3412545192878));
#31293=CARTESIAN_POINT('Ctrl Pts',(4.29256572521535,11.6756605207398,-48.3310538583792));
#31294=CARTESIAN_POINT('Ctrl Pts',(0.43457187364779,11.467516130595,-48.3550823667143));
#31295=CARTESIAN_POINT('Ctrl Pts',(0.707588293928371,11.4749860898031,-48.3541407510376));
#31296=CARTESIAN_POINT('Ctrl Pts',(0.998330962585111,11.4844803122479,-48.3524253715956));
#31297=CARTESIAN_POINT('Ctrl Pts',(1.61221600331842,11.5105174196337,-48.3485410607123));
#31298=CARTESIAN_POINT('Ctrl Pts',(1.93535675582816,11.5270830007415,-48.3463749782919));
#31299=CARTESIAN_POINT('Ctrl Pts',(2.94880362400346,11.5919036248635,-48.3427355509074));
#31300=CARTESIAN_POINT('Ctrl Pts',(3.62682139903089,11.6298708101947,-48.3372561068183));
#31301=CARTESIAN_POINT('Ctrl Pts',(4.29322407507397,11.6636703105734,-48.3260557751567));
#31302=CARTESIAN_POINT('Ctrl Pts',(0.785669116593031,11.4659265087692,-48.353624938571));
#31303=CARTESIAN_POINT('Ctrl Pts',(0.998676156491118,11.4745419834779,-48.352053093827));
#31304=CARTESIAN_POINT('Ctrl Pts',(1.24336152271037,11.4840908039497,-48.3500372977499));
#31305=CARTESIAN_POINT('Ctrl Pts',(1.78640027440588,11.5090816899177,-48.3454511925554));
#31306=CARTESIAN_POINT('Ctrl Pts',(2.08475123053189,11.5245577996643,-48.3428851569693));
#31307=CARTESIAN_POINT('Ctrl Pts',(3.04577954599007,11.5859418512174,-48.3377026419571));
#31308=CARTESIAN_POINT('Ctrl Pts',(3.68879009429774,11.6209827896584,-48.3313642361181));
#31309=CARTESIAN_POINT('Ctrl Pts',(4.29389281449159,11.6514649415801,-48.3199255790041));
#31310=CARTESIAN_POINT('Ctrl Pts',(1.48799468014872,11.4643966328772,-48.3438941182188));
#31311=CARTESIAN_POINT('Ctrl Pts',(1.61377824696731,11.4744825705815,-48.3421773991261));
#31312=CARTESIAN_POINT('Ctrl Pts',(1.78770682158171,11.4843329006934,-48.340137776651));
#31313=CARTESIAN_POINT('Ctrl Pts',(2.21034412030734,11.5079260458425,-48.3350871090452));
#31314=CARTESIAN_POINT('Ctrl Pts',(2.45904980773078,11.5217114161925,-48.3320814058289));
#31315=CARTESIAN_POINT('Ctrl Pts',(3.2850802554449,11.5755468354576,-48.3246778344458));
#31316=CARTESIAN_POINT('Ctrl Pts',(3.83438595516491,11.6050189470212,-48.3171415021045));
#31317=CARTESIAN_POINT('Ctrl Pts',(4.29532858873579,11.6282480883245,-48.3065253445687));
#31318=CARTESIAN_POINT('Ctrl Pts',(1.83922300075916,11.4644563788109,-48.3356207260099));
#31319=CARTESIAN_POINT('Ctrl Pts',(1.93779750981832,11.4748353413218,-48.3343702273184));
#31320=CARTESIAN_POINT('Ctrl Pts',(2.08702911273414,11.4849166217024,-48.3325976279216));
#31321=CARTESIAN_POINT('Ctrl Pts',(2.4601131356293,11.508146276442,-48.3277770168468));
#31322=CARTESIAN_POINT('Ctrl Pts',(2.68396272136668,11.5213343690929,-48.3247339909556));
#31323=CARTESIAN_POINT('Ctrl Pts',(3.4274100778507,11.5710816706554,-48.3166668015675));
#31324=CARTESIAN_POINT('Ctrl Pts',(3.91801312076524,11.5979431249203,-48.308810638791));
#31325=CARTESIAN_POINT('Ctrl Pts',(4.29609562356237,11.6172366040622,-48.299255306286));
#31326=CARTESIAN_POINT('Ctrl Pts',(2.8931453826154,11.4583384590298,-48.2947245924959));
#31327=CARTESIAN_POINT('Ctrl Pts',(2.95442665337013,11.4700074930205,-48.2942918711471));
#31328=CARTESIAN_POINT('Ctrl Pts',(3.05143599905993,11.4818828006791,-48.2936814855085));
#31329=CARTESIAN_POINT('Ctrl Pts',(3.2896917488815,11.5065304546877,-48.2916809761507));
#31330=CARTESIAN_POINT('Ctrl Pts',(3.43093653344645,11.5193254972046,-48.2902937014525));
#31331=CARTESIAN_POINT('Ctrl Pts',(3.88020208317704,11.5598336028455,-48.2862238405637));
#31332=CARTESIAN_POINT('Ctrl Pts',(4.15587731818982,11.5806510816358,-48.2821814457028));
#31333=CARTESIAN_POINT('Ctrl Pts',(4.29866044559197,11.5884292819489,-48.2774220038378));
#31334=CARTESIAN_POINT('Ctrl Pts',(3.59439815510631,11.4609474762041,-48.2515240163507));
#31335=CARTESIAN_POINT('Ctrl Pts',(3.63137389790745,11.4731609516943,-48.2527720831628));
#31336=CARTESIAN_POINT('Ctrl Pts',(3.69355131246284,11.4863352799677,-48.2541165047803));
#31337=CARTESIAN_POINT('Ctrl Pts',(3.83871344717961,11.5121367174564,-48.256744523456));
#31338=CARTESIAN_POINT('Ctrl Pts',(3.921698167341,11.5247638266717,-48.2580281205142));
#31339=CARTESIAN_POINT('Ctrl Pts',(4.15746922938038,11.5581209387927,-48.2614073735947));
#31340=CARTESIAN_POINT('Ctrl Pts',(4.2970724728136,11.5743267261738,-48.2630314915227));
#31341=CARTESIAN_POINT('Ctrl Pts',(4.30071410004375,11.5746245276893,-48.2630127553113));
#31342=CARTESIAN_POINT('Ctrl Pts',(4.29550794738005,11.4732422824942,-48.1954680629781));
#31343=CARTESIAN_POINT('Ctrl Pts',(4.29556063460006,11.4851966459098,-48.200433936555));
#31344=CARTESIAN_POINT('Ctrl Pts',(4.29569371583995,11.4974720069511,-48.2071191491468));
#31345=CARTESIAN_POINT('Ctrl Pts',(4.29625434599591,11.5208685373805,-48.221588093388));
#31346=CARTESIAN_POINT('Ctrl Pts',(4.29668189491196,11.5319897067687,-48.2293718250376));
#31347=CARTESIAN_POINT('Ctrl Pts',(4.29860676262893,11.5609276470972,-48.2508605601154));
#31348=CARTESIAN_POINT('Ctrl Pts',(4.30074630239865,11.5743188502015,-48.2627031036729));
#31349=CARTESIAN_POINT('Ctrl Pts',(4.30427685533896,11.5746245485739,-48.2627017315157));
#31350=CARTESIAN_POINT('Ctrl Pts',(4.30427685447981,11.5746245484995,-48.2627017315161));
#31351=CARTESIAN_POINT('Ctrl Pts',(4.30406730074831,11.5746064038392,-48.2627018128455));
#31352=CARTESIAN_POINT('Ctrl Pts',(4.30391112003706,11.574549785394,-48.2626633000481));
#31353=CARTESIAN_POINT('Ctrl Pts',(4.30379489777073,11.5744984448496,-48.2626265378358));
#31354=CARTESIAN_POINT('Ctrl Pts',(4.30367838955579,11.5744469779889,-48.2625896851753));
#31355=CARTESIAN_POINT('Ctrl Pts',(4.30360215028203,11.5743997047815,-48.2625535320247));
#31356=CARTESIAN_POINT('Ctrl Pts',(4.30355585183876,11.5743705526458,-48.262531196277));
#31357=CARTESIAN_POINT('Ctrl Pts',(4.30346336852036,11.5743123198834,-48.2624865795701));
#31358=CARTESIAN_POINT('Ctrl Pts',(4.30341313104675,11.5742733795723,-48.2624559072521));
#31359=CARTESIAN_POINT('Ctrl Pts',(4.30336529688495,11.5742358022889,-48.26242627286));
#31360=CARTESIAN_POINT('Ctrl Pts',(4.30326962856134,11.5741606477221,-48.2623670040757));
#31361=CARTESIAN_POINT('Ctrl Pts',(4.30319991820999,11.5740963865912,-48.2623154901695));
#31362=CARTESIAN_POINT('Ctrl Pts',(4.30313175144365,11.574029268754,-48.2622613949826));
#31363=CARTESIAN_POINT('Ctrl Pts',(4.30289813112297,11.5737992433104,-48.2620760006094));
#31364=CARTESIAN_POINT('Ctrl Pts',(4.3027074795769,11.573544153445,-48.2618660736616));
#31365=CARTESIAN_POINT('Ctrl Pts',(4.30254169594019,11.5732903201701,-48.261656181311));
#31366=CARTESIAN_POINT('Ctrl Pts',(4.3023183694699,11.5729483823864,-48.2613734361696));
#31367=CARTESIAN_POINT('Ctrl Pts',(4.30213864866023,11.5726061687533,-48.2610884915831));
#31368=CARTESIAN_POINT('Ctrl Pts',(4.30197216232291,11.5722518188883,-48.2607931815174));
#31369=CARTESIAN_POINT('Ctrl Pts',(4.30174482657617,11.5717679570144,-48.2603899380116));
#31370=CARTESIAN_POINT('Ctrl Pts',(4.30155414381932,11.5712800182779,-48.2599826422918));
#31371=CARTESIAN_POINT('Ctrl Pts',(4.30138186491148,11.5707911792801,-48.2595751390173));
#31372=CARTESIAN_POINT('Ctrl Pts',(4.30108725143153,11.5699552176404,-48.2588782692768));
#31373=CARTESIAN_POINT('Ctrl Pts',(4.30084610919985,11.5691127678859,-48.2581774873085));
#31374=CARTESIAN_POINT('Ctrl Pts',(4.30063043411004,11.5682688436763,-48.2574784824322));
#31375=CARTESIAN_POINT('Ctrl Pts',(4.30026642622229,11.566844501768,-48.256298729644));
#31376=CARTESIAN_POINT('Ctrl Pts',(4.29997599910921,11.5654127733926,-48.2551211964302));
#31377=CARTESIAN_POINT('Ctrl Pts',(4.29971880605547,11.5639752439749,-48.2539487703289));
#31378=CARTESIAN_POINT('Ctrl Pts',(4.29931853639503,11.5617380163222,-48.2521241230817));
#31379=CARTESIAN_POINT('Ctrl Pts',(4.29900214095316,11.5594864489408,-48.2503113515096));
#31380=CARTESIAN_POINT('Ctrl Pts',(4.29872534939056,11.5572216878539,-48.2485130362479));
#31381=CARTESIAN_POINT('Ctrl Pts',(4.29830910660352,11.5538159103875,-48.2458087061396));
#31382=CARTESIAN_POINT('Ctrl Pts',(4.29798570586486,11.5503795187906,-48.2431361939227));
#31383=CARTESIAN_POINT('Ctrl Pts',(4.29770861623514,11.5469146456565,-48.2405017858792));
#31384=CARTESIAN_POINT('Ctrl Pts',(4.29756852994005,11.5451629336172,-48.2391699263543));
#31385=CARTESIAN_POINT('Ctrl Pts',(4.29744108789414,11.5434032086018,-48.2378472629719));
#31386=CARTESIAN_POINT('Ctrl Pts',(4.29732351748428,11.5416356868782,-48.2365347367302));
#31387=CARTESIAN_POINT('Ctrl Pts',(4.29694599926989,11.5359601802111,-48.2323202191171));
#31388=CARTESIAN_POINT('Ctrl Pts',(4.29666691876312,11.5302068971307,-48.228210625839));
#31389=CARTESIAN_POINT('Ctrl Pts',(4.29644147322476,11.5243619443827,-48.2242324297731));
#31390=CARTESIAN_POINT('Ctrl Pts',(4.29624888339644,11.519368816311,-48.2208340032489));
#31391=CARTESIAN_POINT('Ctrl Pts',(4.29609717557184,11.5143094135622,-48.2175317826848));
#31392=CARTESIAN_POINT('Ctrl Pts',(4.29597403091793,11.5091702721658,-48.2143536212674));
#31393=CARTESIAN_POINT('Ctrl Pts',(4.29584159356509,11.5036433226738,-48.2109356305416));
#31394=CARTESIAN_POINT('Ctrl Pts',(4.29574246556238,11.4980242335258,-48.2076595865044));
#31395=CARTESIAN_POINT('Ctrl Pts',(4.29566813462061,11.4922875984294,-48.2045854548351));
#31396=CARTESIAN_POINT('Ctrl Pts',(4.29560429163279,11.4873603915918,-48.2019450772747));
#31397=CARTESIAN_POINT('Ctrl Pts',(4.29555890131979,11.4823456579696,-48.1994525269835));
#31398=CARTESIAN_POINT('Ctrl Pts',(4.29552851076737,11.4772262324437,-48.1971803260925));
#31399=CARTESIAN_POINT('Ctrl Pts',(4.29552351828933,11.4763852270169,-48.1968070550545));
#31400=CARTESIAN_POINT('Ctrl Pts',(4.29551893289638,11.4755414144694,-48.1964398420676));
#31401=CARTESIAN_POINT('Ctrl Pts',(4.2955147414803,11.4746947555587,-48.196079159465));
#31402=CARTESIAN_POINT('Ctrl Pts',(4.29551234923451,11.4742115259827,-48.1958733002944));
#31403=CARTESIAN_POINT('Ctrl Pts',(4.29551008533479,11.4737273695405,-48.1956695693956));
#31404=CARTESIAN_POINT('Ctrl Pts',(4.29550794738005,11.4732422824942,-48.1954680629781));
#31405=CARTESIAN_POINT('Ctrl Pts',(48.8335265683621,16.4830954176946,-21.353262804034));
#31406=CARTESIAN_POINT('Ctrl Pts',(48.5210265683622,16.4830954176946,-21.353262804034));
#31407=CARTESIAN_POINT('Ctrl Pts',(48.5210265683621,16.1705954176947,-21.353262804034));
#31408=CARTESIAN_POINT('Ctrl Pts',(48.8335265706117,16.4830954176946,-21.5676091116417));
#31409=CARTESIAN_POINT('Ctrl Pts',(48.5563370700187,16.4830954176946,-21.54119704969));
#31410=CARTESIAN_POINT('Ctrl Pts',(48.5210265683621,16.2080086375453,-21.5523883700179));
#31411=CARTESIAN_POINT('Ctrl Pts',(48.8183477161632,16.4830954176946,-21.7820280540439));
#31412=CARTESIAN_POINT('Ctrl Pts',(48.5755877658885,16.4830954176946,-21.7471528982396));
#31413=CARTESIAN_POINT('Ctrl Pts',(48.5134371390849,16.2456676717398,-21.7511508011048));
#31414=CARTESIAN_POINT('Ctrl Pts',(48.7505672098116,16.4830954176946,-22.2011670980052));
#31415=CARTESIAN_POINT('Ctrl Pts',(48.5696939191561,16.4830954176946,-22.1499363086026));
#31416=CARTESIAN_POINT('Ctrl Pts',(48.4795468922649,16.319697904787,-22.1389084821703));
#31417=CARTESIAN_POINT('Ctrl Pts',(48.7009182366022,16.4830954176946,-22.407870378551));
#31418=CARTESIAN_POINT('Ctrl Pts',(48.5510364183067,16.4830954176946,-22.3516070845003));
#31419=CARTESIAN_POINT('Ctrl Pts',(48.4548516611731,16.3563211717407,-22.3292253454905));
#31420=CARTESIAN_POINT('Ctrl Pts',(48.6088737900635,16.4830954176946,-22.6047435324922));
#31421=CARTESIAN_POINT('Ctrl Pts',(48.4916148036563,16.4830954176946,-22.5499211492369));
#31422=CARTESIAN_POINT('Ctrl Pts',(48.4087001792128,16.3915662868154,-22.5111558702763));
#31423=CARTESIAN_POINT('Ctrl Pts',(48.5210265682481,16.1706033612914,-21.3533050824651));
#31424=CARTESIAN_POINT('Ctrl Pts',(48.5210260905822,16.1872388804039,-21.4418447279119));
#31425=CARTESIAN_POINT('Ctrl Pts',(48.5195289950699,16.2039304589262,-21.5303529580501));
#31426=CARTESIAN_POINT('Ctrl Pts',(48.5163532494991,16.2206573802635,-21.6187323309531));
#31427=CARTESIAN_POINT('Ctrl Pts',(48.5134900262187,16.2357382201841,-21.6984143685593));
#31428=CARTESIAN_POINT('Ctrl Pts',(48.509262165005,16.2508479929972,-21.7779925874712));
#31429=CARTESIAN_POINT('Ctrl Pts',(48.5034990985229,16.2659683787707,-21.8573738795946));
#31430=CARTESIAN_POINT('Ctrl Pts',(48.5015994066349,16.270952543761,-21.8835405041115));
#31431=CARTESIAN_POINT('Ctrl Pts',(48.499532585912,16.275937822519,-21.9096854870959));
#31432=CARTESIAN_POINT('Ctrl Pts',(48.4972915416398,16.2809234207259,-21.9358046625462));
#31433=CARTESIAN_POINT('Ctrl Pts',(48.4970276525395,16.2815104885682,-21.9388802669846));
#31434=CARTESIAN_POINT('Ctrl Pts',(48.4967613650824,16.2820975177296,-21.9419552962478));
#31435=CARTESIAN_POINT('Ctrl Pts',(48.4964926678709,16.2826845076336,-21.9450297471065));
#31436=CARTESIAN_POINT('Ctrl Pts',(48.4911785363218,16.2942936402729,-22.0058343837204));
#31437=CARTESIAN_POINT('Ctrl Pts',(48.4850832026772,16.3059124438886,-22.066544098701));
#31438=CARTESIAN_POINT('Ctrl Pts',(48.4777339713189,16.3175327023971,-22.1271197666865));
#31439=CARTESIAN_POINT('Ctrl Pts',(48.4708550229911,16.3284093715259,-22.1838191505642));
#31440=CARTESIAN_POINT('Ctrl Pts',(48.4628780808606,16.339287358577,-22.2404012791344));
#31441=CARTESIAN_POINT('Ctrl Pts',(48.453373849129,16.3501570443392,-22.2968182791175));
#31442=CARTESIAN_POINT('Ctrl Pts',(48.4445365333712,16.3602639996386,-22.34927647427));
#31443=CARTESIAN_POINT('Ctrl Pts',(48.4343790058226,16.3703637977871,-22.4015919817819));
#31444=CARTESIAN_POINT('Ctrl Pts',(48.4225135354583,16.3804457145562,-22.4537104745914));
#31445=CARTESIAN_POINT('Ctrl Pts',(48.4181477680927,16.3841552432864,-22.4728868922186));
#31446=CARTESIAN_POINT('Ctrl Pts',(48.4135503242605,16.3878623190466,-22.4920364694703));
#31447=CARTESIAN_POINT('Ctrl Pts',(48.4087001792128,16.3915662868154,-22.5111558702763));
#31448=CARTESIAN_POINT('Ctrl Pts',(48.521026568362,16.1705954176947,21.5181263879131));
#31449=CARTESIAN_POINT('Ctrl Pts',(48.521026568362,16.4830954176946,21.5181263879131));
#31450=CARTESIAN_POINT('Ctrl Pts',(48.833526568362,16.4830954176946,21.5181263879131));
#31451=CARTESIAN_POINT('Ctrl Pts',(48.521026568362,16.2080322538905,21.7173776481921));
#31452=CARTESIAN_POINT('Ctrl Pts',(48.5563586162256,16.4830954176918,21.7061753278482));
#31453=CARTESIAN_POINT('Ctrl Pts',(48.833526568103,16.4830954176946,21.7326096831721));
#31454=CARTESIAN_POINT('Ctrl Pts',(48.5135293069769,16.2453207379311,21.9141872379789));
#31455=CARTESIAN_POINT('Ctrl Pts',(48.5754705520278,16.4830954176946,21.9101416977376));
#31456=CARTESIAN_POINT('Ctrl Pts',(48.8185320523741,16.4830954176946,21.9449194637153));
#31457=CARTESIAN_POINT('Ctrl Pts',(48.4797929446078,16.3193045764618,22.3017217477063));
#31458=CARTESIAN_POINT('Ctrl Pts',(48.5698564439212,16.4830954176946,22.3126619379227));
#31459=CARTESIAN_POINT('Ctrl Pts',(48.7510593140707,16.4830954176946,22.3638116144414));
#31460=CARTESIAN_POINT('Ctrl Pts',(48.4548701098381,16.3563070925481,22.4940162271868));
#31461=CARTESIAN_POINT('Ctrl Pts',(48.5510669794482,16.483095417693,22.5163687361117));
#31462=CARTESIAN_POINT('Ctrl Pts',(48.700968878949,16.4830954176946,22.5726256902424));
#31463=CARTESIAN_POINT('Ctrl Pts',(48.4087001792127,16.3915662868154,22.6760194541556));
#31464=CARTESIAN_POINT('Ctrl Pts',(48.4916148036562,16.4830954176946,22.7147847331162));
#31465=CARTESIAN_POINT('Ctrl Pts',(48.6088737900633,16.4830954176946,22.7696071163714));
#31466=CARTESIAN_POINT('Ctrl Pts',(48.4087001792127,16.3915662868154,22.6760194541555));
#31467=CARTESIAN_POINT('Ctrl Pts',(48.4215041465258,16.3817881293016,22.6255458743838));
#31468=CARTESIAN_POINT('Ctrl Pts',(48.4325629456394,16.3719647253873,22.5747387277194));
#31469=CARTESIAN_POINT('Ctrl Pts',(48.442243951573,16.3621195256861,22.5237189880492));
#31470=CARTESIAN_POINT('Ctrl Pts',(48.4524806610765,16.351709197458,22.4697706424398));
#31471=CARTESIAN_POINT('Ctrl Pts',(48.4611763864365,16.3412744261774,22.4155842444699));
#31472=CARTESIAN_POINT('Ctrl Pts',(48.4687118641718,16.3308372397184,22.3612726664185));
#31473=CARTESIAN_POINT('Ctrl Pts',(48.4771655296529,16.3191282962395,22.3003432962141));
#31474=CARTESIAN_POINT('Ctrl Pts',(48.4841586198759,16.3074162297974,22.239256014571));
#31475=CARTESIAN_POINT('Ctrl Pts',(48.4901689987576,16.2957263502233,22.1781386555071));
#31476=CARTESIAN_POINT('Ctrl Pts',(48.4924694182924,16.2912521518638,22.1547465250811));
#31477=CARTESIAN_POINT('Ctrl Pts',(48.4946253459155,16.2867811561769,22.1313497223861));
#31478=CARTESIAN_POINT('Ctrl Pts',(48.4966618765561,16.2823146437397,22.1079546137713));
#31479=CARTESIAN_POINT('Ctrl Pts',(48.49689257277,16.2818086815469,22.1053044385793));
#31480=CARTESIAN_POINT('Ctrl Pts',(48.4971214898655,16.2813027193741,22.1026539911944));
#31481=CARTESIAN_POINT('Ctrl Pts',(48.4973486349728,16.2807967549782,22.1000032598185));
#31482=CARTESIAN_POINT('Ctrl Pts',(48.5070811654924,16.2591176002569,21.9864268578278));
#31483=CARTESIAN_POINT('Ctrl Pts',(48.5135451570134,16.2374836515957,21.872573572219));
#31484=CARTESIAN_POINT('Ctrl Pts',(48.5172287291613,16.2159059273928,21.7584858701599));
#31485=CARTESIAN_POINT('Ctrl Pts',(48.5198114921994,16.2007765512654,21.6784924593757));
#31486=CARTESIAN_POINT('Ctrl Pts',(48.5210261401518,16.1856747351528,21.5983834228076));
#31487=CARTESIAN_POINT('Ctrl Pts',(48.5210265682489,16.1706033824536,21.518168778977));
#31488=CARTESIAN_POINT('Origin',(48.6088737900632,16.1705954176946,22.7696071163714));
#31489=CARTESIAN_POINT('Ctrl Pts',(-48.3539734316379,16.1705954176947,-21.3532628040341));
#31490=CARTESIAN_POINT('Ctrl Pts',(-48.353973431638,16.4830954176946,-21.3532628040341));
#31491=CARTESIAN_POINT('Ctrl Pts',(-48.6664734316379,16.4830954176946,-21.3532628040341));
#31492=CARTESIAN_POINT('Ctrl Pts',(-48.3539734316379,16.2080105885521,-21.5523987534991));
#31493=CARTESIAN_POINT('Ctrl Pts',(-48.3892858729637,16.4830954176974,-21.5412073890877));
#31494=CARTESIAN_POINT('Ctrl Pts',(-48.6664734316171,16.4830954176946,-21.5676219963864));
#31495=CARTESIAN_POINT('Ctrl Pts',(-48.3464913697085,16.2453321156391,-21.7493863021592));
#31496=CARTESIAN_POINT('Ctrl Pts',(-48.4084615410216,16.483095417695,-21.7452887921056));
#31497=CARTESIAN_POINT('Ctrl Pts',(-48.6515093147605,16.4830954176946,-21.7801227265566));
#31498=CARTESIAN_POINT('Ctrl Pts',(-48.3126208434,16.3195206182106,-22.137986751486));
#31499=CARTESIAN_POINT('Ctrl Pts',(-48.4027468354045,16.4830954176942,-22.1489298171496));
#31500=CARTESIAN_POINT('Ctrl Pts',(-48.5837682481807,16.4830954176946,-22.2001688119519));
#31501=CARTESIAN_POINT('Ctrl Pts',(-48.2869930772645,16.3569362864368,-22.3324004616851));
#31502=CARTESIAN_POINT('Ctrl Pts',(-48.3829333544402,16.4830954176958,-22.355111170887));
#31503=CARTESIAN_POINT('Ctrl Pts',(-48.5323224387334,16.4830954176946,-22.4111700033582));
#31504=CARTESIAN_POINT('Ctrl Pts',(-48.241647042494,16.391566286814,-22.5111558702805));
#31505=CARTESIAN_POINT('Ctrl Pts',(-48.324561666938,16.4830954176946,-22.5499211492407));
#31506=CARTESIAN_POINT('Ctrl Pts',(-48.4418206533465,16.4830954176946,-22.6047435324958));
#31507=CARTESIAN_POINT('Origin',(-48.6664734316379,16.1705954176946,-21.3532628040342));
#31508=CARTESIAN_POINT('Ctrl Pts',(-48.2416470424944,16.3915662868137,-22.511155870279));
#31509=CARTESIAN_POINT('Ctrl Pts',(-48.2516296638352,16.3839427400264,-22.4718041113854));
#31510=CARTESIAN_POINT('Ctrl Pts',(-48.260532619053,16.3762820912579,-22.4321984891174));
#31511=CARTESIAN_POINT('Ctrl Pts',(-48.2685549114895,16.3686030213912,-22.3924368065077));
#31512=CARTESIAN_POINT('Ctrl Pts',(-48.2774078505434,16.3601288429616,-22.3485581077925));
#31513=CARTESIAN_POINT('Ctrl Pts',(-48.285188292822,16.3516321729391,-22.3044890886349));
#31514=CARTESIAN_POINT('Ctrl Pts',(-48.2921179089163,16.343129468787,-22.2603152652558));
#31515=CARTESIAN_POINT('Ctrl Pts',(-48.2995987350645,16.3339504247122,-22.2126276749908));
#31516=CARTESIAN_POINT('Ctrl Pts',(-48.3060875995565,16.3247641828062,-22.1648171335444));
#31517=CARTESIAN_POINT('Ctrl Pts',(-48.3118160984604,16.315583691338,-22.1169491583698));
#31518=CARTESIAN_POINT('Ctrl Pts',(-48.3187204578189,16.3045187660849,-22.0592555622088));
#31519=CARTESIAN_POINT('Ctrl Pts',(-48.3245201692789,16.2934618759648,-22.0014770742633));
#31520=CARTESIAN_POINT('Ctrl Pts',(-48.3295569233971,16.2824285258603,-21.9436866585553));
#31521=CARTESIAN_POINT('Ctrl Pts',(-48.329804419995,16.2818863678454,-21.9408469465223));
#31522=CARTESIAN_POINT('Ctrl Pts',(-48.3300499019331,16.2813441490099,-21.9380066039067));
#31523=CARTESIAN_POINT('Ctrl Pts',(-48.3302933786148,16.2808018618168,-21.9351655909642));
#31524=CARTESIAN_POINT('Ctrl Pts',(-48.3403316897726,16.2584438785268,-21.8180333394403));
#31525=CARTESIAN_POINT('Ctrl Pts',(-48.3468913580189,16.2361414811697,-21.7006457858735));
#31526=CARTESIAN_POINT('Ctrl Pts',(-48.3505104144184,16.2139052642594,-21.5830426396001));
#31527=CARTESIAN_POINT('Ctrl Pts',(-48.3528642839503,16.1994426122,-21.5065524078089));
#31528=CARTESIAN_POINT('Ctrl Pts',(-48.353973022726,16.1850078872687,-21.4299706573745));
#31529=CARTESIAN_POINT('Ctrl Pts',(-48.3539734315249,16.1706033824528,-21.353305195093));
#31530=CARTESIAN_POINT('Ctrl Pts',(-48.2412034662232,16.4951170400788,-22.7555193836954));
#31531=CARTESIAN_POINT('Ctrl Pts',(-48.353973431638,16.5812943361539,-22.718696491988));
#31532=CARTESIAN_POINT('Ctrl Pts',(-48.353973431638,16.716129330846,-22.6610856347191));
#31533=CARTESIAN_POINT('Ctrl Pts',(-48.245981940911,15.222424873626,-19.7666451786995));
#31534=CARTESIAN_POINT('Ctrl Pts',(-48.353973431638,15.3157731517017,-19.7471174013183));
#31535=CARTESIAN_POINT('Ctrl Pts',(-48.353973431638,15.4434377916669,-19.6823200414401));
#31536=CARTESIAN_POINT('Ctrl Pts',(-48.2504725327236,14.1211388850897,-16.7051598239745));
#31537=CARTESIAN_POINT('Ctrl Pts',(-48.3539734316379,14.2126904025447,-16.6868950101451));
#31538=CARTESIAN_POINT('Ctrl Pts',(-48.3539734316379,14.3421540079377,-16.6323059622874));
#31539=CARTESIAN_POINT('Ctrl Pts',(-48.2559025241611,12.8451845281714,-11.9819322414057));
#31540=CARTESIAN_POINT('Ctrl Pts',(-48.3539734316379,12.9358419174516,-11.9627573972046));
#31541=CARTESIAN_POINT('Ctrl Pts',(-48.3539734316379,13.0661994464396,-11.9283372932442));
#31542=CARTESIAN_POINT('Ctrl Pts',(-48.2574842477434,12.4841939488209,-10.3943253952016));
#31543=CARTESIAN_POINT('Ctrl Pts',(-48.353973431638,12.5748700381568,-10.377060491345));
#31544=CARTESIAN_POINT('Ctrl Pts',(-48.3539734316379,12.7052089420493,-10.3474501811343));
#31545=CARTESIAN_POINT('Ctrl Pts',(-48.2600649268728,11.9034070980987,-7.16859371359221));
#31546=CARTESIAN_POINT('Ctrl Pts',(-48.3539734316379,11.9947391307946,-7.15708402075537));
#31547=CARTESIAN_POINT('Ctrl Pts',(-48.3539734316379,12.1244225188063,-7.13575072146176));
#31548=CARTESIAN_POINT('Ctrl Pts',(-48.2610519234887,11.6863323985655,-5.5241818920662));
#31549=CARTESIAN_POINT('Ctrl Pts',(-48.353973431638,11.7776141645414,-5.51460558027628));
#31550=CARTESIAN_POINT('Ctrl Pts',(-48.3539734316379,11.9073477677922,-5.49868534862248));
#31551=CARTESIAN_POINT('Ctrl Pts',(-48.261663511885,11.5522837206279,-3.87248433002591));
#31552=CARTESIAN_POINT('Ctrl Pts',(-48.353973431638,11.6436417569439,-3.86503544728664));
#31553=CARTESIAN_POINT('Ctrl Pts',(-48.3539734316379,11.7732992272621,-3.85446429447611));
#31554=CARTESIAN_POINT('Origin',(0.0835265683620477,11.3536536794531,0.0824317919394229));
#31555=CARTESIAN_POINT('Origin',(0.0835265683620477,11.3536536794531,0.0824317919394229));
#31556=CARTESIAN_POINT('Ctrl Pts',(48.5210265683622,16.8990456170575,-23.0860157986068));
#31557=CARTESIAN_POINT('Ctrl Pts',(48.5210265683622,16.7639535854308,-23.14458938147));
#31558=CARTESIAN_POINT('Ctrl Pts',(48.4074773267406,16.6779610391845,-23.1819141669453));
#31559=CARTESIAN_POINT('Ctrl Pts',(48.5210265683621,15.5488264423803,-19.9724299127091));
#31560=CARTESIAN_POINT('Ctrl Pts',(48.5210265683621,15.421754102374,-20.0395475263466));
#31561=CARTESIAN_POINT('Ctrl Pts',(48.4125145055694,15.3277344823348,-20.0578585833071));
#31562=CARTESIAN_POINT('Ctrl Pts',(48.5210265683621,14.3828771896198,-16.7823795949988));
#31563=CARTESIAN_POINT('Ctrl Pts',(48.5210265683621,14.2535943246426,-16.8384455883479));
#31564=CARTESIAN_POINT('Ctrl Pts',(48.4172647900869,14.1617844287939,-16.8558621541832));
#31565=CARTESIAN_POINT('Ctrl Pts',(48.5210265683621,13.0662924545663,-11.9287072175551));
#31566=CARTESIAN_POINT('Ctrl Pts',(48.5210265683621,12.9358690854413,-11.9631452471962));
#31567=CARTESIAN_POINT('Ctrl Pts',(48.4228719618904,12.845200563322,-11.9823199869963));
#31568=CARTESIAN_POINT('Ctrl Pts',(48.5210265683621,12.7052707111109,-10.3477586668265));
#31569=CARTESIAN_POINT('Ctrl Pts',(48.5210265683621,12.5748662546476,-10.377384989854));
#31570=CARTESIAN_POINT('Ctrl Pts',(48.4244550341077,12.4841786131515,-10.3946498939195));
#31571=CARTESIAN_POINT('Ctrl Pts',(48.5210265683621,12.0967706305342,-6.98287544832615));
#31572=CARTESIAN_POINT('Ctrl Pts',(48.5210265683621,11.9671239054848,-7.00421648724047));
#31573=CARTESIAN_POINT('Ctrl Pts',(48.4271609489138,11.8756772066794,-7.01505958302208));
#31574=CARTESIAN_POINT('Ctrl Pts',(48.5210265683621,11.867306293034,-5.19149268823613));
#31575=CARTESIAN_POINT('Ctrl Pts',(48.5210265683621,11.7375302448688,-5.20668019500151));
#31576=CARTESIAN_POINT('Ctrl Pts',(48.4282082222567,11.6462130037594,-5.21561646581236));
#31577=CARTESIAN_POINT('Ctrl Pts',(48.5210265683621,11.7377723215061,-3.39157010211078));
#31578=CARTESIAN_POINT('Ctrl Pts',(48.521026568362,11.6080928971653,-3.40090234579438));
#31579=CARTESIAN_POINT('Ctrl Pts',(48.4288000980576,11.5166787215354,-3.4074882922648));
#31580=CARTESIAN_POINT('Ctrl Pts',(48.4082566029293,16.4951170442608,22.9203829774002));
#31581=CARTESIAN_POINT('Ctrl Pts',(48.521026568362,16.5812943403342,22.8835600856804));
#31582=CARTESIAN_POINT('Ctrl Pts',(48.521026568362,16.716129335031,22.8259492283893));
#31583=CARTESIAN_POINT('Ctrl Pts',(48.4130350776236,15.2224248760375,19.9315087692866));
#31584=CARTESIAN_POINT('Ctrl Pts',(48.521026568362,15.3157731540769,19.9119809919554));
#31585=CARTESIAN_POINT('Ctrl Pts',(48.521026568362,15.4434377940522,19.8471836320167));
#31586=CARTESIAN_POINT('Ctrl Pts',(48.4175256694355,14.12113888602,16.870023411326));
#31587=CARTESIAN_POINT('Ctrl Pts',(48.521026568362,14.2126904034778,16.8517585975199));
#31588=CARTESIAN_POINT('Ctrl Pts',(48.521026568362,14.3421540088633,16.7971695496233));
#31589=CARTESIAN_POINT('Ctrl Pts',(48.4229556608863,12.8451845281721,12.1467958252831));
#31590=CARTESIAN_POINT('Ctrl Pts',(48.521026568362,12.9358419174544,12.1276209810818));
#31591=CARTESIAN_POINT('Ctrl Pts',(48.521026568362,13.0661994464451,12.0932008771218));
#31592=CARTESIAN_POINT('Ctrl Pts',(48.4245373844683,12.4841939488219,10.5591889790814));
#31593=CARTESIAN_POINT('Ctrl Pts',(48.521026568362,12.5748700381609,10.541924075223));
#31594=CARTESIAN_POINT('Ctrl Pts',(48.521026568362,12.7052089420549,10.5123137650119));
#31595=CARTESIAN_POINT('Ctrl Pts',(48.427118063595,11.9034070974575,7.33345729393522));
#31596=CARTESIAN_POINT('Ctrl Pts',(48.521026568362,11.9947391301531,7.32194760111541));
#31597=CARTESIAN_POINT('Ctrl Pts',(48.521026568362,12.124422518164,7.30061430182188));
#31598=CARTESIAN_POINT('Ctrl Pts',(48.4281050602037,11.686332397615,5.68904546884577));
#31599=CARTESIAN_POINT('Ctrl Pts',(48.5210265683621,11.7776141635803,5.67946915707043));
#31600=CARTESIAN_POINT('Ctrl Pts',(48.521026568362,11.9073477668319,5.66354892543314));
#31601=CARTESIAN_POINT('Ctrl Pts',(48.4287166486124,11.5522837197589,4.03734790320594));
#31602=CARTESIAN_POINT('Ctrl Pts',(48.5210265683621,11.6436417560773,4.02989902048659));
#31603=CARTESIAN_POINT('Ctrl Pts',(48.521026568362,11.7732992263959,4.01932786770446));
#31604=CARTESIAN_POINT('Ctrl Pts',(48.4286600918172,11.5746245485738,4.30318207891633));
#31605=CARTESIAN_POINT('Ctrl Pts',(48.4289711156128,11.5746245276893,4.29961932362112));
#31606=CARTESIAN_POINT('Ctrl Pts',(48.4433803641393,11.5884292819488,4.29756566916935));
#31607=CARTESIAN_POINT('Ctrl Pts',(48.4724914340702,11.6268390447666,4.29414590646321));
#31608=CARTESIAN_POINT('Ctrl Pts',(48.4870160522355,11.6516801004069,4.29278764850995));
#31609=CARTESIAN_POINT('Ctrl Pts',(48.4970122186807,11.6756605207397,4.29147094879272));
#31610=CARTESIAN_POINT('Origin',(0.0835265683620477,16.1705954176946,0.0824317919394229));
#31611=CARTESIAN_POINT('Origin',(22.7707018927938,16.1705954176946,48.6077790136406));
#31612=CARTESIAN_POINT('Origin',(-48.6664734316379,16.1705954176946,-44.2925682080606));
#31613=CARTESIAN_POINT('Origin',(-48.6664734316379,16.1705954176946,21.5181263879129));
#31614=CARTESIAN_POINT('Ctrl Pts',(-48.3539734316379,16.8990456227292,23.2508793955723));
#31615=CARTESIAN_POINT('Ctrl Pts',(-48.3539734316379,16.7639535910939,23.3094529784638));
#31616=CARTESIAN_POINT('Ctrl Pts',(-48.2404241899901,16.6779610448551,23.3467777639552));
#31617=CARTESIAN_POINT('Ctrl Pts',(-48.3539734316379,15.5488264456615,20.1372935055198));
#31618=CARTESIAN_POINT('Ctrl Pts',(-48.3539734316379,15.4217541056756,20.204411119231));
#31619=CARTESIAN_POINT('Ctrl Pts',(-48.2454613688405,15.3277344856077,20.2227221761541));
#31620=CARTESIAN_POINT('Ctrl Pts',(-48.3539734316379,14.3828771908746,16.9472431835038));
#31621=CARTESIAN_POINT('Ctrl Pts',(-48.353973431638,14.2535943258927,17.0033091768937));
#31622=CARTESIAN_POINT('Ctrl Pts',(-48.2502116533547,14.1617844300463,17.0207257427074));
#31623=CARTESIAN_POINT('Ctrl Pts',(-48.3539734316379,13.0662924545663,12.0935708014341));
#31624=CARTESIAN_POINT('Ctrl Pts',(-48.3539734316379,12.9358690854431,12.1280088310745));
#31625=CARTESIAN_POINT('Ctrl Pts',(-48.2558188251637,12.8452005633196,12.1471835708758));
#31626=CARTESIAN_POINT('Ctrl Pts',(-48.3539734316379,12.7052707111123,10.5126222507054));
#31627=CARTESIAN_POINT('Ctrl Pts',(-48.3539734316379,12.5748662546484,10.5422485737337));
#31628=CARTESIAN_POINT('Ctrl Pts',(-48.2574018973817,12.4841786131498,10.5595134777991));
#31629=CARTESIAN_POINT('Ctrl Pts',(-48.3539734316379,12.09677062968,7.14773902748995));
#31630=CARTESIAN_POINT('Ctrl Pts',(-48.353973431638,11.9671239046302,7.16908006640543));
#31631=CARTESIAN_POINT('Ctrl Pts',(-48.2601078121902,11.8756772058235,7.17992316216539));
#31632=CARTESIAN_POINT('Ctrl Pts',(-48.353973431638,11.8673062918515,5.35635626264026));
#31633=CARTESIAN_POINT('Ctrl Pts',(-48.3539734316379,11.7375302436853,5.37154376938283));
#31634=CARTESIAN_POINT('Ctrl Pts',(-48.261155085551,11.6462130025588,5.38048004017552));
#31635=CARTESIAN_POINT('Ctrl Pts',(-48.353973431638,11.7377723204669,3.55643367171442));
#31636=CARTESIAN_POINT('Ctrl Pts',(-48.353973431638,11.6080928961254,3.5657659153597));
#31637=CARTESIAN_POINT('Ctrl Pts',(-48.2617469613299,11.5166787204998,3.57235186180297));
#31638=CARTESIAN_POINT('Ctrl Pts',(-48.2416470424886,16.3915662868154,22.6760194541553));
#31639=CARTESIAN_POINT('Ctrl Pts',(-48.2550583113966,16.3813243440928,22.6231518753406));
#31640=CARTESIAN_POINT('Ctrl Pts',(-48.2665413365694,16.371060182303,22.5700615306077));
#31641=CARTESIAN_POINT('Ctrl Pts',(-48.2765223146654,16.3607859543218,22.5168101838168));
#31642=CARTESIAN_POINT('Ctrl Pts',(-48.2870013352819,16.3499990508944,22.4609016390319));
#31643=CARTESIAN_POINT('Ctrl Pts',(-48.2958241781355,16.3392010160241,22.404815463508));
#31644=CARTESIAN_POINT('Ctrl Pts',(-48.3034279033223,16.3284020448452,22.3486028384447));
#31645=CARTESIAN_POINT('Ctrl Pts',(-48.3117577974371,16.3165717532105,22.2870218103047));
#31646=CARTESIAN_POINT('Ctrl Pts',(-48.318624191821,16.304740305612,22.225288907512));
#31647=CARTESIAN_POINT('Ctrl Pts',(-48.3245425371134,16.2929170788295,22.1634496834489));
#31648=CARTESIAN_POINT('Ctrl Pts',(-48.3262538527391,16.289498340696,22.1455685992625));
#31649=CARTESIAN_POINT('Ctrl Pts',(-48.3278855787644,16.2860802681944,22.12767850517));
#31650=CARTESIAN_POINT('Ctrl Pts',(-48.3294494632194,16.2826630404187,22.1097802343589));
#31651=CARTESIAN_POINT('Ctrl Pts',(-48.3297163898139,16.282079781873,22.1067253255002));
#31652=CARTESIAN_POINT('Ctrl Pts',(-48.3299809399224,16.2814964941327,22.1036698975148));
#31653=CARTESIAN_POINT('Ctrl Pts',(-48.3302431245746,16.2809131770539,22.1006139497897));
#31654=CARTESIAN_POINT('Ctrl Pts',(-48.3374362318239,16.2649097143329,22.0167731927283));
#31655=CARTESIAN_POINT('Ctrl Pts',(-48.3428413032002,16.2489117074373,21.9326789574656));
#31656=CARTESIAN_POINT('Ctrl Pts',(-48.346668755976,16.2329404500536,21.8484396681528));
#31657=CARTESIAN_POINT('Ctrl Pts',(-48.3508266167155,16.2155904609288,21.7569283538995));
#31658=CARTESIAN_POINT('Ctrl Pts',(-48.3531227295817,16.1982718719703,21.6652451220175));
#31659=CARTESIAN_POINT('Ctrl Pts',(-48.353776871749,16.1810063870583,21.573494203965));
#31660=CARTESIAN_POINT('Ctrl Pts',(-48.3539083353861,16.177536524456,21.5550549257804));
#31661=CARTESIAN_POINT('Ctrl Pts',(-48.3539733323427,16.1740687951328,21.5366128328767));
#31662=CARTESIAN_POINT('Ctrl Pts',(-48.3539734315243,16.1706033612909,21.5181686663419));
#31663=CARTESIAN_POINT('Ctrl Pts',(-48.353987706665,11.4728541727075,0.0824317919420715));
#31664=CARTESIAN_POINT('Ctrl Pts',(-48.3539872411712,11.4515020042572,0.0824317919420012));
#31665=CARTESIAN_POINT('Ctrl Pts',(-48.3536289324683,11.4284235901226,0.0824317919405622));
#31666=CARTESIAN_POINT('Ctrl Pts',(-48.3495242803204,11.3941472536996,0.0824317919402862));
#31667=CARTESIAN_POINT('Ctrl Pts',(-48.3539734316379,11.3720285904897,0.08243179194024));
#31668=CARTESIAN_POINT('Ctrl Pts',(-48.3539734316379,11.3536536794531,0.0824317919394318));
#31669=CARTESIAN_POINT('Ctrl Pts',(-48.3539875902917,11.4675161305949,0.433477097230381));
#31670=CARTESIAN_POINT('Ctrl Pts',(-48.3539275501285,11.4488974993902,0.355621276400125));
#31671=CARTESIAN_POINT('Ctrl Pts',(-48.353663231583,11.4285976962987,0.338435236571238));
#31672=CARTESIAN_POINT('Ctrl Pts',(-48.3495016478723,11.3940705712691,0.360237634010735));
#31673=CARTESIAN_POINT('Ctrl Pts',(-48.3539734316379,11.3720285904897,0.399226071278088));
#31674=CARTESIAN_POINT('Ctrl Pts',(-48.3539734316379,11.3536536794531,0.433719204637307));
#31675=CARTESIAN_POINT('Ctrl Pts',(-48.3525301621484,11.4659265087691,0.784574340176142));
#31676=CARTESIAN_POINT('Ctrl Pts',(-48.3527335277693,11.447718516688,0.651206502089013));
#31677=CARTESIAN_POINT('Ctrl Pts',(-48.3522992264021,11.428587933622,0.625439688759691));
#31678=CARTESIAN_POINT('Ctrl Pts',(-48.3473885439727,11.3934281614349,0.66646486508276));
#31679=CARTESIAN_POINT('Ctrl Pts',(-48.3508557705029,11.3718199008203,0.733256854734286));
#31680=CARTESIAN_POINT('Ctrl Pts',(-48.3501520759131,11.3536536794531,0.785006622606324));
#31681=CARTESIAN_POINT('Ctrl Pts',(-48.3427993417961,11.4643966328771,1.48689990373394));
#31682=CARTESIAN_POINT('Ctrl Pts',(-48.3443675175871,11.4452664260877,1.29386039425038));
#31683=CARTESIAN_POINT('Ctrl Pts',(-48.3432090309081,11.4271829834973,1.26166887657828));
#31684=CARTESIAN_POINT('Ctrl Pts',(-48.3361366891649,11.39130385313,1.32614678064444));
#31685=CARTESIAN_POINT('Ctrl Pts',(-48.3366948692382,11.3711415135622,1.42281620238213));
#31686=CARTESIAN_POINT('Ctrl Pts',(-48.3348648315386,11.3536536794531,1.48749857171648));
#31687=CARTESIAN_POINT('Ctrl Pts',(-48.334525949587,11.4644563788108,1.83812822434599));
#31688=CARTESIAN_POINT('Ctrl Pts',(-48.3370692580422,11.4439380177891,1.64093757517121));
#31689=CARTESIAN_POINT('Ctrl Pts',(-48.3353565172244,11.425732495649,1.61090009066833));
#31690=CARTESIAN_POINT('Ctrl Pts',(-48.326934699005,11.389794304459,1.67960165301714));
#31691=CARTESIAN_POINT('Ctrl Pts',(-48.3256515256245,11.3706718159735,1.77834069986839));
#31692=CARTESIAN_POINT('Ctrl Pts',(-48.3233989425165,11.3536536794531,1.83870311340059));
#31693=CARTESIAN_POINT('Ctrl Pts',(-48.3072618605772,11.4603777656236,2.54074314558774));
#31694=CARTESIAN_POINT('Ctrl Pts',(-48.3087333779098,11.4381382649983,2.39327412400269));
#31695=CARTESIAN_POINT('Ctrl Pts',(-48.3062335055346,11.4203247666438,2.37176704511889));
#31696=CARTESIAN_POINT('Ctrl Pts',(-48.2977571518657,11.3861758639155,2.42404521997606));
#31697=CARTESIAN_POINT('Ctrl Pts',(-48.2950709238183,11.3696277842964,2.49783047371681));
#31698=CARTESIAN_POINT('Ctrl Pts',(-48.2928171719614,11.3536536794531,2.54094611738018));
#31699=CARTESIAN_POINT('Ctrl Pts',(-48.2896456942886,11.4600103666203,2.8917100690178));
#31700=CARTESIAN_POINT('Ctrl Pts',(-48.2899913249917,11.4370088609558,2.76883563487708));
#31701=CARTESIAN_POINT('Ctrl Pts',(-48.2869150458799,11.4187667259072,2.75380781417152));
#31702=CARTESIAN_POINT('Ctrl Pts',(-48.2785859525266,11.3847952022384,2.80028584083724));
#31703=CARTESIAN_POINT('Ctrl Pts',(-48.2755338718729,11.369053450208,2.86179168820836));
#31704=CARTESIAN_POINT('Ctrl Pts',(-48.2737012896825,11.3536536794531,2.89198459022056));
#31705=CARTESIAN_POINT('Ctrl Pts',(-48.2472153956208,11.4633689234831,3.59326763363504));
#31706=CARTESIAN_POINT('Ctrl Pts',(-48.2437182974631,11.4394032486783,3.52561349527619));
#31707=CARTESIAN_POINT('Ctrl Pts',(-48.2392225168533,11.4193327724023,3.52141678779854));
#31708=CARTESIAN_POINT('Ctrl Pts',(-48.2313449268363,11.3835624194323,3.55118314893263));
#31709=CARTESIAN_POINT('Ctrl Pts',(-48.2285187243939,11.3679565169509,3.58514621754432));
#31710=CARTESIAN_POINT('Ctrl Pts',(-48.2278104516838,11.3536536794531,3.59381163136407));
#31711=CARTESIAN_POINT('Ctrl Pts',(-48.2224012632416,11.4670948793492,3.94385827482222));
#31712=CARTESIAN_POINT('Ctrl Pts',(-48.2161873228526,11.4429270404433,3.90682984480091));
#31713=CARTESIAN_POINT('Ctrl Pts',(-48.2108487059855,11.4214568596339,3.9069829679927));
#31714=CARTESIAN_POINT('Ctrl Pts',(-48.203275617213,11.3837102983034,3.92583579004338));
#31715=CARTESIAN_POINT('Ctrl Pts',(-48.2010411453076,11.3674339177823,3.94453548890227));
#31716=CARTESIAN_POINT('Ctrl Pts',(-48.2010354948423,11.3536536794531,3.94460021021516));
#31717=CARTESIAN_POINT('Ctrl Pts',(-48.1943732865555,11.4732422824942,4.29441317095732));
#31718=CARTESIAN_POINT('Ctrl Pts',(-48.1844415394016,11.4493335556629,4.29430779651731));
#31719=CARTESIAN_POINT('Ctrl Pts',(-48.178454383799,11.4261172510678,4.29450986621179));
#31720=CARTESIAN_POINT('Ctrl Pts',(-48.1714459461707,11.384958159128,4.29496669282076));
#31721=CARTESIAN_POINT('Ctrl Pts',(-48.170424664145,11.3670153717833,4.29522144973525));
#31722=CARTESIAN_POINT('Ctrl Pts',(-48.170424664145,11.3536536794531,4.29522144973525));
#31723=CARTESIAN_POINT('Origin',(-48.483024238303,11.3534224546476,4.32103607293009));
#31724=CARTESIAN_POINT('Ctrl Pts',(48.5210408433891,11.4728541727075,0.0824317919368853));
#31725=CARTESIAN_POINT('Ctrl Pts',(48.5210409597623,11.4781922148201,0.4334770972252));
#31726=CARTESIAN_POINT('Ctrl Pts',(48.5195837679409,11.4874426767152,0.784346426598513));
#31727=CARTESIAN_POINT('Ctrl Pts',(48.5162561594212,11.5143737377389,1.48575918656021));
#31728=CARTESIAN_POINT('Ctrl Pts',(48.5143857427228,11.5320543368676,1.83630261714859));
#31729=CARTESIAN_POINT('Ctrl Pts',(48.5119067425813,11.5986492866067,2.88748314030395));
#31730=CARTESIAN_POINT('Ctrl Pts',(48.5072128795892,11.6392592214936,3.58975549746708));
#31731=CARTESIAN_POINT('Ctrl Pts',(48.4970122186807,11.6756605207398,4.29147094879272));
#31732=CARTESIAN_POINT('Ctrl Pts',(48.5210407270154,11.467516130595,0.433477097225236));
#31733=CARTESIAN_POINT('Ctrl Pts',(48.5200991113385,11.4749860898032,0.706493517505826));
#31734=CARTESIAN_POINT('Ctrl Pts',(48.5183837318963,11.484480312248,0.997236186162579));
#31735=CARTESIAN_POINT('Ctrl Pts',(48.5144994210127,11.5105174196337,1.61112122689591));
#31736=CARTESIAN_POINT('Ctrl Pts',(48.5123333385923,11.5270830007415,1.93426197940565));
#31737=CARTESIAN_POINT('Ctrl Pts',(48.5086939112088,11.5919036248635,2.94770884758093));
#31738=CARTESIAN_POINT('Ctrl Pts',(48.5032144671198,11.6298708101947,3.62572662260832));
#31739=CARTESIAN_POINT('Ctrl Pts',(48.4920141354581,11.6636703105733,4.29212929865133));
#31740=CARTESIAN_POINT('Ctrl Pts',(48.5195832988718,11.4659265087693,0.784574340170486));
#31741=CARTESIAN_POINT('Ctrl Pts',(48.5180114541276,11.4745419834779,0.997581380068577));
#31742=CARTESIAN_POINT('Ctrl Pts',(48.5159956580504,11.4840908039497,1.24226674628784));
#31743=CARTESIAN_POINT('Ctrl Pts',(48.5114095528557,11.5090816899177,1.78530549798337));
#31744=CARTESIAN_POINT('Ctrl Pts',(48.5088435172697,11.5245577996643,2.08365645410939));
#31745=CARTESIAN_POINT('Ctrl Pts',(48.5036610022584,11.5859418512174,3.04468476956754));
#31746=CARTESIAN_POINT('Ctrl Pts',(48.4973225964196,11.6209827896584,3.68769531787518));
#31747=CARTESIAN_POINT('Ctrl Pts',(48.4858839393055,11.6514649415801,4.29279803806896));
#31748=CARTESIAN_POINT('Ctrl Pts',(48.5098524785193,11.4643966328772,1.48689990372619));
#31749=CARTESIAN_POINT('Ctrl Pts',(48.5081357594265,11.4744825705816,1.61268347054477));
#31750=CARTESIAN_POINT('Ctrl Pts',(48.5060961369513,11.4843329006934,1.78661204515917));
#31751=CARTESIAN_POINT('Ctrl Pts',(48.5010454693456,11.5079260458425,2.20924934388482));
#31752=CARTESIAN_POINT('Ctrl Pts',(48.4980397661294,11.5217114161925,2.45795503130826));
#31753=CARTESIAN_POINT('Ctrl Pts',(48.4906361947471,11.5755468354576,3.28398547902237));
#31754=CARTESIAN_POINT('Ctrl Pts',(48.4830998624059,11.6050189470212,3.83329117874236));
#31755=CARTESIAN_POINT('Ctrl Pts',(48.4724837048702,11.6282480883245,4.29423381231316));
#31756=CARTESIAN_POINT('Ctrl Pts',(48.5015790863104,11.4644563788109,1.83812822433663));
#31757=CARTESIAN_POINT('Ctrl Pts',(48.5003285876188,11.4748353413218,1.93670273339578));
#31758=CARTESIAN_POINT('Ctrl Pts',(48.498555988222,11.4849166217024,2.08593433631161));
#31759=CARTESIAN_POINT('Ctrl Pts',(48.4937353771472,11.508146276442,2.45901835920677));
#31760=CARTESIAN_POINT('Ctrl Pts',(48.4906923512561,11.5213343690929,2.68286794494415));
#31761=CARTESIAN_POINT('Ctrl Pts',(48.4826251618687,11.5710816706553,3.42631530142816));
#31762=CARTESIAN_POINT('Ctrl Pts',(48.4747689990924,11.5979431249203,3.91691834434268));
#31763=CARTESIAN_POINT('Ctrl Pts',(48.4652136665875,11.6172366040621,4.29500084713974));
#31764=CARTESIAN_POINT('Ctrl Pts',(48.4606829527973,11.4583384590298,2.89205060619288));
#31765=CARTESIAN_POINT('Ctrl Pts',(48.4602502314484,11.4700074930205,2.95333187694758));
#31766=CARTESIAN_POINT('Ctrl Pts',(48.4596398458099,11.481882800679,3.05034122263737));
#31767=CARTESIAN_POINT('Ctrl Pts',(48.457639336452,11.5065304546877,3.28859697245894));
#31768=CARTESIAN_POINT('Ctrl Pts',(48.4562520617537,11.5193254972046,3.42984175702388));
#31769=CARTESIAN_POINT('Ctrl Pts',(48.4521822008652,11.5598336028455,3.87910730675446));
#31770=CARTESIAN_POINT('Ctrl Pts',(48.4481398060042,11.5806510816358,4.15478254176723));
#31771=CARTESIAN_POINT('Ctrl Pts',(48.4433803641393,11.5884292819488,4.29756566916935));
#31772=CARTESIAN_POINT('Ctrl Pts',(48.4174823766521,11.4609474762041,3.59330337868378));
#31773=CARTESIAN_POINT('Ctrl Pts',(48.4187304434642,11.4731609516943,3.63027912148489));
#31774=CARTESIAN_POINT('Ctrl Pts',(48.4200748650817,11.4863352799677,3.69245653604027));
#31775=CARTESIAN_POINT('Ctrl Pts',(48.4227028837574,11.5121367174564,3.83761867075702));
#31776=CARTESIAN_POINT('Ctrl Pts',(48.4239864808157,11.5247638266716,3.92060339091839));
#31777=CARTESIAN_POINT('Ctrl Pts',(48.4273657338961,11.5581209387927,4.15637445295775));
#31778=CARTESIAN_POINT('Ctrl Pts',(48.4289898518242,11.5743267261738,4.29597769639097));
#31779=CARTESIAN_POINT('Ctrl Pts',(48.4289711156128,11.5746245276893,4.29961932362112));
#31780=CARTESIAN_POINT('Ctrl Pts',(48.3614264232796,11.4732422824942,4.29441317095744));
#31781=CARTESIAN_POINT('Ctrl Pts',(48.3663922968565,11.4851966459098,4.29446585817745));
#31782=CARTESIAN_POINT('Ctrl Pts',(48.3730775094482,11.497472006951,4.29459893941734));
#31783=CARTESIAN_POINT('Ctrl Pts',(48.3875464536895,11.5208685373805,4.29515956957329));
#31784=CARTESIAN_POINT('Ctrl Pts',(48.395330185339,11.5319897067687,4.29558711848934));
#31785=CARTESIAN_POINT('Ctrl Pts',(48.4168189204169,11.5609276470972,4.2975119862063));
#31786=CARTESIAN_POINT('Ctrl Pts',(48.4286614639743,11.5743188502015,4.29965152597602));
#31787=CARTESIAN_POINT('Ctrl Pts',(48.4286600918172,11.5746245485738,4.30318207891633));
#31788=CARTESIAN_POINT('Ctrl Pts',(48.4286600918175,11.5746245484995,4.30318207805718));
#31789=CARTESIAN_POINT('Ctrl Pts',(48.428660173147,11.5746064038391,4.30297252432489));
#31790=CARTESIAN_POINT('Ctrl Pts',(48.4286216603492,11.5745497853935,4.302816343613));
#31791=CARTESIAN_POINT('Ctrl Pts',(48.4285848981368,11.5744984448488,4.30270012134642));
#31792=CARTESIAN_POINT('Ctrl Pts',(48.4285480454769,11.574446977989,4.30258361313381));
#31793=CARTESIAN_POINT('Ctrl Pts',(48.4285118923269,11.5743997047824,4.30250737386098));
#31794=CARTESIAN_POINT('Ctrl Pts',(48.4284895565794,11.574370552647,4.30246107541817));
#31795=CARTESIAN_POINT('Ctrl Pts',(48.4284449398726,11.5743123198847,4.30236859209968));
#31796=CARTESIAN_POINT('Ctrl Pts',(48.4284142675547,11.5742733795738,4.30231835462613));
#31797=CARTESIAN_POINT('Ctrl Pts',(48.4283846331628,11.5742358022906,4.30227052046444));
#31798=CARTESIAN_POINT('Ctrl Pts',(48.4283253643788,11.5741606477241,4.30217485214104));
#31799=CARTESIAN_POINT('Ctrl Pts',(48.428273850473,11.5740963865937,4.30210514179006));
#31800=CARTESIAN_POINT('Ctrl Pts',(48.4282197552865,11.5740292687569,4.30203697502406));
#31801=CARTESIAN_POINT('Ctrl Pts',(48.4280343609139,11.5737992433141,4.3018033547035));
#31802=CARTESIAN_POINT('Ctrl Pts',(48.4278244339668,11.5735441534495,4.3016127031576));
#31803=CARTESIAN_POINT('Ctrl Pts',(48.4276145416169,11.5732903201755,4.30144691952107));
#31804=CARTESIAN_POINT('Ctrl Pts',(48.4273317964772,11.5729483823938,4.3012235930516));
#31805=CARTESIAN_POINT('Ctrl Pts',(48.4270468518926,11.5726061687629,4.30104387224263));
#31806=CARTESIAN_POINT('Ctrl Pts',(48.4267515418286,11.5722518189,4.3008773859058));
#31807=CARTESIAN_POINT('Ctrl Pts',(48.4263482983298,11.5717679570344,4.30065005016229));
#31808=CARTESIAN_POINT('Ctrl Pts',(48.4259410026168,11.571280018306,4.30045936740763));
#31809=CARTESIAN_POINT('Ctrl Pts',(48.4255334993493,11.5707911793166,4.30028708850175));
#31810=CARTESIAN_POINT('Ctrl Pts',(48.4248366295841,11.5699552176474,4.29999247500965));
#31811=CARTESIAN_POINT('Ctrl Pts',(48.4241358475905,11.5691127678625,4.29975133277005));
#31812=CARTESIAN_POINT('Ctrl Pts',(48.4234368426892,11.5682688436226,4.2995356576737));
#31813=CARTESIAN_POINT('Ctrl Pts',(48.4222570898919,11.5668445017031,4.29917164978511));
#31814=CARTESIAN_POINT('Ctrl Pts',(48.4210795566691,11.5654127733163,4.2988812226714));
#31815=CARTESIAN_POINT('Ctrl Pts',(48.4199071305588,11.5639752438872,4.29862402961716));
#31816=CARTESIAN_POINT('Ctrl Pts',(48.4180824832977,11.5617380162167,4.29822375995592));
#31817=CARTESIAN_POINT('Ctrl Pts',(48.4162697117118,11.5594864488171,4.29790736451354));
#31818=CARTESIAN_POINT('Ctrl Pts',(48.4144713964367,11.5572216877119,4.29763057295059));
#31819=CARTESIAN_POINT('Ctrl Pts',(48.4117670663131,11.5538159102244,4.2972143301638));
#31820=CARTESIAN_POINT('Ctrl Pts',(48.4090945540814,11.550379518606,4.29689092942539));
#31821=CARTESIAN_POINT('Ctrl Pts',(48.4064601460237,11.5469146454501,4.29661383979601));
#31822=CARTESIAN_POINT('Ctrl Pts',(48.4051282865519,11.545162933479,4.29647375350743));
#31823=CARTESIAN_POINT('Ctrl Pts',(48.4038056232218,11.5434032085324,4.2963463114669));
#31824=CARTESIAN_POINT('Ctrl Pts',(48.4024930970316,11.5416356868782,4.29622874106166));
#31825=CARTESIAN_POINT('Ctrl Pts',(48.3982785721702,11.5359601704501,4.295851222198));
#31826=CARTESIAN_POINT('Ctrl Pts',(48.3941689719985,11.5302068773408,4.295572141369));
#31827=CARTESIAN_POINT('Ctrl Pts',(48.390190769549,11.5243619142254,4.29534669563895));
#31828=CARTESIAN_POINT('Ctrl Pts',(48.3867923502581,11.5193687959371,4.29515410636583));
#31829=CARTESIAN_POINT('Ctrl Pts',(48.3834901365878,11.5143094032157,4.29500239890131));
#31830=CARTESIAN_POINT('Ctrl Pts',(48.3803119815688,11.5091702721658,4.29487925449532));
#31831=CARTESIAN_POINT('Ctrl Pts',(48.3767563627651,11.5034207757166,4.29474148444857));
#31832=CARTESIAN_POINT('Ctrl Pts',(48.3733540435004,11.4975716267243,4.29463972870061));
#31833=CARTESIAN_POINT('Ctrl Pts',(48.3701734723775,11.49159405132,4.29456450114538));
#31834=CARTESIAN_POINT('Ctrl Pts',(48.3675896123393,11.4867379366112,4.29450338712962));
#31835=CARTESIAN_POINT('Ctrl Pts',(48.3651512727409,11.4817961991037,4.29445995841077));
#31836=CARTESIAN_POINT('Ctrl Pts',(48.3629292995066,11.4767527247579,4.29443096808727));
#31837=CARTESIAN_POINT('Ctrl Pts',(48.3624161617827,11.4755879956304,4.29442427312426));
#31838=CARTESIAN_POINT('Ctrl Pts',(48.3619147674745,11.4744178750436,4.29441835222065));
#31839=CARTESIAN_POINT('Ctrl Pts',(48.3614264232796,11.4732422824942,4.29441317095744));
#31840=CARTESIAN_POINT('Ctrl Pts',(21.3906463937529,16.4830953098781,48.8309185363369));
#31841=CARTESIAN_POINT('Ctrl Pts',(21.4003401995189,16.4833744495148,48.4949669229311));
#31842=CARTESIAN_POINT('Ctrl Pts',(21.3997327223527,16.1481826330634,48.5190454048188));
#31843=CARTESIAN_POINT('Ctrl Pts',(21.6479745476933,16.483095324294,48.8379328597607));
#31844=CARTESIAN_POINT('Ctrl Pts',(21.6200830023851,16.483319828549,48.5460524616203));
#31845=CARTESIAN_POINT('Ctrl Pts',(21.6389642094873,16.1929802521112,48.5225608943597));
#31846=CARTESIAN_POINT('Ctrl Pts',(21.9045410908616,16.4830953387802,48.8243898617382));
#31847=CARTESIAN_POINT('Ctrl Pts',(21.8672452314961,16.483273583025,48.5750825049463));
#31848=CARTESIAN_POINT('Ctrl Pts',(21.8768838415007,16.2379895254129,48.5158004457527));
#31849=CARTESIAN_POINT('Ctrl Pts',(22.4076757669193,16.4830953673845,48.743210136482));
#31850=CARTESIAN_POINT('Ctrl Pts',(22.3511228078461,16.4831976839893,48.5682561154872));
#31851=CARTESIAN_POINT('Ctrl Pts',(22.3423318951884,16.3268490737816,48.4752349408482));
#31852=CARTESIAN_POINT('Ctrl Pts',(22.6581433216875,16.4830953816853,48.6788328743123));
#31853=CARTESIAN_POINT('Ctrl Pts',(22.5967474570195,16.4831654080667,48.5419054522021));
#31854=CARTESIAN_POINT('Ctrl Pts',(22.5727876009851,16.3712675955695,48.4432313777772));
#31855=CARTESIAN_POINT('Ctrl Pts',(22.8868233850503,16.4830953949244,48.5476959795698));
#31856=CARTESIAN_POINT('Ctrl Pts',(22.8291967273507,16.4831380278819,48.4517667232661));
#31857=CARTESIAN_POINT('Ctrl Pts',(22.7844241394783,16.4123847430248,48.3774109749067));
#31858=CARTESIAN_POINT('Ctrl Pts',(21.5192634427593,16.17060336129,48.5199317918263));
#31859=CARTESIAN_POINT('Ctrl Pts',(21.6170999500073,16.1889856471435,48.5199312682443));
#31860=CARTESIAN_POINT('Ctrl Pts',(21.7148708403879,16.2074307865443,48.518116604729));
#31861=CARTESIAN_POINT('Ctrl Pts',(21.8124883377731,16.2259200040867,48.5142156384362));
#31862=CARTESIAN_POINT('Ctrl Pts',(21.908956873748,16.2441916028821,48.5103605866552));
#31863=CARTESIAN_POINT('Ctrl Pts',(22.0052762797485,16.2625063923372,48.5044686188699));
#31864=CARTESIAN_POINT('Ctrl Pts',(22.1013380589794,16.2808424439029,48.4962332420434));
#31865=CARTESIAN_POINT('Ctrl Pts',(22.1040951139171,16.2813687042107,48.4959968797094));
#31866=CARTESIAN_POINT('Ctrl Pts',(22.1068517512828,16.2818949414479,48.4957586005132));
#31867=CARTESIAN_POINT('Ctrl Pts',(22.109607981701,16.2824211576432,48.4955183962497));
#31868=CARTESIAN_POINT('Ctrl Pts',(22.1685278155313,16.2936700614283,48.4903835587579));
#31869=CARTESIAN_POINT('Ctrl Pts',(22.2274507987805,16.3049460203239,48.4844875476039));
#31870=CARTESIAN_POINT('Ctrl Pts',(22.2862696411608,16.3162274856622,48.4774282375931));
#31871=CARTESIAN_POINT('Ctrl Pts',(22.340258020577,16.3265824672703,48.4709486692804));
#31872=CARTESIAN_POINT('Ctrl Pts',(22.3941591829442,16.3369421989583,48.4634895977143));
#31873=CARTESIAN_POINT('Ctrl Pts',(22.4478699699773,16.3472864072044,48.4547032934322));
#31874=CARTESIAN_POINT('Ctrl Pts',(22.4969660605998,16.3567418669644,48.4466718864263));
#31875=CARTESIAN_POINT('Ctrl Pts',(22.5459033047808,16.3661844046848,48.4375317183341));
#31876=CARTESIAN_POINT('Ctrl Pts',(22.5945805754926,16.3755943695783,48.4269802673523));
#31877=CARTESIAN_POINT('Ctrl Pts',(22.6221833139186,16.380930346632,48.4209970037632));
#31878=CARTESIAN_POINT('Ctrl Pts',(22.6497020262212,16.3862557688531,48.4145592382452));
#31879=CARTESIAN_POINT('Ctrl Pts',(22.677114230578,16.3915662868154,48.4076054027901));
#31880=CARTESIAN_POINT('Origin',(21.5192211643356,16.1705954176946,48.8324317919394));
#31881=CARTESIAN_POINT('Ctrl Pts',(-48.6664734316379,16.4830954176946,21.5181263879129));
#31882=CARTESIAN_POINT('Ctrl Pts',(-48.353973431638,16.4830954176946,21.5181263879129));
#31883=CARTESIAN_POINT('Ctrl Pts',(-48.3539734316379,16.1705954176947,21.5181263879129));
#31884=CARTESIAN_POINT('Ctrl Pts',(-48.6664734339897,16.4830954176946,21.7328421481057));
#31885=CARTESIAN_POINT('Ctrl Pts',(-48.3893416276193,16.4830954176967,21.7063677013623));
#31886=CARTESIAN_POINT('Ctrl Pts',(-48.3539734316379,16.208073041206,21.7175947316477));
#31887=CARTESIAN_POINT('Ctrl Pts',(-48.6512918054456,16.4830954176946,21.9468604135708));
#31888=CARTESIAN_POINT('Ctrl Pts',(-48.4085265371208,16.4830954176942,21.9119950055367));
#31889=CARTESIAN_POINT('Ctrl Pts',(-48.3463826153449,16.2456622380852,21.9159853456124));
#31890=CARTESIAN_POINT('Ctrl Pts',(-48.583556384038,16.4830954176946,22.3658173905146));
#31891=CARTESIAN_POINT('Ctrl Pts',(-48.4026513877734,16.483095417695,22.3146013303459));
#31892=CARTESIAN_POINT('Ctrl Pts',(-48.312514911035,16.3196601510152,22.3035748967492));
#31893=CARTESIAN_POINT('Ctrl Pts',(-48.5339575321232,16.4830954176946,22.5725362595963));
#31894=CARTESIAN_POINT('Ctrl Pts',(-48.3840456652921,16.483095417695,22.5162624682257));
#31895=CARTESIAN_POINT('Ctrl Pts',(-48.2878455968984,16.3562852232532,22.4939033682569));
#31896=CARTESIAN_POINT('Ctrl Pts',(-48.4418206533393,16.4830954176946,22.7696071163712));
#31897=CARTESIAN_POINT('Ctrl Pts',(-48.3245616669322,16.4830954176946,22.7147847331159));
#31898=CARTESIAN_POINT('Ctrl Pts',(-48.2416470424886,16.3915662868154,22.6760194541553));
#31899=CARTESIAN_POINT('Origin',(-48.4418206533391,16.1705954176946,22.7696071163712));
#31900=CARTESIAN_POINT('Origin',(0.0835265683620477,11.3536536794531,0.0824317919394229));
#31901=CARTESIAN_POINT('Origin',(0.0835265683620477,11.353653679453,0.0824317919394229));
#31902=CARTESIAN_POINT('Ctrl Pts',(23.2519741921975,16.8990456314821,48.5199317919394));
#31903=CARTESIAN_POINT('Ctrl Pts',(23.3105477751332,16.763953599836,48.5199317919394));
#31904=CARTESIAN_POINT('Ctrl Pts',(23.3478725606479,16.6779610536085,48.4063825502508));
#31905=CARTESIAN_POINT('Ctrl Pts',(20.1383882957297,15.5488264507417,48.5199317919394));
#31906=CARTESIAN_POINT('Ctrl Pts',(20.2055059095578,15.4217541107764,48.5199317919394));
#31907=CARTESIAN_POINT('Ctrl Pts',(20.2238169664254,15.3277344906633,48.411419729136));
#31908=CARTESIAN_POINT('Ctrl Pts',(16.9483379670617,14.3828771928117,48.5199317919394));
#31909=CARTESIAN_POINT('Ctrl Pts',(17.0044039605232,14.2535943278388,48.5199317919394));
#31910=CARTESIAN_POINT('Ctrl Pts',(17.0218205262955,14.1617844319789,48.4161700136446));
#31911=CARTESIAN_POINT('Ctrl Pts',(12.0946655778594,13.0662924545662,48.5199317919394));
#31912=CARTESIAN_POINT('Ctrl Pts',(12.1291036075007,12.9358690854399,48.5199317919394));
#31913=CARTESIAN_POINT('Ctrl Pts',(12.1482783473018,12.8452005633163,48.4217771854608));
#31914=CARTESIAN_POINT('Ctrl Pts',(10.5137170271294,12.7052707111067,48.5199317919394));
#31915=CARTESIAN_POINT('Ctrl Pts',(10.5433433501585,12.5748662546398,48.5199317919394));
#31916=CARTESIAN_POINT('Ctrl Pts',(10.5606082542232,12.4841786131435,48.4233602576764));
#31917=CARTESIAN_POINT('Ctrl Pts',(7.14883379663184,12.0967706283699,48.5199317919394));
#31918=CARTESIAN_POINT('Ctrl Pts',(7.1701748355487,11.9671239033221,48.5199317919394));
#31919=CARTESIAN_POINT('Ctrl Pts',(7.18101793127648,11.8756772045064,48.426066172497));
#31920=CARTESIAN_POINT('Ctrl Pts',(5.35745102444326,11.8673062899501,48.5199317919395));
#31921=CARTESIAN_POINT('Ctrl Pts',(5.3726385311504,11.7375302417815,48.5199317919394));
#31922=CARTESIAN_POINT('Ctrl Pts',(5.38157480191148,11.6462130006682,48.4271134458431));
#31923=CARTESIAN_POINT('Ctrl Pts',(3.55752842609651,11.7377723188913,48.5199317919395));
#31924=CARTESIAN_POINT('Ctrl Pts',(3.56686066968263,11.6080928945489,48.5199317919394));
#31925=CARTESIAN_POINT('Ctrl Pts',(3.57344661608542,11.5166787189151,48.4277053216402));
#31926=CARTESIAN_POINT('Origin',(-44.291473431638,16.1705954176946,48.8324317919394));
#31927=CARTESIAN_POINT('Origin',(-21.3521680276115,16.1705954176946,48.8324317919394));
#31928=CARTESIAN_POINT('Origin',(0.0835265683620477,16.1705954176946,0.0824317919394229));
#31929=CARTESIAN_POINT('Origin',(-22.6036487560697,16.1705954176946,48.6077790136406));
#31930=CARTESIAN_POINT('Ctrl Pts',(0.0835265683646154,11.4728541727075,
48.5199460669665));
#31931=CARTESIAN_POINT('Ctrl Pts',(0.0835265683646867,11.4942063411577,
48.5199465324602));
#31932=CARTESIAN_POINT('Ctrl Pts',(0.0835265683659855,11.5200575082527,
48.5195892904601));
#31933=CARTESIAN_POINT('Ctrl Pts',(0.0835265683637358,11.5731362269332,
48.5213546907495));
#31934=CARTESIAN_POINT('Ctrl Pts',(0.0835265683629213,11.5876793312944,
48.5199317919394));
#31935=CARTESIAN_POINT('Ctrl Pts',(0.0835265683619702,11.6131136241746,
48.5199317919394));
#31936=CARTESIAN_POINT('Ctrl Pts',(-0.267518736923682,11.47819221482,48.5199461833397));
#31937=CARTESIAN_POINT('Ctrl Pts',(-0.189316787738642,11.4971000233706,
48.519886961282));
#31938=CARTESIAN_POINT('Ctrl Pts',(-0.189103448006821,11.5200113925673,
48.519586959612));
#31939=CARTESIAN_POINT('Ctrl Pts',(-0.227816669701683,11.5731490589916,
48.5213559145826));
#31940=CARTESIAN_POINT('Ctrl Pts',(-0.266743231125736,11.5876793312944,
48.5199317919394));
#31941=CARTESIAN_POINT('Ctrl Pts',(-0.266821084249534,11.6131136241746,
48.5199317919394));
#31942=CARTESIAN_POINT('Ctrl Pts',(-0.618388066296979,11.4874426767151,
48.5184889915183));
#31943=CARTESIAN_POINT('Ctrl Pts',(-0.484920402710071,11.5031786713302,
48.5195752074935));
#31944=CARTESIAN_POINT('Ctrl Pts',(-0.484557203618662,11.524500508176,48.5196902430683));
#31945=CARTESIAN_POINT('Ctrl Pts',(-0.550623003964169,11.5776504745526,
48.5214911613193));
#31946=CARTESIAN_POINT('Ctrl Pts',(-0.617052003398677,11.5930695682598,
48.5199317919388));
#31947=CARTESIAN_POINT('Ctrl Pts',(-0.617168736861038,11.6169153282063,
48.5199317919388));
#31948=CARTESIAN_POINT('Ctrl Pts',(-1.31980082625865,11.5143737377389,48.5151613829986));
#31949=CARTESIAN_POINT('Ctrl Pts',(-1.12748086026437,11.5255419633077,48.5183112784636));
#31950=CARTESIAN_POINT('Ctrl Pts',(-1.1269213087647,11.5448479357173,48.5193460059348));
#31951=CARTESIAN_POINT('Ctrl Pts',(-1.22201691763213,11.5959692446121,48.5214366576314));
#31952=CARTESIAN_POINT('Ctrl Pts',(-1.31767207799737,11.6126245374907,48.5199317919371));
#31953=CARTESIAN_POINT('Ctrl Pts',(-1.31778153573108,11.6321221443329,48.5199317919372));
#31954=CARTESIAN_POINT('Ctrl Pts',(-1.67034425684702,11.5320543368675,48.5132909663004));
#31955=CARTESIAN_POINT('Ctrl Pts',(-1.47443454802356,11.5418711528743,48.517374142432));
#31956=CARTESIAN_POINT('Ctrl Pts',(-1.47382850347521,11.5607507931985,48.5189135245549));
#31957=CARTESIAN_POINT('Ctrl Pts',(-1.57060291962576,11.609808871885,48.5212544268116));
#31958=CARTESIAN_POINT('Ctrl Pts',(-1.66798338032313,11.6267892697563,48.5199317919361));
#31959=CARTESIAN_POINT('Ctrl Pts',(-1.66804668198961,11.6435272564279,48.5199317919363));
#31960=CARTESIAN_POINT('Ctrl Pts',(-2.72152478000237,11.5986492866067,48.5108119661587));
#31961=CARTESIAN_POINT('Ctrl Pts',(-2.60108318318851,11.612020620858,48.5172046544326));
#31962=CARTESIAN_POINT('Ctrl Pts',(-2.60045731731407,11.6290600690797,48.5194534619891));
#31963=CARTESIAN_POINT('Ctrl Pts',(-2.6593197052731,11.6658592241824,48.5212339924693));
#31964=CARTESIAN_POINT('Ctrl Pts',(-2.71880795910599,11.6794362415569,48.5199317919341));
#31965=CARTESIAN_POINT('Ctrl Pts',(-2.7185946017063,11.689147704808,48.5199317919344));
#31966=CARTESIAN_POINT('Ctrl Pts',(-3.42379713716555,11.6392592214936,48.5061181031666));
#31967=CARTESIAN_POINT('Ctrl Pts',(-3.35185488688305,11.6580360440914,48.5141149281055));
#31968=CARTESIAN_POINT('Ctrl Pts',(-3.35085409224963,11.678564828469,48.5175683502973));
#31969=CARTESIAN_POINT('Ctrl Pts',(-3.38453260249245,11.7135824344713,48.5204767822116));
#31970=CARTESIAN_POINT('Ctrl Pts',(-3.4192119073687,11.728071256096,48.5199317919341));
#31971=CARTESIAN_POINT('Ctrl Pts',(-3.41862985610554,11.734768153188,48.5199317919344));
#31972=CARTESIAN_POINT('Ctrl Pts',(-4.12551258849121,11.6756605207398,48.4959174422581));
#31973=CARTESIAN_POINT('Ctrl Pts',(-4.12419588877397,11.6996409410726,48.5059136087032));
#31974=CARTESIAN_POINT('Ctrl Pts',(-4.12290068805218,11.7229366511894,48.5119171961235));
#31975=CARTESIAN_POINT('Ctrl Pts',(-4.12038695498645,11.7642258753786,48.5189262877417));
#31976=CARTESIAN_POINT('Ctrl Pts',(-4.11916842264252,11.7822193894509,48.5199317919394));
#31977=CARTESIAN_POINT('Ctrl Pts',(-4.11800505968102,11.7955954176946,48.5199317919394));
#31978=CARTESIAN_POINT('Origin',(-4.11644600935663,11.7956965877495,48.2062629115074));
#31979=CARTESIAN_POINT('Ctrl Pts',(-21.3521680276115,16.1705954176947,48.5199317919394));
#31980=CARTESIAN_POINT('Ctrl Pts',(-21.3521680276115,16.4830954176946,48.5199317919395));
#31981=CARTESIAN_POINT('Ctrl Pts',(-21.3521680276115,16.4830954176946,48.8324317919394));
#31982=CARTESIAN_POINT('Ctrl Pts',(-21.5512737421848,16.208004907791,48.5199317919394));
#31983=CARTESIAN_POINT('Ctrl Pts',(-21.5400855159438,16.4830954176967,48.5552391421598));
#31984=CARTESIAN_POINT('Ctrl Pts',(-21.566494676323,16.4830954176946,48.8324317919409));
#31985=CARTESIAN_POINT('Ctrl Pts',(-21.7482599692405,16.2453260884686,48.5124525747896));
#31986=CARTESIAN_POINT('Ctrl Pts',(-21.7441579658526,16.4830954176946,48.5744206138524));
#31987=CARTESIAN_POINT('Ctrl Pts',(-21.7789938361076,16.4830954176946,48.8174733646386));
#31988=CARTESIAN_POINT('Ctrl Pts',(-22.1369289600096,16.3195276817375,48.4785758857753));
#31989=CARTESIAN_POINT('Ctrl Pts',(-22.1478705006132,16.4830954176946,48.5687045084598));
#31990=CARTESIAN_POINT('Ctrl Pts',(-22.1991140172779,16.4830954176946,48.7497199726123));
#31991=CARTESIAN_POINT('Ctrl Pts',(-22.3313759293136,16.3569498947407,48.4529336183403));
#31992=CARTESIAN_POINT('Ctrl Pts',(-22.3540938889857,16.4830954176935,48.5488684947966));
#31993=CARTESIAN_POINT('Ctrl Pts',(-22.4101480350136,16.4830954176946,48.6982467590681));
#31994=CARTESIAN_POINT('Ctrl Pts',(-22.5100610938555,16.3915662868148,48.4076054027924));
#31995=CARTESIAN_POINT('Ctrl Pts',(-22.548826372816,16.4830954176946,48.4905200272361));
#31996=CARTESIAN_POINT('Ctrl Pts',(-22.6036487560711,16.4830954176946,48.6077790136438));
#31997=CARTESIAN_POINT('Ctrl Pts',(-22.510061093855,16.3915662868147,48.4076054027925));
#31998=CARTESIAN_POINT('Ctrl Pts',(-22.470838026846,16.3839676712791,48.4175553780106));
#31999=CARTESIAN_POINT('Ctrl Pts',(-22.4313616813393,16.3763319926636,48.4264324211722));
#32000=CARTESIAN_POINT('Ctrl Pts',(-22.3917296389681,16.3686778876786,48.4344340496838));
#32001=CARTESIAN_POINT('Ctrl Pts',(-22.3479890308505,16.3602302986418,48.4432651892387));
#32002=CARTESIAN_POINT('Ctrl Pts',(-22.3040585025035,16.3517602066229,48.451029983322));
#32003=CARTESIAN_POINT('Ctrl Pts',(-22.2600230793043,16.3432839722933,48.4579483574562));
#32004=CARTESIAN_POINT('Ctrl Pts',(-22.2124872920991,16.3341339643652,48.4654166712991));
#32005=CARTESIAN_POINT('Ctrl Pts',(-22.1648284589081,16.3249766329791,48.4718982624129));
#32006=CARTESIAN_POINT('Ctrl Pts',(-22.1171112171318,16.3158247537685,48.4776226213431));
#32007=CARTESIAN_POINT('Ctrl Pts',(-22.0590026864533,16.3046798880117,48.4845935625403));
#32008=CARTESIAN_POINT('Ctrl Pts',(-22.0008060837811,16.2935427876858,48.4904415667607));
#32009=CARTESIAN_POINT('Ctrl Pts',(-21.942594596444,16.2824290454294,48.4955150476558));
#32010=CARTESIAN_POINT('Ctrl Pts',(-21.9397573875572,16.2818873652605,48.4957623274581));
#32011=CARTESIAN_POINT('Ctrl Pts',(-21.9369195504994,16.2813456246244,48.4960075961641));
#32012=CARTESIAN_POINT('Ctrl Pts',(-21.9340810451365,16.28080381591,48.496250863188));
#32013=CARTESIAN_POINT('Ctrl Pts',(-21.8165634625776,16.2583722745907,48.5063224145554));
#32014=CARTESIAN_POINT('Ctrl Pts',(-21.6987927520804,16.2359974208102,48.5128922231434));
#32015=CARTESIAN_POINT('Ctrl Pts',(-21.5808083365145,16.21368980715,48.5165038490348));
#32016=CARTESIAN_POINT('Ctrl Pts',(-21.5046957442586,16.199299005665,48.5188337347873));
#32017=CARTESIAN_POINT('Ctrl Pts',(-21.4284939067714,16.1849361189809,48.5199313850954));
#32018=CARTESIAN_POINT('Ctrl Pts',(-21.3522104186698,16.1706033824526,48.5199317918264));
#32019=CARTESIAN_POINT('Ctrl Pts',(-22.754424611923,16.495117042058,48.4071618265161));
#32020=CARTESIAN_POINT('Ctrl Pts',(-22.7176017202102,16.581294338131,48.5199317919394));
#32021=CARTESIAN_POINT('Ctrl Pts',(-22.6599908629307,16.7161293328258,48.5199317919394));
#32022=CARTESIAN_POINT('Ctrl Pts',(-19.765550405457,15.2224248747711,48.4119403012087));
#32023=CARTESIAN_POINT('Ctrl Pts',(-19.7460226280874,15.3157731528558,48.5199317919394));
#32024=CARTESIAN_POINT('Ctrl Pts',(-19.6812252681849,15.4434377928151,48.5199317919394));
#32025=CARTESIAN_POINT('Ctrl Pts',(-16.7040650491873,14.1211388855287,48.4164308930203));
#32026=CARTESIAN_POINT('Ctrl Pts',(-16.6858002353668,14.2126904029842,48.5199317919394));
#32027=CARTESIAN_POINT('Ctrl Pts',(-16.6312111874939,14.3421540083754,48.5199317919394));
#32028=CARTESIAN_POINT('Ctrl Pts',(-11.9808374649863,12.8451845281724,48.4218608844626));
#32029=CARTESIAN_POINT('Ctrl Pts',(-11.9616626207849,12.9358419174536,48.5199317919394));
#32030=CARTESIAN_POINT('Ctrl Pts',(-11.9272425168244,13.0661994464424,48.5199317919394));
#32031=CARTESIAN_POINT('Ctrl Pts',(-10.3932306187778,12.4841939488199,48.4234426080441));
#32032=CARTESIAN_POINT('Ctrl Pts',(-10.3759657149212,12.5748700381561,48.5199317919394));
#32033=CARTESIAN_POINT('Ctrl Pts',(-10.3463554047103,12.7052089420493,48.5199317919394));
#32034=CARTESIAN_POINT('Ctrl Pts',(-7.1674989354977,11.9034070977967,48.4260232871746));
#32035=CARTESIAN_POINT('Ctrl Pts',(-7.15598924266794,11.9947391304937,48.5199317919394));
#32036=CARTESIAN_POINT('Ctrl Pts',(-7.13465594337445,12.1244225185051,48.5199317919394));
#32037=CARTESIAN_POINT('Ctrl Pts',(-5.52308711228244,11.6863323981099,48.4270102837803));
#32038=CARTESIAN_POINT('Ctrl Pts',(-5.51351080050052,11.7776141640752,48.5199317919394));
#32039=CARTESIAN_POINT('Ctrl Pts',(-5.49759056885458,11.9073477673264,48.5199317919394));
#32040=CARTESIAN_POINT('Ctrl Pts',(-3.87138954853958,11.5522837202171,48.4276218721885));
#32041=CARTESIAN_POINT('Ctrl Pts',(-3.86394066580964,11.6436417565348,48.5199317919394));
#32042=CARTESIAN_POINT('Ctrl Pts',(-3.85336951301254,11.7732992268532,48.5199317919394));
#32043=CARTESIAN_POINT('Origin',(44.4585265683622,-14.4544045823054,-44.2925682080604));
#32044=CARTESIAN_POINT('Origin',(49.7710265683622,-14.4544045823054,-44.2925682080604));
#32045=CARTESIAN_POINT('Origin',(44.4585265683622,-14.4544045823054,-49.6050682080604));
#32046=CARTESIAN_POINT('Origin',(0.0835265683620477,-14.4544045823054,-49.6050682080606));
#32047=CARTESIAN_POINT('Origin',(-44.2914734316379,-14.4544045823054,-49.6050682080606));
#32048=CARTESIAN_POINT('Origin',(49.7710265683621,-14.4544045823054,0.0824317919395964));
#32049=CARTESIAN_POINT('Origin',(49.7710265683619,-14.4544045823054,36.6697170232579));
#32050=CARTESIAN_POINT('Origin',(-44.291473431638,-14.4544045823054,-44.2925682080606));
#32051=CARTESIAN_POINT('Origin',(-49.603973431638,-14.4544045823054,-44.2925682080605));
#32052=CARTESIAN_POINT('Origin',(44.4585265683621,-14.4544045823054,44.4574317919394));
#32053=CARTESIAN_POINT('Origin',(44.458526568362,-14.4544045823054,49.7699317919394));
#32054=CARTESIAN_POINT('Origin',(-49.603973431638,-14.4544045823054,0.0824317919394229));
#32055=CARTESIAN_POINT('Origin',(-49.603973431638,-14.4544045823054,44.4574317919389));
#32056=CARTESIAN_POINT('Origin',(0.0835265683620476,-14.4544045823054,49.7699317919394));
#32057=CARTESIAN_POINT('Origin',(-44.2914734316384,-14.4544045823054,49.7699317919394));
#32058=CARTESIAN_POINT('Origin',(-44.2914734316384,-14.4544045823054,44.457431791939));
#32059=CARTESIAN_POINT('Origin',(44.4585265683622,16.1705954176946,-44.2925682080604));
#32060=CARTESIAN_POINT('Origin',(49.7710265683622,16.1705954176946,-44.2925682080604));
#32061=CARTESIAN_POINT('Origin',(44.4585265683622,16.1705954176946,-49.6050682080604));
#32062=CARTESIAN_POINT('Origin',(-44.291473431638,16.1705954176946,-49.6050682080606));
#32063=CARTESIAN_POINT('Origin',(-44.2914734316379,16.1705954176946,-49.6050682080606));
#32064=CARTESIAN_POINT('Origin',(49.7710265683622,16.1705954176946,-44.2925682080603));
#32065=CARTESIAN_POINT('Origin',(49.7710265683619,16.1705954176946,36.6697170232579));
#32066=CARTESIAN_POINT('Origin',(-44.291473431638,16.1705954176946,-44.2925682080606));
#32067=CARTESIAN_POINT('Origin',(-49.603973431638,16.1705954176946,-44.2925682080605));
#32068=CARTESIAN_POINT('Origin',(44.4585265683621,16.1705954176946,44.4574317919394));
#32069=CARTESIAN_POINT('Origin',(44.458526568362,16.1705954176946,49.7699317919394));
#32070=CARTESIAN_POINT('Origin',(-49.603973431638,16.1705954176946,-44.2925682080606));
#32071=CARTESIAN_POINT('Origin',(-49.603973431638,16.1705954176946,44.4574317919389));
#32072=CARTESIAN_POINT('Origin',(-44.2914734316379,16.1705954176946,49.7699317919394));
#32073=CARTESIAN_POINT('Origin',(-44.2914734316384,16.1705954176946,49.7699317919394));
#32074=CARTESIAN_POINT('Origin',(-44.2914734316384,16.1705954176946,44.457431791939));
#32075=CARTESIAN_POINT('Origin',(44.4585265683621,16.1705954176946,44.4574317919394));
#32076=CARTESIAN_POINT('Origin',(41.173224139993,16.1705954176946,46.8471376742924));
#32077=CARTESIAN_POINT('Origin',(40.162361854341,16.1705954176946,47.5824317919394));
#32078=CARTESIAN_POINT('Origin',(40.162361854341,16.1705954176946,48.8324317919394));
#32079=CARTESIAN_POINT('Origin',(48.8335265683621,16.1705954176946,42.8336341598436));
#32080=CARTESIAN_POINT('Origin',(48.8335265683621,16.1705954176946,35.8884670232579));
#32081=CARTESIAN_POINT('Origin',(48.8335265683621,16.1705954176946,29.6248403980433));
#32082=CARTESIAN_POINT('Origin',(26.1374820022305,16.1705954176946,48.8324317919394));
#32083=CARTESIAN_POINT('Origin',(29.625935174466,16.1705954176946,48.8324317919394));
#32084=CARTESIAN_POINT('Origin',(47.583526568362,16.1705954176946,29.6248403980433));
#32085=CARTESIAN_POINT('Origin',(46.5220740543956,16.1705954176946,28.9646748425997));
#32086=CARTESIAN_POINT('Origin',(29.625935174466,16.1705954176946,47.5824317919394));
#32087=CARTESIAN_POINT('Origin',(28.9657696190223,16.1705954176946,46.5209792779729));
#32088=CARTESIAN_POINT('Origin',(0.0835265683620477,16.1705954176946,0.0824317919394229));
#32089=CARTESIAN_POINT('Origin',(44.4585265683621,15.8580954176946,44.4574317919394));
#32090=CARTESIAN_POINT('Origin',(40.667792997167,15.8580954176946,47.2147847331159));
#32091=CARTESIAN_POINT('Origin',(40.162361854341,15.8580954176946,47.5824317919394));
#32092=CARTESIAN_POINT('Origin',(40.162361854341,15.8580954176946,48.2074317919394));
#32093=CARTESIAN_POINT('Origin',(48.2085265683621,15.8580954176946,0.0824317919394229));
#32094=CARTESIAN_POINT('Origin',(48.2085265683621,15.8580954176946,35.8884670232579));
#32095=CARTESIAN_POINT('Origin',(48.2085265683621,15.8580954176946,29.6248403980433));
#32096=CARTESIAN_POINT('Origin',(0.0835265683619977,15.8580954176946,48.2074317919394));
#32097=CARTESIAN_POINT('Origin',(29.625935174466,15.8580954176946,48.2074317919394));
#32098=CARTESIAN_POINT('Origin',(47.583526568362,15.8580954176946,29.6248403980433));
#32099=CARTESIAN_POINT('Origin',(47.0528003113788,15.8580954176946,29.2947576203215));
#32100=CARTESIAN_POINT('Origin',(29.625935174466,15.8580954176946,47.5824317919394));
#32101=CARTESIAN_POINT('Origin',(29.2958523967441,15.8580954176946,47.0517055349562));
#32102=CARTESIAN_POINT('Origin',(0.0835265683620477,15.8580954176946,0.0824317919394229));
#32103=CARTESIAN_POINT('Origin',(40.1623618543411,16.1705954176946,-47.4175682080604));
#32104=CARTESIAN_POINT('Origin',(40.1623618543411,16.1705954176946,-48.6675682080604));
#32105=CARTESIAN_POINT('Origin',(47.5835265683622,16.1705954176946,-39.9964034940393));
#32106=CARTESIAN_POINT('Origin',(48.8335265683622,16.1705954176946,-39.9964034940393));
#32107=CARTESIAN_POINT('Origin',(42.8347289362664,16.1705954176946,-48.6675682080604));
#32108=CARTESIAN_POINT('Origin',(29.6259351744661,16.1705954176946,-48.6675682080605));
#32109=CARTESIAN_POINT('Origin',(48.8335265683621,16.1705954176946,-25.9715236419289));
#32110=CARTESIAN_POINT('Origin',(29.6259351744661,16.1705954176946,-47.4175682080605));
#32111=CARTESIAN_POINT('Origin',(28.9657696190224,16.1705954176946,-46.356115694094));
#32112=CARTESIAN_POINT('Origin',(0.0835265683620477,16.1705954176946,0.0824317919394229));
#32113=CARTESIAN_POINT('Origin',(40.1623618543411,15.8580954176946,-47.4175682080604));
#32114=CARTESIAN_POINT('Origin',(40.1623618543411,15.8580954176946,-48.0425682080604));
#32115=CARTESIAN_POINT('Origin',(47.5835265683622,15.8580954176946,-39.9964034940393));
#32116=CARTESIAN_POINT('Origin',(48.2085265683622,15.8580954176946,-39.9964034940393));
#32117=CARTESIAN_POINT('Origin',(0.0835265683622157,15.8580954176946,-48.0425682080606));
#32118=CARTESIAN_POINT('Origin',(29.6259351744661,15.8580954176946,-48.0425682080605));
#32119=CARTESIAN_POINT('Origin',(48.208526568362,15.8580954176946,0.0824317919396409));
#32120=CARTESIAN_POINT('Origin',(29.6259351744661,15.8580954176946,-47.4175682080605));
#32121=CARTESIAN_POINT('Origin',(29.2958523967443,15.8580954176946,-46.8868419510772));
#32122=CARTESIAN_POINT('Origin',(0.0835265683620477,15.8580954176946,0.0824317919394229));
#32123=CARTESIAN_POINT('Origin',(-47.4164734316379,16.1705954176946,-39.9964034940395));
#32124=CARTESIAN_POINT('Origin',(-48.6664734316379,16.1705954176946,-39.9964034940395));
#32125=CARTESIAN_POINT('Origin',(-39.9953087176169,16.1705954176946,-47.4175682080606));
#32126=CARTESIAN_POINT('Origin',(-39.9953087176169,16.1705954176946,-48.6675682080606));
#32127=CARTESIAN_POINT('Origin',(-48.6664734316379,16.1705954176946,-42.6687705759647));
#32128=CARTESIAN_POINT('Origin',(-25.9704288655064,16.1705954176946,-48.6675682080606));
#32129=CARTESIAN_POINT('Origin',(-29.4588820377419,16.1705954176946,-48.6675682080606));
#32130=CARTESIAN_POINT('Origin',(-29.4588820377419,16.1705954176946,-47.4175682080606));
#32131=CARTESIAN_POINT('Origin',(-28.7987164822982,16.1705954176946,-46.3561156940941));
#32132=CARTESIAN_POINT('Origin',(0.0835265683620477,16.1705954176946,0.0824317919394229));
#32133=CARTESIAN_POINT('Origin',(-47.4164734316379,15.8580954176946,-39.9964034940395));
#32134=CARTESIAN_POINT('Origin',(-48.0414734316379,15.8580954176946,-39.9964034940395));
#32135=CARTESIAN_POINT('Origin',(-39.9953087176169,15.8580954176946,-47.4175682080606));
#32136=CARTESIAN_POINT('Origin',(-39.9953087176169,15.8580954176946,-48.0425682080606));
#32137=CARTESIAN_POINT('Origin',(-48.0414734316379,15.8580954176946,0.0824317919394229));
#32138=CARTESIAN_POINT('Origin',(0.0835265683620977,15.8580954176946,-48.0425682080605));
#32139=CARTESIAN_POINT('Origin',(-29.4588820377419,15.8580954176946,-48.0425682080606));
#32140=CARTESIAN_POINT('Origin',(-29.4588820377419,15.8580954176946,-47.4175682080606));
#32141=CARTESIAN_POINT('Origin',(-29.1287992600201,15.8580954176946,-46.8868419510773));
#32142=CARTESIAN_POINT('Origin',(0.0835265683620477,15.8580954176946,0.0824317919394229));
#32143=CARTESIAN_POINT('Origin',(0.0835265683620477,-12.5794045823054,0.0824317919394229));
#32144=CARTESIAN_POINT('',(7.59696574233659,-12.5794045823054,18.6174859267129));
#32145=CARTESIAN_POINT('',(-6.17974956131282,-12.5794045823054,19.076414315977));
#32146=CARTESIAN_POINT('Origin',(-5.38208978662056,-12.5794045823054,16.6574349341085));
#32147=CARTESIAN_POINT('',(7.67510093260532,-12.5794045823054,20.9630507178886));
#32148=CARTESIAN_POINT('',(15.3925785990455,-12.5794045823054,23.5078932009404));
#32149=CARTESIAN_POINT('Origin',(-6.17974956131282,-12.5794045823054,19.076414315977));
#32150=CARTESIAN_POINT('',(46.9585265683621,-12.5794045823054,36.5987899438301));
#32151=CARTESIAN_POINT('',(14.5949188243533,-17.1192738307565,25.9268725828089));
#32152=CARTESIAN_POINT('',(44.4818701996542,-11.3294045823054,35.7821111511702));
#32153=CARTESIAN_POINT('',(16.3756046859818,-11.3294045823054,26.5140547199659));
#32154=CARTESIAN_POINT('',(44.4818701996542,17.4534666579714,35.7821111511702));
#32155=CARTESIAN_POINT('Origin',(8.06655569071,-12.5794045823054,19.7759268101363));
#32156=CARTESIAN_POINT('Origin',(0.0835265683620477,-11.3294045823054,0.0824317919394229));
#32157=CARTESIAN_POINT('Origin',(0.0835265683620477,-10.0794045823054,0.0824317919394229));
#32158=CARTESIAN_POINT('Origin',(0.0835265683620477,-14.4544045823054,0.0824317919394229));
#32159=CARTESIAN_POINT('Origin',(17.9541833518389,-17.1192738307565,25.7183855703182));
#32160=CARTESIAN_POINT('',(18.353013239185,-11.3294045823054,24.508895879384));
#32161=CARTESIAN_POINT('',(18.353013239185,-11.3294045823054,24.508895879384));
#32162=CARTESIAN_POINT('',(18.353013239185,-11.3294045823054,24.508895879384));
#32163=CARTESIAN_POINT('Origin',(14.5949188243533,-17.1192738307565,25.9268725828089));
#32164=CARTESIAN_POINT('Origin',(48.8335265683621,-11.3294045823054,37.2170722197182));
#32165=CARTESIAN_POINT('',(48.8335265683621,21.5220065103812,36.6697170232579));
#32166=CARTESIAN_POINT('',(48.8335265683621,-11.3294045823054,34.5598618267976));
#32167=CARTESIAN_POINT('Origin',(48.8335265683621,-11.3294045823054,34.5598618267976));
#32168=CARTESIAN_POINT('',(45.272154845105,-11.3294045823054,33.3854975524836));
#32169=CARTESIAN_POINT('',(45.272154845105,17.4534666579714,33.3854975524836));
#32170=CARTESIAN_POINT('',(48.8335265683621,-11.3294045823054,34.5598618267976));
#32171=CARTESIAN_POINT('Origin',(16.7670594440865,-11.3294045823054,25.3269308122136));
#32172=CARTESIAN_POINT('',(44.4818701996542,-11.3294045823054,35.7821111511702));
#32173=CARTESIAN_POINT('Origin',(0.0835265683620477,21.5220065103812,37.6072170232579));
#32174=CARTESIAN_POINT('',(48.8335265683621,21.5220065103812,37.6072170232579));
#32175=CARTESIAN_POINT('Origin',(48.8335265683619,21.5220065103812,0.0824317919392537));
#32176=CARTESIAN_POINT('',(48.8335265683621,21.5220065103812,38.3884670232579));
#32177=CARTESIAN_POINT('Origin',(46.9585265683619,21.5220065103812,0.0824317919392602));
#32178=CARTESIAN_POINT('',(46.9585265683621,21.5220065103812,38.3884670232579));
#32179=CARTESIAN_POINT('Origin',(0.0835265683620477,21.5220065103812,36.6697170232579));
#32180=CARTESIAN_POINT('Origin',(0.0835265683620477,21.5220065103812,38.3884670232579));
#32181=CARTESIAN_POINT('Origin',(0.0835265683620477,21.5220065103812,37.6072170232579));
#32182=CARTESIAN_POINT('',(48.8335265683621,21.5220065103812,37.6072170232579));
#32183=CARTESIAN_POINT('Origin',(48.8335265683619,21.5220065103812,0.0824317919392537));
#32184=CARTESIAN_POINT('',(48.8335265683621,21.5220065103812,38.3884670232579));
#32185=CARTESIAN_POINT('Origin',(0.0835265683620477,21.5220065103812,38.3884670232579));
#32186=CARTESIAN_POINT('',(46.9585265683621,21.5220065103812,38.3884670232579));
#32187=CARTESIAN_POINT('Origin',(0.0835265683620477,21.5220065103812,36.6697170232579));
#32188=CARTESIAN_POINT('',(48.8335265683621,21.5220065103812,36.6697170232579));
#32189=CARTESIAN_POINT('Origin',(48.8335265683619,21.5220065103812,0.0824317919392537));
#32190=CARTESIAN_POINT('',(48.8335265683621,21.5220065103812,35.8884670232579));
#32191=CARTESIAN_POINT('Origin',(0.0835265683620477,21.5220065103812,35.8884670232579));
#32192=CARTESIAN_POINT('',(46.958526568362,21.5220065103812,35.8884670232579));
#32193=CARTESIAN_POINT('Origin',(46.9585265683619,21.5220065103812,0.0824317919392602));
#32194=CARTESIAN_POINT('Origin',(44.4818701996542,17.4534666579714,35.7821111511702));
#32195=CARTESIAN_POINT('',(0.,0.,0.));
#32196=CARTESIAN_POINT('Origin',(7.5111559719605E-6,20.2903503023534,4.07573877568452E-6));
#32197=CARTESIAN_POINT('',(7.51115596928158E-6,-3.14714969764662,21.8750040757388));
#32198=CARTESIAN_POINT('Origin',(7.5111559719605E-6,-3.14714969764662,4.07573877568452E-6));
#32199=CARTESIAN_POINT('',(7.51113043071691E-6,-0.359077263140675,21.8750040757388));
#32200=CARTESIAN_POINT('',(7.51115596928158E-6,20.2903503023534,21.8750040757388));
#32201=CARTESIAN_POINT('',(-11.6286532108092,17.7903562366901,18.528087484808));
#32202=CARTESIAN_POINT('Ctrl Pts',(7.51110489222162E-6,-0.359077263140676,
21.8750040757388));
#32203=CARTESIAN_POINT('Ctrl Pts',(-0.242521808837313,0.787240620602144,
21.8750040757382));
#32204=CARTESIAN_POINT('Ctrl Pts',(-0.54540759357386,1.9195211595413,21.8714101784102));
#32205=CARTESIAN_POINT('Ctrl Pts',(-1.59847036445218,5.0559408312384,21.8271017536525));
#32206=CARTESIAN_POINT('Ctrl Pts',(-2.48649791511479,6.94231008337416,21.7624093403727));
#32207=CARTESIAN_POINT('Ctrl Pts',(-4.68929447542434,10.5092773155408,21.3951090797112));
#32208=CARTESIAN_POINT('Ctrl Pts',(-5.95096816574499,12.119347275553,21.0995416323438));
#32209=CARTESIAN_POINT('Ctrl Pts',(-8.70650705890375,15.1447845037697,20.1220819188374));
#32210=CARTESIAN_POINT('Ctrl Pts',(-10.1763293042647,16.5261427053452,19.4396001110593));
#32211=CARTESIAN_POINT('Ctrl Pts',(-11.6286532108092,17.7903562366901,18.528087484808));
#32212=CARTESIAN_POINT('',(-21.6029109448944,17.7903503023534,3.43941378980876));
#32213=CARTESIAN_POINT('Origin',(7.5111559719605E-6,17.7903503023534,4.07573877568452E-6));
#32214=CARTESIAN_POINT('',(-16.8093026954431,-3.07550340054456,13.9986724319706));
#32215=CARTESIAN_POINT('Ctrl Pts',(-21.6029109448944,17.7903503023534,3.43941378980876));
#32216=CARTESIAN_POINT('Ctrl Pts',(-21.3273236992784,16.6048563822885,5.17037616111758));
#32217=CARTESIAN_POINT('Ctrl Pts',(-20.8613902773445,15.2608755267349,6.74246896531775));
#32218=CARTESIAN_POINT('Ctrl Pts',(-19.7942016810054,12.2596276657995,9.41879827256646));
#32219=CARTESIAN_POINT('Ctrl Pts',(-19.2123581961323,10.6436381400427,10.5083820514703));
#32220=CARTESIAN_POINT('Ctrl Pts',(-18.1533883573703,7.04932465914044,12.2482184494194));
#32221=CARTESIAN_POINT('Ctrl Pts',(-17.7057831864294,5.15107554627117,12.856864075177));
#32222=CARTESIAN_POINT('Ctrl Pts',(-17.0634858899474,1.10319626289942,13.6979815703421));
#32223=CARTESIAN_POINT('Ctrl Pts',(-16.8802985444201,-0.980646982039156,
13.9134220807907));
#32224=CARTESIAN_POINT('Ctrl Pts',(-16.8093024574423,-3.07550338138541,
13.9986727045614));
#32225=CARTESIAN_POINT('',(-21.7361818719648,17.7903503023534,2.46043007566383));
#32226=CARTESIAN_POINT('Ctrl Pts',(-16.809302912983,-3.07550344707786,13.9986721575575));
#32227=CARTESIAN_POINT('Ctrl Pts',(-16.9860508960446,-0.997639372661501,
13.7864368436865));
#32228=CARTESIAN_POINT('Ctrl Pts',(-17.2665397063309,1.04520175631502,13.4472040857416));
#32229=CARTESIAN_POINT('Ctrl Pts',(-18.0609524981394,5.05250922301929,12.3603585968672));
#32230=CARTESIAN_POINT('Ctrl Pts',(-18.5636987886872,6.93818763618362,11.6263456265167));
#32231=CARTESIAN_POINT('Ctrl Pts',(-19.6498492391718,10.5055771888037,9.67592682088231));
#32232=CARTESIAN_POINT('Ctrl Pts',(-20.2057076270334,12.116505550095,8.50500890855202));
#32233=CARTESIAN_POINT('Ctrl Pts',(-21.16013987792,15.143532030257,5.74031484751266));
#32234=CARTESIAN_POINT('Ctrl Pts',(-21.5432335765096,16.525560671386,4.16499696419982));
#32235=CARTESIAN_POINT('Ctrl Pts',(-21.7361818719648,17.7903503023534,2.46043007566384));
#32236=CARTESIAN_POINT('',(-16.1582306321435,17.7903503023534,-14.7454008052546));
#32237=CARTESIAN_POINT('Origin',(7.5111559719605E-6,17.7903503023534,4.07573877568452E-6));
#32238=CARTESIAN_POINT('',(-21.4250256124694,-3.07550340054456,-4.41401688263851));
#32239=CARTESIAN_POINT('Ctrl Pts',(-16.1582306321435,17.7903503023534,-14.7454008052546));
#32240=CARTESIAN_POINT('Ctrl Pts',(-17.3397256718364,16.6048563822885,-13.4507006345531));
#32241=CARTESIAN_POINT('Ctrl Pts',(-18.2783325826005,15.2608755267349,-12.1062353855568));
#32242=CARTESIAN_POINT('Ctrl Pts',(-19.7053898859821,12.2596276657995,-9.60320971372281));
#32243=CARTESIAN_POINT('Ctrl Pts',(-20.1944873080192,10.6436381400427,-8.46896178496286));
#32244=CARTESIAN_POINT('Ctrl Pts',(-20.8944892833356,7.04932465914048,-6.55625557501076));
#32245=CARTESIAN_POINT('Ctrl Pts',(-21.0912703358785,5.15107554627125,-5.8268194200479));
#32246=CARTESIAN_POINT('Ctrl Pts',(-21.3484166599352,1.10319626289929,-4.8002229921537));
#32247=CARTESIAN_POINT('Ctrl Pts',(-21.402639391837,-0.980646982039869,
-4.5226763970588));
#32248=CARTESIAN_POINT('Ctrl Pts',(-21.4250256771985,-3.07550338138541,
-4.41401652660439));
#32249=CARTESIAN_POINT('',(-15.4759234075142,17.7903503023534,-15.4599825736911));
#32250=CARTESIAN_POINT('Ctrl Pts',(-21.4250255335586,-3.07550344707786,
-4.41401722381183));
#32251=CARTESIAN_POINT('Ctrl Pts',(-21.3692938484207,-0.997639372661258,
-4.68453091522497));
#32252=CARTESIAN_POINT('Ctrl Pts',(-21.2789529111239,1.04520175631505,-5.11533406262186));
#32253=CARTESIAN_POINT('Ctrl Pts',(-20.9245311655024,5.05250922301919,-6.41406807184237));
#32254=CARTESIAN_POINT('Ctrl Pts',(-20.6641139018212,6.93818763618362,-7.26478055093226));
#32255=CARTESIAN_POINT('Ctrl Pts',(-19.81641880474,10.5055771888037,-9.33003340248447));
#32256=CARTESIAN_POINT('Ctrl Pts',(-19.2475303536038,12.116505550095,-10.4946763670602));
#32257=CARTESIAN_POINT('Ctrl Pts',(-17.6810842722838,15.1435320302569,-12.9646401010037));
#32258=CARTESIAN_POINT('Ctrl Pts',(-16.6883061704418,16.5255606713859,-14.2463494502274));
#32259=CARTESIAN_POINT('Ctrl Pts',(-15.4759234075142,17.7903503023534,-15.4599825736911));
#32260=CARTESIAN_POINT('',(7.51115596928158E-6,17.7903503023534,-21.8749959242612));
#32261=CARTESIAN_POINT('Origin',(7.5111559719605E-6,17.7903503023534,4.07573877568452E-6));
#32262=CARTESIAN_POINT('',(1.45393257050235,17.7903503023534,-21.8266247734858));
#32263=CARTESIAN_POINT('Origin',(7.5111559719605E-6,17.7903503023534,4.07573877568452E-6));
#32264=CARTESIAN_POINT('',(-9.90726159778959,-3.07550341763295,-19.5028583812017));
#32265=CARTESIAN_POINT('Ctrl Pts',(1.45393257050235,17.7903503023534,-21.8266247734858));
#32266=CARTESIAN_POINT('Ctrl Pts',(-0.42071722963709,16.5196076224518,-21.9514997755189));
#32267=CARTESIAN_POINT('Ctrl Pts',(-2.16453839481852,15.0681198554842,-21.822133979092));
#32268=CARTESIAN_POINT('Ctrl Pts',(-5.15083863820302,11.8037205632591,-21.3119549809142));
#32269=CARTESIAN_POINT('Ctrl Pts',(-6.3697426145343,10.0441260470548,-20.9514582684722));
#32270=CARTESIAN_POINT('Ctrl Pts',(-8.15807676202854,6.37804252407538,-20.316195099095));
#32271=CARTESIAN_POINT('Ctrl Pts',(-8.7555204640488,4.59032766603492,-20.0515884547815));
#32272=CARTESIAN_POINT('Ctrl Pts',(-9.59144327553473,0.814270441473194,
-19.6655393452124));
#32273=CARTESIAN_POINT('Ctrl Pts',(-9.8152351985608,-1.12645709600235,-19.5496069154558));
#32274=CARTESIAN_POINT('Ctrl Pts',(-9.90726191550005,-3.07550338999529,
-19.5028582143879));
#32275=CARTESIAN_POINT('',(2.4380266901546,17.7903503023534,-21.7387099497696));
#32276=CARTESIAN_POINT('Ctrl Pts',(2.4380266901546,17.7903503023534,-21.7387099497696));
#32277=CARTESIAN_POINT('Ctrl Pts',(0.519424066437449,16.366911361741,-21.9538832110771));
#32278=CARTESIAN_POINT('Ctrl Pts',(-1.29094448071633,14.7970175900028,-21.8969955147474));
#32279=CARTESIAN_POINT('Ctrl Pts',(-4.46152970952729,11.3236494616448,-21.4731858316244));
#32280=CARTESIAN_POINT('Ctrl Pts',(-5.790993610098,9.47257185931529,-21.12458283065));
#32281=CARTESIAN_POINT('Ctrl Pts',(-7.71013039377804,5.79264830253153,-20.4907332313965));
#32282=CARTESIAN_POINT('Ctrl Pts',(-8.36432873407734,4.10230776867177,-20.2201250966576));
#32283=CARTESIAN_POINT('Ctrl Pts',(-9.35970303244591,0.555960676466445,
-19.7788756473871));
#32284=CARTESIAN_POINT('Ctrl Pts',(-9.69063212779356,-1.24753824725553,
-19.6129040870217));
#32285=CARTESIAN_POINT('Ctrl Pts',(-9.90726128043683,-3.07550344707786,
-19.502858536994));
#32286=CARTESIAN_POINT('',(17.9712605487941,17.7903503023534,-12.4719520361622));
#32287=CARTESIAN_POINT('Origin',(7.5111559719605E-6,17.7903503023534,4.07573877568452E-6));
#32288=CARTESIAN_POINT('',(9.07087812914772,-3.07550340054456,-19.9056466697429));
#32289=CARTESIAN_POINT('Ctrl Pts',(17.9712652714714,17.790355904801,-12.4719452310979));
#32290=CARTESIAN_POINT('Ctrl Pts',(16.9719333168451,16.6048619847361,-13.9119156145767));
#32291=CARTESIAN_POINT('Ctrl Pts',(15.8700315823639,15.2608755267349,-15.1261681583902));
#32292=CARTESIAN_POINT('Ctrl Pts',(13.747312113943,12.2596276657995,-17.074421765953));
#32293=CARTESIAN_POINT('Ctrl Pts',(12.7503365640078,10.6436381400426,-17.8036504029188));
#32294=CARTESIAN_POINT('Ctrl Pts',(11.0413509854407,7.04932465914046,-18.9117190394597));
#32295=CARTESIAN_POINT('Ctrl Pts',(10.3739912214096,5.1510755462712,-19.2658811946362));
#32296=CARTESIAN_POINT('Ctrl Pts',(9.43035414950194,1.10319626289946,-19.7450195194052));
#32297=CARTESIAN_POINT('Ctrl Pts',(9.17183191995736,-0.980646982038627,
-19.859642701768));
#32298=CARTESIAN_POINT('Ctrl Pts',(9.07087779644369,-3.07550338138541,-19.9056468120741));
#32299=CARTESIAN_POINT('',(18.5160986195094,17.7903503023534,-11.6477422756871));
#32300=CARTESIAN_POINT('Ctrl Pts',(9.0708784442078,-3.07550344707787,-19.9056465168923));
#32301=CARTESIAN_POINT('Ctrl Pts',(9.32220832596597,-0.997639372661295,
-19.7911171821972));
#32302=CARTESIAN_POINT('Ctrl Pts',(9.72210758927721,1.04520175631505,-19.6071785621038));
#32303=CARTESIAN_POINT('Ctrl Pts',(10.909413367516,5.05250922301937,-18.9726474049206));
#32304=CARTESIAN_POINT('Ctrl Pts',(11.6808484158895,6.93818763618365,-18.5294580103685));
#32305=CARTESIAN_POINT('Ctrl Pts',(13.5056911618681,10.5055771888038,-17.243454405821));
#32306=CARTESIAN_POINT('Ctrl Pts',(14.5145445062954,12.1165055500951,-16.4296717356873));
#32307=CARTESIAN_POINT('Ctrl Pts',(16.5740140475861,15.143532030257,-14.3528810911652));
#32308=CARTESIAN_POINT('Ctrl Pts',(17.6026743570154,16.5255606713859,-13.0997868476268));
#32309=CARTESIAN_POINT('Ctrl Pts',(18.5160986195094,17.7903503023534,-11.6477422756871));
#32310=CARTESIAN_POINT('',(20.9558684429898,17.7903503023534,6.27435803496356));
#32311=CARTESIAN_POINT('Origin',(7.5111559719605E-6,17.7903503023534,4.07573877568452E-6));
#32312=CARTESIAN_POINT('',(21.2184672672846,-3.07550340054455,-5.31907394089049));
#32313=CARTESIAN_POINT('Ctrl Pts',(20.9558684429898,17.7903503023534,6.27435803496357));
#32314=CARTESIAN_POINT('Ctrl Pts',(21.4586093402341,16.6048563822885,4.59524200232282));
#32315=CARTESIAN_POINT('Ctrl Pts',(21.7209233366826,15.260875526735,2.97667439299652));
#32316=CARTESIAN_POINT('Ctrl Pts',(21.9206354021396,12.2596276657995,0.102349228387359));
#32317=CARTESIAN_POINT('Ctrl Pts',(21.8691652203497,10.6436381400426,-1.13178426217439));
#32318=CARTESIAN_POINT('Ctrl Pts',(21.6699530853725,7.04932465914044,-3.15879248522481));
#32319=CARTESIAN_POINT('Ctrl Pts',(21.530756201144,5.15107554627118,-3.9013718508336));
#32320=CARTESIAN_POINT('Ctrl Pts',(21.3170135369151,1.10319626289944,-4.9378748808481));
#32321=CARTESIAN_POINT('Ctrl Pts',(21.2454435758322,-0.980646982038895,
-5.21146208408366));
#32322=CARTESIAN_POINT('Ctrl Pts',(21.2184671711261,-3.07550338138541,-5.31907428975103));
#32323=CARTESIAN_POINT('',(20.6511762848484,17.7903503023534,7.2142159717446));
#32324=CARTESIAN_POINT('Ctrl Pts',(21.218467344218,-3.07550344707786,-5.31907359926584));
#32325=CARTESIAN_POINT('Ctrl Pts',(21.2856263228658,-0.997639372661455,
-5.0511681130263));
#32326=CARTESIAN_POINT('Ctrl Pts',(21.3911504312805,1.045201756315,-4.62383042535759));
#32327=CARTESIAN_POINT('Ctrl Pts',(21.6353270404075,5.05250922301931,-3.29993368314891));
#32328=CARTESIAN_POINT('Ctrl Pts',(21.769809504508,6.93818763618363,-2.42047740785612));
#32329=CARTESIAN_POINT('Ctrl Pts',(21.902142242019,10.5055771888038,-0.191947765907667));
#32330=CARTESIAN_POINT('Ctrl Pts',(21.8949111024431,12.116505550095,1.10419073571645));
#32331=CARTESIAN_POINT('Ctrl Pts',(21.5552690502941,15.143532030257,4.00920664773668));
#32332=CARTESIAN_POINT('Ctrl Pts',(21.2169197327024,16.5255606713859,5.59473714402792));
#32333=CARTESIAN_POINT('Ctrl Pts',(20.6511762848484,17.7903503023534,7.2142159717446));
#32334=CARTESIAN_POINT('',(8.16028563385461,17.7903503023534,20.2959516012968));
#32335=CARTESIAN_POINT('Origin',(7.5111559719605E-6,17.7903503023534,4.07573877568452E-6));
#32336=CARTESIAN_POINT('',(17.3881234313567,-3.07550340054456,13.2728730239015));
#32337=CARTESIAN_POINT('Ctrl Pts',(8.16028563385462,17.7903503023534,20.2959516012968));
#32338=CARTESIAN_POINT('Ctrl Pts',(9.78652523329912,16.6048563822885,19.6420985397976));
#32339=CARTESIAN_POINT('Ctrl Pts',(11.2155224484438,15.2608755267349,18.8380234824792));
#32340=CARTESIAN_POINT('Ctrl Pts',(13.587278789106,12.2596276657994,17.2020522353224));
#32341=CARTESIAN_POINT('Ctrl Pts',(14.5200720721495,10.6436381400426,16.3923415812932));
#32342=CARTESIAN_POINT('Ctrl Pts',(15.980644181587,7.0493246591405,14.9727723071226));
#32343=CARTESIAN_POINT('Ctrl Pts',(16.4744282700841,5.15107554627125,14.4009531392434));
#32344=CARTESIAN_POINT('Ctrl Pts',(17.1515325992541,1.1031962628995,13.587593326393));
#32345=CARTESIAN_POINT('Ctrl Pts',(17.3208085470894,-0.980646982038474,
13.3610588464829));
#32346=CARTESIAN_POINT('Ctrl Pts',(17.3881236441529,-3.07550338138541,13.2728727312108));
#32347=CARTESIAN_POINT('',(7.23550265652423,17.7903503023534,20.6437255183797));
#32348=CARTESIAN_POINT('Ctrl Pts',(17.3881232122309,-3.07550344707786,13.27287329705));
#32349=CARTESIAN_POINT('Ctrl Pts',(17.2205392070531,-0.99763937266114,13.4924166394196));
#32350=CARTESIAN_POINT('Ctrl Pts',(16.9522263546354,1.04520175631507,13.8413593997489));
#32351=CARTESIAN_POINT('Ctrl Pts',(16.069403827683,5.05250922301932,14.8577004775278));
#32352=CARTESIAN_POINT('Ctrl Pts',(15.4656656691005,6.93818763618363,15.5111751206272));
#32353=CARTESIAN_POINT('Ctrl Pts',(13.8058391477021,10.5055771888038,17.0041025258692));
#32354=CARTESIAN_POINT('Ctrl Pts',(12.7879687197121,12.116505550095,17.8065781308538));
#32355=CARTESIAN_POINT('Ctrl Pts',(10.3049724668269,15.143532030257,19.3522830770956));
#32356=CARTESIAN_POINT('Ctrl Pts',(8.85439745942891,16.5255606713859,20.0763130235044));
#32357=CARTESIAN_POINT('Ctrl Pts',(7.23550265652423,17.7903503023534,20.6437255183797));
#32358=CARTESIAN_POINT('',(7.51115596928158E-6,17.7903503023534,21.8750040757388));
#32359=CARTESIAN_POINT('Origin',(7.5111559719605E-6,17.7903503023534,4.07573877568452E-6));
#32360=CARTESIAN_POINT('',(7.51080208344241E-6,1.03580637516255,21.8750040757388));
#32361=CARTESIAN_POINT('',(7.51115596928158E-6,20.2903503023534,21.8750040757388));
#32362=CARTESIAN_POINT('',(0.464173657934616,-3.07550341763295,21.8700789498582));
#32363=CARTESIAN_POINT('Ctrl Pts',(7.51044819783525E-6,1.03580637516255,
21.8750040757388));
#32364=CARTESIAN_POINT('Ctrl Pts',(0.243703115036094,-0.321768697993278,
21.8750040757467));
#32365=CARTESIAN_POINT('Ctrl Pts',(0.391146320999169,-1.69625048081135,
21.8716288639911));
#32366=CARTESIAN_POINT('Ctrl Pts',(0.464174017015567,-3.0755033986066,21.8700789374039));
#32367=CARTESIAN_POINT('Ctrl Pts',(0.464173305560506,-3.07550345570599,
21.8700789525037));
#32368=CARTESIAN_POINT('Ctrl Pts',(0.342862298231604,-2.16265365777846,
21.8726536313927));
#32369=CARTESIAN_POINT('Ctrl Pts',(0.189893689499557,-1.25657667567048,
21.8750040757392));
#32370=CARTESIAN_POINT('Ctrl Pts',(7.51110489346195E-6,-0.359077263140675,
21.8750040757388));
#32371=CARTESIAN_POINT('Origin',(7.5111559719605E-6,13.1028503023534,4.07573877568452E-6));
#32372=CARTESIAN_POINT('',(7.51115597150125E-6,13.1028503023534,3.75000407573878));
#32373=CARTESIAN_POINT('Origin',(7.5111559719605E-6,13.1028503023534,4.07573877568452E-6));
#32374=CARTESIAN_POINT('',(7.51115597119509E-6,15.6028503023534,6.25000407573878));
#32375=CARTESIAN_POINT('Origin',(7.51115597119509E-6,13.1028503023534,6.25000407573878));
#32376=CARTESIAN_POINT('Origin',(7.5111559719605E-6,15.6028503023534,4.07573877568452E-6));
#32377=CARTESIAN_POINT('Origin',(7.5111559719605E-6,13.1028503023534,4.07573877568452E-6));
#32378=CARTESIAN_POINT('',(7.51115597173087E-6,13.1028503023534,-1.87499592426122));
#32379=CARTESIAN_POINT('Origin',(7.5111559719605E-6,13.1028503023534,4.07573877568452E-6));
#32380=CARTESIAN_POINT('',(7.51115597173087E-6,15.6028503023534,-1.87499592426122));
#32381=CARTESIAN_POINT('',(7.51115597173087E-6,13.1028503023534,-1.87499592426122));
#32382=CARTESIAN_POINT('Origin',(7.5111559719605E-6,15.6028503023534,4.07573877568452E-6));
#32383=CARTESIAN_POINT('Origin',(7.5111559719605E-6,14.3528503023534,4.07573877568452E-6));
#32384=CARTESIAN_POINT('',(7.51115596966429E-6,15.6028503023534,18.7500040757388));
#32385=CARTESIAN_POINT('Origin',(7.5111559719605E-6,15.6028503023534,4.07573877568452E-6));
#32386=CARTESIAN_POINT('',(7.5111559695112E-6,14.3528503023534,20.0000040757388));
#32387=CARTESIAN_POINT('Origin',(7.51115596966428E-6,14.3528503023534,18.7500040757388));
#32388=CARTESIAN_POINT('Origin',(7.5111559719605E-6,14.3528503023534,4.07573877568452E-6));
#32389=CARTESIAN_POINT('Origin',(7.5111559719605E-6,15.6028503023534,4.07573877568452E-6));
#32390=CARTESIAN_POINT('',(7.5111559695112E-6,-3.14714969764662,20.0000040757388));
#32391=CARTESIAN_POINT('',(7.5111559695112E-6,15.6028503023534,20.0000040757388));
#32392=CARTESIAN_POINT('Origin',(7.5111559719605E-6,-3.14714969764662,4.07573877568452E-6));
#32393=CARTESIAN_POINT('Origin',(7.5111559719605E-6,21.2397676607012,4.07573877568452E-6));
#32394=CARTESIAN_POINT('',(29.890987486445,20.7105311502984,-36.1080966928894));
#32395=CARTESIAN_POINT('',(-0.621426586513352,-3.27137103605589,-46.8708765192191));
#32396=CARTESIAN_POINT('Ctrl Pts',(-0.621426973050868,-3.27137033355074,
-46.8708764811895));
#32397=CARTESIAN_POINT('Ctrl Pts',(1.22198947607096,-0.293500394512695,
-46.8953172968223));
#32398=CARTESIAN_POINT('Ctrl Pts',(3.47149086853713,2.39667808539656,-46.812476661266));
#32399=CARTESIAN_POINT('Ctrl Pts',(8.47386002556298,7.40863725852386,-46.1734052030165));
#32400=CARTESIAN_POINT('Ctrl Pts',(11.2378060047234,9.72308571822484,-45.603191808413));
#32401=CARTESIAN_POINT('Ctrl Pts',(16.8130139628313,13.8834472854297,-43.8519117248611));
#32402=CARTESIAN_POINT('Ctrl Pts',(19.6837688691993,15.782750805847,-42.6607369480052));
#32403=CARTESIAN_POINT('Ctrl Pts',(24.9813517355624,18.7788815506097,-39.7661777334129));
#32404=CARTESIAN_POINT('Ctrl Pts',(27.4992571672096,19.9779504583433,-38.0880170308874));
#32405=CARTESIAN_POINT('Ctrl Pts',(29.8909874864411,20.7105311502992,-36.1080966928852));
#32406=CARTESIAN_POINT('',(29.906901044747,20.5529756002067,-36.0949172314265));
#32407=CARTESIAN_POINT('',(29.906901044747,20.5529756002067,-36.0949172314265));
#32408=CARTESIAN_POINT('Ctrl Pts',(29.9069010447472,20.5529756002057,-36.0949172314263));
#32409=CARTESIAN_POINT('Ctrl Pts',(27.4917467114803,19.3280006163688,-38.0960232290689));
#32410=CARTESIAN_POINT('Ctrl Pts',(24.9374114080822,17.7790790293585,-39.7993592079281));
#32411=CARTESIAN_POINT('Ctrl Pts',(19.584902818122,14.2745254800632,-42.7044404021991));
#32412=CARTESIAN_POINT('Ctrl Pts',(16.7183127703354,12.2572382417917,-43.8921366201915));
#32413=CARTESIAN_POINT('Ctrl Pts',(8.45552582412058,6.00731091640547,-46.4561374167343));
#32414=CARTESIAN_POINT('Ctrl Pts',(3.38588451053795,1.62140339199547,-46.9240070793036));
#32415=CARTESIAN_POINT('Ctrl Pts',(-0.621426068179982,-3.27137132078905,
-46.8708764931867));
#32416=CARTESIAN_POINT('Origin',(7.5111559719605E-6,17.7903503023534,4.07573877568452E-6));
#32417=CARTESIAN_POINT('',(7.51115596958774E-6,20.2903503023534,-19.3749959242612));
#32418=CARTESIAN_POINT('Origin',(7.5111559719605E-6,20.2903503023534,4.07573877568452E-6));
#32419=CARTESIAN_POINT('Origin',(7.51115596958774E-6,17.7903503023534,-19.3749959242612));
#32420=CARTESIAN_POINT('',(-12.693647630517,19.9464420456703,-16.2756753502908));
#32421=CARTESIAN_POINT('Ctrl Pts',(-12.6936476305231,19.9464420456617,-16.2756753502661));
#32422=CARTESIAN_POINT('Ctrl Pts',(-12.8235252273233,19.8728182056928,-16.3334681308482));
#32423=CARTESIAN_POINT('Ctrl Pts',(-12.9581519320085,19.7918094976896,-16.371317941139));
#32424=CARTESIAN_POINT('Ctrl Pts',(-13.2224716578103,19.625306229008,-16.4147366199682));
#32425=CARTESIAN_POINT('Ctrl Pts',(-13.3532075689092,19.5393897285476,-16.4214641365178));
#32426=CARTESIAN_POINT('Ctrl Pts',(-13.7362414247294,19.2783123963091,-16.407438160254));
#32427=CARTESIAN_POINT('Ctrl Pts',(-13.987254982389,19.0945659360765,-16.3530231613382));
#32428=CARTESIAN_POINT('Ctrl Pts',(-14.6625794013184,18.5673472018936,-16.1138738953652));
#32429=CARTESIAN_POINT('Ctrl Pts',(-15.0965980929232,18.1860724615002,-15.8396990959256));
#32430=CARTESIAN_POINT('Ctrl Pts',(-15.4759234075142,17.7903503023534,-15.4599825736911));
#32431=CARTESIAN_POINT('',(-12.5441843191278,20.1925493450899,-15.6634703684439));
#32432=CARTESIAN_POINT('Ctrl Pts',(-12.5441843191278,20.1925493450898,-15.6634703684439));
#32433=CARTESIAN_POINT('Ctrl Pts',(-12.5734306475263,20.1623540838438,-15.774258024762));
#32434=CARTESIAN_POINT('Ctrl Pts',(-12.6011389695311,20.1252944701824,-15.8835795820431));
#32435=CARTESIAN_POINT('Ctrl Pts',(-12.6271510859688,20.0815864671199,-15.9906280584417));
#32436=CARTESIAN_POINT('Ctrl Pts',(-12.6507434848167,20.0419443009946,-16.0877185953578));
#32437=CARTESIAN_POINT('Ctrl Pts',(-12.6729413900718,19.9968331833498,-16.1829393382146));
#32438=CARTESIAN_POINT('Ctrl Pts',(-12.6936476305122,19.946442045657,-16.2756753502846));
#32439=CARTESIAN_POINT('Ctrl Pts',(-16.1582306321435,17.7903503023534,-14.7454008052546));
#32440=CARTESIAN_POINT('Ctrl Pts',(-15.9327118880776,18.0166323356832,-14.9925276628623));
#32441=CARTESIAN_POINT('Ctrl Pts',(-15.6779879864518,18.244370505181,-15.2146917900135));
#32442=CARTESIAN_POINT('Ctrl Pts',(-15.1369202951668,18.6805240933459,-15.5819230082715));
#32443=CARTESIAN_POINT('Ctrl Pts',(-14.8487394640944,18.8925325606821,-15.7331109967917));
#32444=CARTESIAN_POINT('Ctrl Pts',(-14.163605905897,19.353358815909,-15.9788255101609));
#32445=CARTESIAN_POINT('Ctrl Pts',(-13.7876875418779,19.5776706634899,-16.0374669418776));
#32446=CARTESIAN_POINT('Ctrl Pts',(-13.260925054244,19.8635098001506,-16.0019414049453));
#32447=CARTESIAN_POINT('Ctrl Pts',(-13.066900930548,19.9622625901948,-15.9623273700109));
#32448=CARTESIAN_POINT('Ctrl Pts',(-12.7633032903853,20.1031710857547,-15.8284713051116));
#32449=CARTESIAN_POINT('Ctrl Pts',(-12.6477215025671,20.1529191619863,-15.7566974006731));
#32450=CARTESIAN_POINT('Ctrl Pts',(-12.5441843191278,20.1925493450899,-15.6634703684439));
#32451=CARTESIAN_POINT('',(-20.6391955918159,19.9464420456703,-0.223416847360512));
#32452=CARTESIAN_POINT('Ctrl Pts',(-20.6391955918004,19.9464420456617,-0.223416847340363));
#32453=CARTESIAN_POINT('Ctrl Pts',(-20.7653571642138,19.8728182056928,-0.157907662608692));
#32454=CARTESIAN_POINT('Ctrl Pts',(-20.8788877149336,19.7918094976896,-0.0762512372233672));
#32455=CARTESIAN_POINT('Ctrl Pts',(-21.0776344584369,19.625306229008,0.103331142385521));
#32456=CARTESIAN_POINT('Ctrl Pts',(-21.1644067499811,19.5393897285476,0.201350055611236));
#32457=CARTESIAN_POINT('Ctrl Pts',(-21.3922585030362,19.2783123963091,0.509563036104214));
#32458=CARTESIAN_POINT('Ctrl Pts',(-21.5062195370944,19.0945659360766,0.739740534900876));
#32459=CARTESIAN_POINT('Ctrl Pts',(-21.7403030000965,18.5673472018931,1.41683755495611));
#32460=CARTESIAN_POINT('Ctrl Pts',(-21.7965507382266,18.1860724614997,1.92711222340975));
#32461=CARTESIAN_POINT('Ctrl Pts',(-21.7361818719648,17.7903503023534,2.46043007566384));
#32462=CARTESIAN_POINT('',(-20.067365612881,20.1925493450899,0.0414315931501207));
#32463=CARTESIAN_POINT('Ctrl Pts',(-20.067365612881,20.1925493450898,0.0414315931501189));
#32464=CARTESIAN_POINT('Ctrl Pts',(-20.1722176779583,20.1623540838436,-0.00477768044781249));
#32465=CARTESIAN_POINT('Ctrl Pts',(-20.2749645693503,20.1252944701819,-0.0512753180664436));
#32466=CARTESIAN_POINT('Ctrl Pts',(-20.3748767276733,20.0815864671191,-0.0976818598491867));
#32467=CARTESIAN_POINT('Ctrl Pts',(-20.4654947861664,20.0419443009939,-0.139771539306826));
#32468=CARTESIAN_POINT('Ctrl Pts',(-20.5537815282644,19.9968331833494,-0.181785680229823));
#32469=CARTESIAN_POINT('Ctrl Pts',(-20.6391955918081,19.946442045657,-0.223416847360427));
#32470=CARTESIAN_POINT('Ctrl Pts',(-21.6029109448944,17.7903503023534,3.43941378980876));
#32471=CARTESIAN_POINT('Ctrl Pts',(-21.6555138652825,18.0166323356831,3.10901506032762));
#32472=CARTESIAN_POINT('Ctrl Pts',(-21.6703910192109,18.244370505181,2.7713468270818));
#32473=CARTESIAN_POINT('Ctrl Pts',(-21.6201537593587,18.6805240933459,2.11935815238101));
#32474=CARTESIAN_POINT('Ctrl Pts',(-21.55867947929,18.8925325606821,1.79978513699883));
#32475=CARTESIAN_POINT('Ctrl Pts',(-21.3236130350936,19.3533588159098,1.11092565824911));
#32476=CARTESIAN_POINT('Ctrl Pts',(-21.1350794862891,19.5776706634905,0.780458511779776));
#32477=CARTESIAN_POINT('Ctrl Pts',(-20.7788734640431,19.8635098001506,0.390768825148143));
#32478=CARTESIAN_POINT('Ctrl Pts',(-20.6269299019448,19.9622625901948,0.263773603676359));
#32479=CARTESIAN_POINT('Ctrl Pts',(-20.3329869837774,20.1031710857547,0.109869301975848));
#32480=CARTESIAN_POINT('Ctrl Pts',(-20.2048078196825,20.1529191619863,0.0642541189165845));
#32481=CARTESIAN_POINT('Ctrl Pts',(-20.067365612881,20.1925493450898,0.0414315931501027));
#32482=CARTESIAN_POINT('',(-13.0430026535592,19.9464420456703,15.9970821676198));
#32483=CARTESIAN_POINT('Ctrl Pts',(-13.0430026535338,19.9464420456617,15.9970821676202));
#32484=CARTESIAN_POINT('Ctrl Pts',(-13.0704465353675,19.872816673671,16.1365664678557));
#32485=CARTESIAN_POINT('Ctrl Pts',(-13.0773897151475,19.7918112588121,16.2762344448439));
#32486=CARTESIAN_POINT('Ctrl Pts',(-13.0609029504193,19.625306229008,16.5435915160662));
#32487=CARTESIAN_POINT('Ctrl Pts',(-13.0383703170438,19.5393897285476,16.6725466181869));
#32488=CARTESIAN_POINT('Ctrl Pts',(-12.9394629499546,19.2783123963091,17.0428559421987));
#32489=CARTESIAN_POINT('Ctrl Pts',(-12.8305564773841,19.0945659360765,17.2754675895172));
#32490=CARTESIAN_POINT('Ctrl Pts',(-12.4471293623855,18.5673472018934,17.8806444972902));
#32491=CARTESIAN_POINT('Ctrl Pts',(-12.0832504529845,18.1860724615001,18.2427718017058));
#32492=CARTESIAN_POINT('Ctrl Pts',(-11.6286463934656,17.7903503023534,18.5280917635313));
#32493=CARTESIAN_POINT('',(-12.4794056444224,20.1925493450899,15.715137789166));
#32494=CARTESIAN_POINT('Ctrl Pts',(-12.4794056444224,20.1925493450898,15.715137789166));
#32495=CARTESIAN_POINT('Ctrl Pts',(-12.5809077025813,20.162354083844,15.7683034238049));
#32496=CARTESIAN_POINT('Ctrl Pts',(-12.6813226584862,20.125294470183,15.8196433753545));
#32497=CARTESIAN_POINT('Ctrl Pts',(-12.7798989656392,20.081586467121,15.868823840671));
#32498=CARTESIAN_POINT('Ctrl Pts',(-12.8693054374623,20.0419443009953,15.9134294057765));
#32499=CARTESIAN_POINT('Ctrl Pts',(-12.9571992988835,19.9968331833502,15.9562593718345));
#32500=CARTESIAN_POINT('Ctrl Pts',(-13.0430026535542,19.946442045657,15.9970821676137));
#32501=CARTESIAN_POINT('',(-10.7801530410109,17.7903503023534,19.0342827190051));
#32502=CARTESIAN_POINT('Ctrl Pts',(-10.7801530410109,17.7903503023534,19.0342827190051));
#32503=CARTESIAN_POINT('Ctrl Pts',(-11.0712665538967,18.0166323356832,18.8694090998557));
#32504=CARTESIAN_POINT('Ctrl Pts',(-11.3445419630327,18.244370505181,18.6705078273261));
#32505=CARTESIAN_POINT('Ctrl Pts',(-11.8229648159352,18.6805240933458,18.2247224663774));
#32506=CARTESIAN_POINT('Ctrl Pts',(-12.0344884736088,18.8925325606821,17.9774094228175));
#32507=CARTESIAN_POINT('Ctrl Pts',(-12.4264989703763,19.3533588159099,17.3641302163587));
#32508=CARTESIAN_POINT('Ctrl Pts',(-12.5673198444194,19.5776706634906,17.0106858567289));
#32509=CARTESIAN_POINT('Ctrl Pts',(-12.6499006875901,19.8635098001506,16.4892252287881));
#32510=CARTESIAN_POINT('Ctrl Pts',(-12.6544542884334,19.9622625901948,16.2912507429088));
#32511=CARTESIAN_POINT('Ctrl Pts',(-12.5915111049841,20.1031710857547,15.9654791528645));
#32512=CARTESIAN_POINT('Ctrl Pts',(-12.5472560895544,20.1529191619863,15.8368240455314));
#32513=CARTESIAN_POINT('Ctrl Pts',(-12.4794056444224,20.1925493450899,15.715137789166));
#32514=CARTESIAN_POINT('Origin',(7.5111559719605E-6,17.7903503023534,4.07573877568452E-6));
#32515=CARTESIAN_POINT('',(4.37484296764849,19.9464420456703,20.1714550984892));
#32516=CARTESIAN_POINT('Ctrl Pts',(4.37484296766468,19.9464420456617,20.1714550984696));
#32517=CARTESIAN_POINT('Ctrl Pts',(4.46678329128665,19.8728182056928,20.2798763718909));
#32518=CARTESIAN_POINT('Ctrl Pts',(4.57165534378247,19.7918094976897,20.3723902106327));
#32519=CARTESIAN_POINT('Ctrl Pts',(4.79096052918446,19.625306229008,20.5261931194967));
#32520=CARTESIAN_POINT('Ctrl Pts',(4.90583055496595,19.5393897285475,20.5889785884108));
#32521=CARTESIAN_POINT('Ctrl Pts',(5.2570177774387,19.2783123963091,20.742533782027));
#32522=CARTESIAN_POINT('Ctrl Pts',(5.50678296150517,19.0945659360764,20.8024182630235));
#32523=CARTESIAN_POINT('Ctrl Pts',(6.21899221642201,18.5673472018938,20.8799645036025));
#32524=CARTESIAN_POINT('Ctrl Pts',(6.72898953279836,18.1860724615004,20.8212551977046));
#32525=CARTESIAN_POINT('Ctrl Pts',(7.23550265652423,17.7903503023534,20.6437255183797));
#32526=CARTESIAN_POINT('',(4.50580696382332,20.1925493450899,19.5550277686639));
#32527=CARTESIAN_POINT('Ctrl Pts',(4.50580696382332,20.1925493450898,19.5550277686639));
#32528=CARTESIAN_POINT('Ctrl Pts',(4.48408803263945,20.1623540838438,19.6675335042753));
#32529=CARTESIAN_POINT('Ctrl Pts',(4.46161952210836,20.1252944701825,19.7780510143322));
#32530=CARTESIAN_POINT('Ctrl Pts',(4.43860903600032,20.0815864671201,19.885784593266));
#32531=CARTESIAN_POINT('Ctrl Pts',(4.41773904769133,20.0419443009947,19.9834965026223));
#32532=CARTESIAN_POINT('Ctrl Pts',(4.3964239373066,19.9968331833498,20.0789187376476));
#32533=CARTESIAN_POINT('Ctrl Pts',(4.37484296764684,19.946442045657,20.1714550984815));
#32534=CARTESIAN_POINT('Ctrl Pts',(8.16028563385462,17.7903503023534,20.2959516012968));
#32535=CARTESIAN_POINT('Ctrl Pts',(7.84987594130768,18.0166323356831,20.4207562905075));
#32536=CARTESIAN_POINT('Ctrl Pts',(7.52398423384595,18.244370505181,20.5103986937555));
#32537=CARTESIAN_POINT('Ctrl Pts',(6.87716343447198,18.6805240933459,20.6065021157174));
#32538=CARTESIAN_POINT('Ctrl Pts',(6.55192346758059,18.8925325606821,20.6176808100472));
#32539=CARTESIAN_POINT('Ctrl Pts',(5.82802792947244,19.3533588159096,20.5417936269589));
#32540=CARTESIAN_POINT('Ctrl Pts',(5.46389362295823,19.5776706634904,20.431522865921));
#32541=CARTESIAN_POINT('Ctrl Pts',(5.00471097362036,19.8635098001506,20.1709617853684));
#32542=CARTESIAN_POINT('Ctrl Pts',(4.84708916414706,19.9622625901948,20.0510868608924));
#32543=CARTESIAN_POINT('Ctrl Pts',(4.63163511193388,20.1031710857547,19.798760634337));
#32544=CARTESIAN_POINT('Ctrl Pts',(4.55864104944201,20.1529191619863,19.6839455226377));
#32545=CARTESIAN_POINT('Ctrl Pts',(4.50580696382331,20.1925493450898,19.5550277686639));
#32546=CARTESIAN_POINT('',(18.4983482597372,19.9464420456703,9.15631398661356));
#32547=CARTESIAN_POINT('Ctrl Pts',(18.4983482597319,19.9464420456617,9.15631398658867));
#32548=CARTESIAN_POINT('Ctrl Pts',(18.6404422355597,19.872816673671,9.15203161624641));
#32549=CARTESIAN_POINT('Ctrl Pts',(18.7781534476127,19.791811258812,9.12772166732995));
#32550=CARTESIAN_POINT('Ctrl Pts',(19.0351386685812,19.625306229008,9.05215571502665));
#32551=CARTESIAN_POINT('Ctrl Pts',(19.1558466144338,19.5393897285476,9.00149281205167));
#32552=CARTESIAN_POINT('Ctrl Pts',(19.4948625508543,19.2783123963091,8.82266368252409));
#32553=CARTESIAN_POINT('Ctrl Pts',(19.6974081685334,19.0945659360765,8.66472676158745));
#32554=CARTESIAN_POINT('Ctrl Pts',(20.2020914679953,18.5673472018936,8.1562484341617));
#32555=CARTESIAN_POINT('Ctrl Pts',(20.4741688100664,18.1860724615003,7.7209118227428));
#32556=CARTESIAN_POINT('Ctrl Pts',(20.6511762848484,17.7903503023534,7.2142159717446));
#32557=CARTESIAN_POINT('',(18.0980606826517,20.1925493450899,8.66958605760119));
#32558=CARTESIAN_POINT('Ctrl Pts',(18.0980606826517,20.1925493450898,8.66958605760119));
#32559=CARTESIAN_POINT('Ctrl Pts',(18.1724796766112,20.1623540838435,8.75671278057142));
#32560=CARTESIAN_POINT('Ctrl Pts',(18.2448768581592,20.1252944701818,8.84318590991689));
#32561=CARTESIAN_POINT('Ctrl Pts',(18.3147595584651,20.0815864671188,8.92834702016679));
#32562=CARTESIAN_POINT('Ctrl Pts',(18.3781415805357,20.0419443009937,9.00558621306851));
#32563=CARTESIAN_POINT('Ctrl Pts',(18.4394559340548,19.9968331833493,9.0817458278276));
#32564=CARTESIAN_POINT('Ctrl Pts',(18.4983482597302,19.946442045657,9.15631398661009));
#32565=CARTESIAN_POINT('Ctrl Pts',(20.9558684429898,17.7903503023534,6.27435803496357));
#32566=CARTESIAN_POINT('Ctrl Pts',(20.8599066157679,18.0166341860667,6.59486317686292));
#32567=CARTESIAN_POINT('Ctrl Pts',(20.7268038872205,18.2443686579063,6.90554168138285));
#32568=CARTESIAN_POINT('Ctrl Pts',(20.3986530062068,18.6805240933459,7.47116844499778));
#32569=CARTESIAN_POINT('Ctrl Pts',(20.2046090588531,18.8925325606821,7.73242109238302));
#32570=CARTESIAN_POINT('Ctrl Pts',(19.6939365843773,19.3533588159097,8.25107052934689));
#32571=CARTESIAN_POINT('Ctrl Pts',(19.3806894051836,19.5776706634905,8.46700949907594));
#32572=CARTESIAN_POINT('Ctrl Pts',(18.8906788502492,19.8635098001506,8.66355577404548));
#32573=CARTESIAN_POINT('Ctrl Pts',(18.6986812695782,19.9622625901948,8.71204867410587));
#32574=CARTESIAN_POINT('Ctrl Pts',(18.3670712774808,20.1031710857547,8.72317460615268));
#32575=CARTESIAN_POINT('Ctrl Pts',(18.2317941549313,20.1529191619863,8.70865761099829));
#32576=CARTESIAN_POINT('Ctrl Pts',(18.0980606826517,20.1925493450899,8.6695860576012));
#32577=CARTESIAN_POINT('',(18.6922256707601,19.9464420456703,-8.75371524283479));
#32578=CARTESIAN_POINT('Ctrl Pts',(18.6922256707374,19.9464420456617,-8.75371524284621));
#32579=CARTESIAN_POINT('Ctrl Pts',(18.7774717236184,19.872816673671,-8.86747880085354));
#32580=CARTESIAN_POINT('Ctrl Pts',(18.844326976535,19.7918112588121,-8.99030276715853));
#32581=CARTESIAN_POINT('Ctrl Pts',(18.9454748005239,19.625306229008,-9.23833650406963));
#32582=CARTESIAN_POINT('Ctrl Pts',(18.9811251212272,19.5393897285476,-9.36429757965868));
#32583=CARTESIAN_POINT('Ctrl Pts',(19.0526838568059,19.2783123963091,-9.74084905034631));
#32584=CARTESIAN_POINT('Ctrl Pts',(19.0554889268077,19.0945659360765,-9.99767765042472));
#32585=CARTESIAN_POINT('Ctrl Pts',(18.9726094526565,18.5673472018935,-10.7092859942362));
#32586=CARTESIAN_POINT('Ctrl Pts',(18.8018870324763,18.1860724615002,-11.193432563529));
#32587=CARTESIAN_POINT('Ctrl Pts',(18.5160986195094,17.7903503023534,-11.6477422756871));
#32588=CARTESIAN_POINT('',(18.0621112303383,20.1925493450899,-8.74422771304759));
#32589=CARTESIAN_POINT('Ctrl Pts',(18.0621112303383,20.1925493450898,-8.74422771304759));
#32590=CARTESIAN_POINT('Ctrl Pts',(18.1766291291173,20.162354083844,-8.74808820217735));
#32591=CARTESIAN_POINT('Ctrl Pts',(18.2893754484039,20.1252944701829,-8.75077548367181));
#32592=CARTESIAN_POINT('Ctrl Pts',(18.3995282364447,20.0815864671208,-8.75231489509503));
#32593=CARTESIAN_POINT('Ctrl Pts',(18.4994343135196,20.0419443009952,-8.75371110629433));
#32594=CARTESIAN_POINT('Ctrl Pts',(18.5972071721593,19.9968331833502,-8.75416385508704));
#32595=CARTESIAN_POINT('Ctrl Pts',(18.692225670753,19.946442045657,-8.75371524283147));
#32596=CARTESIAN_POINT('Ctrl Pts',(17.9712605487941,17.7903503023534,-12.4719520361622));
#32597=CARTESIAN_POINT('Ctrl Pts',(18.1620087785714,18.0166323356831,-12.1970966186916));
#32598=CARTESIAN_POINT('Ctrl Pts',(18.3219213867259,18.244370505181,-11.8993230080315));
#32599=CARTESIAN_POINT('Ctrl Pts',(18.5595464636318,18.6805240933458,-11.2901043797534));
#32600=CARTESIAN_POINT('Ctrl Pts',(18.6428175859483,18.8925325606821,-10.9755063513766));
#32601=CARTESIAN_POINT('Ctrl Pts',(18.7299149642054,19.35335881591,-10.2528738989142));
#32602=CARTESIAN_POINT('Ctrl Pts',(18.7034364273428,19.5776706634907,-9.87333164697644));
#32603=CARTESIAN_POINT('Ctrl Pts',(18.5515859090712,19.8635098001506,-9.36768137035073));
#32604=CARTESIAN_POINT('Ctrl Pts',(18.4697906514847,19.9622625901948,-9.18733678857422));
#32605=CARTESIAN_POINT('Ctrl Pts',(18.2717338071635,20.1031710857547,-8.92113675168414));
#32606=CARTESIAN_POINT('Ctrl Pts',(18.1760400569865,20.1529191619863,-8.82442403684966));
#32607=CARTESIAN_POINT('Ctrl Pts',(18.0621112303383,20.1925493450898,-8.74422771304758));
#32608=CARTESIAN_POINT('',(4.81048155583834,19.9464420456703,-20.0720152820648));
#32609=CARTESIAN_POINT('Ctrl Pts',(4.81048155581525,19.9464420456617,-20.0720152820541));
#32610=CARTESIAN_POINT('Ctrl Pts',(4.77468841403889,19.8728182056928,-20.2095908854138));
#32611=CARTESIAN_POINT('Ctrl Pts',(4.72034220990053,19.7918094976896,-20.3384452522362));
#32612=CARTESIAN_POINT('Ctrl Pts',(4.58948764646888,19.625306229008,-20.5721698387655));
#32613=CARTESIAN_POINT('Ctrl Pts',(4.51323492339935,19.5393897285476,-20.6785778279124));
#32614=CARTESIAN_POINT('Ctrl Pts',(4.26345127071336,19.2783123963091,-20.9693007020821));
#32615=CARTESIAN_POINT('Ctrl Pts',(4.06440351811344,19.0945659360765,-21.1316238070946));
#32616=CARTESIAN_POINT('Ctrl Pts',(3.4563712048186,18.567347201894,-21.5105065702365));
#32617=CARTESIAN_POINT('Ctrl Pts',(2.97140648688581,18.1860724615007,-21.6788908559357));
#32618=CARTESIAN_POINT('Ctrl Pts',(2.4380266901546,17.7903503023534,-21.7387099497696));
#32619=CARTESIAN_POINT('',(4.42502927770989,20.1925493450898,-19.5734565969181));
#32620=CARTESIAN_POINT('Ctrl Pts',(4.42502927770989,20.1925493450898,-19.5734565969181));
#32621=CARTESIAN_POINT('Ctrl Pts',(4.49341176778961,20.162354083844,-19.6653972710923));
#32622=CARTESIAN_POINT('Ctrl Pts',(4.5616069467874,20.1252944701828,-19.7552213856496));
#32623=CARTESIAN_POINT('Ctrl Pts',(4.62908252646208,20.0815864671207,-19.8423021105449));
#32624=CARTESIAN_POINT('Ctrl Pts',(4.69028134479012,20.0419443009951,-19.9212823503358));
#32625=CARTESIAN_POINT('Ctrl Pts',(4.75088775179068,19.9968331833501,-19.9980065336062));
#32626=CARTESIAN_POINT('Ctrl Pts',(4.81048155583652,19.946442045657,-20.0720152820572));
#32627=CARTESIAN_POINT('Ctrl Pts',(1.45393257050235,17.7903503023534,-21.8266247734858));
#32628=CARTESIAN_POINT('Ctrl Pts',(1.78775549475546,18.0166341860667,-21.8043880131364));
#32629=CARTESIAN_POINT('Ctrl Pts',(2.1202627839953,18.2443686579063,-21.743754918874));
#32630=CARTESIAN_POINT('Ctrl Pts',(2.74472854424224,18.6805240933458,-21.549695261277));
#32631=CARTESIAN_POINT('Ctrl Pts',(3.04260988270327,18.8925325606821,-21.4186505839066));
#32632=CARTESIAN_POINT('Ctrl Pts',(3.66189101140341,19.3533588159101,-21.036192091666));
#32633=CARTESIAN_POINT('Ctrl Pts',(3.94211999519319,19.5776706634907,-20.7788496144794));
#32634=CARTESIAN_POINT('Ctrl Pts',(4.24277605102848,19.8635098001506,-20.3448603078825));
#32635=CARTESIAN_POINT('Ctrl Pts',(4.33277661380831,19.9622625901948,-20.1684671928266));
#32636=CARTESIAN_POINT('Ctrl Pts',(4.41741376066054,20.1031710857547,-19.8476471083627));
#32637=CARTESIAN_POINT('Ctrl Pts',(4.43336272853615,20.1529191619863,-19.7125313303895));
#32638=CARTESIAN_POINT('Ctrl Pts',(4.4250292777099,20.1925493450898,-19.5734565969181));
#32639=CARTESIAN_POINT('Origin',(7.5111559719605E-6,20.2903503023534,4.07573877568452E-6));
#32640=CARTESIAN_POINT('Ctrl Pts',(-10.7801530410109,17.7903503023534,19.0342827190051));
#32641=CARTESIAN_POINT('Ctrl Pts',(-9.25446266768857,16.6044337968475,19.8983652243397));
#32642=CARTESIAN_POINT('Ctrl Pts',(-7.73431157051831,15.2599230184859,20.514394463872));
#32643=CARTESIAN_POINT('Ctrl Pts',(-4.97570813316128,12.2573869722707,21.3487202901183));
#32644=CARTESIAN_POINT('Ctrl Pts',(-3.76084392376818,10.6406932625641,21.5730668416575));
#32645=CARTESIAN_POINT('Ctrl Pts',(-1.74098153262667,7.04601500804021,21.8296182862512));
#32646=CARTESIAN_POINT('Ctrl Pts',(-0.986571430673042,5.14830176393068,
21.8591019108078));
#32647=CARTESIAN_POINT('Ctrl Pts',(-0.278505434869228,2.43854448983318,
21.8739805820085));
#32648=CARTESIAN_POINT('Ctrl Pts',(-0.126302322075248,1.73945090916345,
21.8750040757347));
#32649=CARTESIAN_POINT('Ctrl Pts',(7.5104481972281E-6,1.03580637516255,
21.8750040757388));
#32650=CARTESIAN_POINT('Ctrl Pts',(-19.3643013307678,20.9435908393615,50.1865120070872));
#32651=CARTESIAN_POINT('Ctrl Pts',(-19.2220541116569,20.9358615047579,50.1240929228611));
#32652=CARTESIAN_POINT('Ctrl Pts',(-19.079806892546,20.9281321701544,50.061673838635));
#32653=CARTESIAN_POINT('Ctrl Pts',(-18.9375596734351,20.9204028355509,49.9992547544089));
#32654=CARTESIAN_POINT('Ctrl Pts',(-4.71283776234417,20.1474693751975,43.7573463318004));
#32655=CARTESIAN_POINT('Ctrl Pts',(4.99651958832846,20.0812550388979,28.7471447887935));
#32656=CARTESIAN_POINT('Ctrl Pts',(5.0291830418987,19.8399463130827,13.2252152613227));
#32657=CARTESIAN_POINT('Ctrl Pts',(-19.3642064856396,20.9469886892296,50.1865190303546));
#32658=CARTESIAN_POINT('Ctrl Pts',(-19.2219541714401,20.9392720585054,50.1241062032879));
#32659=CARTESIAN_POINT('Ctrl Pts',(-19.0797018572407,20.9315554277811,50.0616933762211));
#32660=CARTESIAN_POINT('Ctrl Pts',(-18.9374495430412,20.9238387970569,49.9992805491544));
#32661=CARTESIAN_POINT('Ctrl Pts',(-4.71221812309168,20.1521757246323,43.7579978424802));
#32662=CARTESIAN_POINT('Ctrl Pts',(4.99686729900256,20.0873688943554,28.7474275948137));
#32663=CARTESIAN_POINT('Ctrl Pts',(5.02977040929867,19.8474084919615,13.2255751562655));
#32664=CARTESIAN_POINT('Ctrl Pts',(-19.3641116405114,20.9503865390978,50.1865260536221));
#32665=CARTESIAN_POINT('Ctrl Pts',(-19.2218542312234,20.9426826122528,50.1241194837147));
#32666=CARTESIAN_POINT('Ctrl Pts',(-19.0795968219353,20.9349786854078,50.0617129138073));
#32667=CARTESIAN_POINT('Ctrl Pts',(-18.9373394126472,20.9272747585629,49.9993063438999));
#32668=CARTESIAN_POINT('Ctrl Pts',(-4.71159848383918,20.1568820740671,43.75864935316));
#32669=CARTESIAN_POINT('Ctrl Pts',(4.99721500967666,20.093482749813,28.747710400834));
#32670=CARTESIAN_POINT('Ctrl Pts',(5.03035777669865,19.8548706708402,13.2259350512082));
#32671=CARTESIAN_POINT('Ctrl Pts',(-19.3640167953833,20.9537843889659,50.1865330768895));
#32672=CARTESIAN_POINT('Ctrl Pts',(-19.2217542910066,20.9460931660003,50.1241327641415));
#32673=CARTESIAN_POINT('Ctrl Pts',(-19.0794917866299,20.9384019430346,50.0617324513934));
#32674=CARTESIAN_POINT('Ctrl Pts',(-18.9372292822533,20.9307107200689,49.9993321386454));
#32675=CARTESIAN_POINT('Ctrl Pts',(-4.71097884458669,20.1615884235019,43.7593008638397));
#32676=CARTESIAN_POINT('Ctrl Pts',(4.99756272035076,20.0995966052706,28.7479932068543));
#32677=CARTESIAN_POINT('Ctrl Pts',(5.03094514409862,19.862332849719,13.226294946151));
#32678=CARTESIAN_POINT('Ctrl Pts',(-19.363728775738,20.9641027630587,50.1865544047009));
#32679=CARTESIAN_POINT('Ctrl Pts',(-19.2214507989208,20.9564501184246,50.1241730932958));
#32680=CARTESIAN_POINT('Ctrl Pts',(-19.0791728221036,20.9487974737906,50.0617917818908));
#32681=CARTESIAN_POINT('Ctrl Pts',(-18.9368948452864,20.9411448291565,49.9994104704857));
#32682=CARTESIAN_POINT('Ctrl Pts',(-4.70909716356548,20.1758803657488,43.7612793299817));
#32683=CARTESIAN_POINT('Ctrl Pts',(4.99861862598245,20.1181627721728,28.7488520141665));
#32684=CARTESIAN_POINT('Ctrl Pts',(5.03272882401328,19.8849935193208,13.2273878521937));
#32685=CARTESIAN_POINT('Ctrl Pts',(-19.3631527362822,20.9847395112521,50.1865970600935));
#32686=CARTESIAN_POINT('Ctrl Pts',(-19.2208438146391,20.9771640232786,50.1242537514512));
#32687=CARTESIAN_POINT('Ctrl Pts',(-19.078534892996,20.9695885353052,50.061910442809));
#32688=CARTESIAN_POINT('Ctrl Pts',(-18.9362259713529,20.9620130473318,49.9995671341667));
#32689=CARTESIAN_POINT('Ctrl Pts',(-4.70533380704113,20.2044642499886,43.7652362699409));
#32690=CARTESIAN_POINT('Ctrl Pts',(5.00073044157035,20.1552951062578,28.7505696258898));
#32691=CARTESIAN_POINT('Ctrl Pts',(5.03629618384262,19.9303148585245,13.2295736642792));
#32692=CARTESIAN_POINT('Ctrl Pts',(-19.362288665564,21.0156946339229,50.1866610281067));
#32693=CARTESIAN_POINT('Ctrl Pts',(-19.2199333305268,21.0082348808134,50.1243747286337));
#32694=CARTESIAN_POINT('Ctrl Pts',(-19.0775779954895,21.000775127704,50.0620884291608));
#32695=CARTESIAN_POINT('Ctrl Pts',(-18.9352226604523,20.9933153745945,49.9998021296879));
#32696=CARTESIAN_POINT('Ctrl Pts',(-4.69968915672916,20.2473400636495,43.7711721823959));
#32697=CARTESIAN_POINT('Ctrl Pts',(5.00389843664987,20.2109936225946,28.7531458689445));
#32698=CARTESIAN_POINT('Ctrl Pts',(5.0416472235866,19.9982968673298,13.2328523824074));
#32699=CARTESIAN_POINT('Ctrl Pts',(-19.3614245796962,21.0466497571015,50.1867249762735));
#32700=CARTESIAN_POINT('Ctrl Pts',(-19.2190228363148,21.0393057386868,50.1244956925854));
#32701=CARTESIAN_POINT('Ctrl Pts',(-19.0766210929333,21.0319617202721,50.0622664088974));
#32702=CARTESIAN_POINT('Ctrl Pts',(-18.9342193495519,21.0246177018574,50.0000371252093));
#32703=CARTESIAN_POINT('Ctrl Pts',(-4.69404501140909,20.2902158603888,43.7771087564017));
#32704=CARTESIAN_POINT('Ctrl Pts',(5.00706678981436,20.2666921589687,28.7557218794068));
#32705=CARTESIAN_POINT('Ctrl Pts',(5.0469982633306,20.0662788761352,13.2361311005356));
#32706=CARTESIAN_POINT('Ctrl Pts',(-19.3608485148276,21.0672865061488,50.1867675983585));
#32707=CARTESIAN_POINT('Ctrl Pts',(-19.2184158350912,21.0600196441101,50.1245763285357));
#32708=CARTESIAN_POINT('Ctrl Pts',(-19.0759831553547,21.0527527820714,50.0623850587129));
#32709=CARTESIAN_POINT('Ctrl Pts',(-18.9335504756182,21.0454859200326,50.0001937888901));
#32710=CARTESIAN_POINT('Ctrl Pts',(-4.69028250197186,20.3187997161584,43.7810668066102));
#32711=CARTESIAN_POINT('Ctrl Pts',(5.00917920656114,20.3038245267329,28.7574391004138));
#32712=CARTESIAN_POINT('Ctrl Pts',(5.05056562315993,20.1116002153389,13.2383169126211));
#32713=CARTESIAN_POINT('Ctrl Pts',(-19.3605604823138,21.0776048806767,50.1867889092869));
#32714=CARTESIAN_POINT('Ctrl Pts',(-19.2181123344263,21.0703765968246,50.1246166464348));
#32715=CARTESIAN_POINT('Ctrl Pts',(-19.0756641865389,21.0631483129724,50.0624443835827));
#32716=CARTESIAN_POINT('Ctrl Pts',(-18.9332160386514,21.0559200291202,50.0002721207305));
#32717=CARTESIAN_POINT('Ctrl Pts',(-4.68840124990593,20.3330916439037,43.7830458355166));
#32718=CARTESIAN_POINT('Ctrl Pts',(5.01023541710294,20.3223907107576,28.7582977093251));
#32719=CARTESIAN_POINT('Ctrl Pts',(5.05234930307459,20.1342608849406,13.2394098186638));
#32720=CARTESIAN_POINT('Ctrl Pts',(-19.3605327274403,21.0785991614118,50.1867909628125));
#32721=CARTESIAN_POINT('Ctrl Pts',(-19.2180830890386,21.0713745949617,50.124620531476));
#32722=CARTESIAN_POINT('Ctrl Pts',(-19.0756334506368,21.0641500285117,50.0624501001396));
#32723=CARTESIAN_POINT('Ctrl Pts',(-18.9331838122351,21.0569254620617,50.0002796688031));
#32724=CARTESIAN_POINT('Ctrl Pts',(-4.68821997206204,20.3344688170607,43.7832365351574));
#32725=CARTESIAN_POINT('Ctrl Pts',(5.01033719377241,20.3241797521467,28.75838044506));
#32726=CARTESIAN_POINT('Ctrl Pts',(5.05252117884551,20.1364444718193,13.2395151313195));
#32727=CARTESIAN_POINT('Ctrl Pts',(-19.3605049725668,21.0795934421468,50.186793016338));
#32728=CARTESIAN_POINT('Ctrl Pts',(-19.2180538436508,21.0723725930989,50.1246244165172));
#32729=CARTESIAN_POINT('Ctrl Pts',(-19.0756027147348,21.0651517440511,50.0624558166965));
#32730=CARTESIAN_POINT('Ctrl Pts',(-18.9331515858188,21.0579308950032,50.0002872168757));
#32731=CARTESIAN_POINT('Ctrl Pts',(-4.68803869421815,20.3358459902176,43.7834272347982));
#32732=CARTESIAN_POINT('Ctrl Pts',(5.01043897044188,20.3259687935359,28.7584631807949));
#32733=CARTESIAN_POINT('Ctrl Pts',(5.05269305461643,20.1386280586979,13.2396204439751));
#32734=CARTESIAN_POINT('Ctrl Pts',(-19.3604772176933,21.0805877228818,50.1867950698636));
#32735=CARTESIAN_POINT('Ctrl Pts',(-19.218024598263,21.0733705912361,50.1246283015585));
#32736=CARTESIAN_POINT('Ctrl Pts',(-19.0755719788328,21.0661534595904,50.0624615332534));
#32737=CARTESIAN_POINT('Ctrl Pts',(-18.9331193594025,21.0589363279447,50.0002947649483));
#32738=CARTESIAN_POINT('Ctrl Pts',(-4.68785741637426,20.3372231633746,43.7836179344389));
#32739=CARTESIAN_POINT('Ctrl Pts',(5.01054074711136,20.327757834925,28.7585459165298));
#32740=CARTESIAN_POINT('Ctrl Pts',(5.05286493038735,20.1408116455766,13.2397257566308));
#32741=CARTESIAN_POINT('',(-11.284173078362,20.5529756002005,45.4965192546307));
#32742=CARTESIAN_POINT('Ctrl Pts',(4.37484296764849,19.9464420456703,20.1714550984892));
#32743=CARTESIAN_POINT('Ctrl Pts',(3.44448305305149,20.0189549105364,25.1661789821446));
#32744=CARTESIAN_POINT('Ctrl Pts',(1.55215272586899,20.0954766247834,29.9700084636964));
#32745=CARTESIAN_POINT('Ctrl Pts',(-3.79011625520565,20.2752040736288,38.6053112430901));
#32746=CARTESIAN_POINT('Ctrl Pts',(-7.23855178728743,20.3824974081048,42.4380069630988));
#32747=CARTESIAN_POINT('Ctrl Pts',(-11.284173078368,20.5529756002053,45.4965192546226));
#32748=CARTESIAN_POINT('',(-11.2641171037461,20.7105311502992,45.5014889049172));
#32749=CARTESIAN_POINT('',(-11.2841730783683,20.5529756002016,45.4965192546224));
#32750=CARTESIAN_POINT('Ctrl Pts',(-11.264117103744,20.7105311502982,45.50148890492));
#32751=CARTESIAN_POINT('Ctrl Pts',(-7.12723823252845,20.5483438544847,42.3780169116778));
#32752=CARTESIAN_POINT('Ctrl Pts',(-3.61607404464229,20.4520245495079,38.4420106405091));
#32753=CARTESIAN_POINT('Ctrl Pts',(1.76528630148522,20.3052748660675,29.5836747606129));
#32754=CARTESIAN_POINT('Ctrl Pts',(3.63859976812651,20.248474007324,24.6615284366429));
#32755=CARTESIAN_POINT('Ctrl Pts',(4.50580696382332,20.1925493450898,19.5550277686639));
#32756=CARTESIAN_POINT('Ctrl Pts',(16.3617859818256,-4.68328060676847,50.8901188958912));
#32757=CARTESIAN_POINT('Ctrl Pts',(16.622166238714,-4.67927906663786,50.5796103403414));
#32758=CARTESIAN_POINT('Ctrl Pts',(16.8774519664815,-4.67486342687383,50.2628798120286));
#32759=CARTESIAN_POINT('Ctrl Pts',(17.9410437802702,-4.65418501649615,48.8890505498656));
#32760=CARTESIAN_POINT('Ctrl Pts',(19.4134795663389,-4.61395560865182,46.711300994988));
#32761=CARTESIAN_POINT('Ctrl Pts',(21.157886103088,-4.53496565777432,43.2616774490902));
#32762=CARTESIAN_POINT('Ctrl Pts',(22.6517756066693,-4.42959393838223,39.075796489912));
#32763=CARTESIAN_POINT('Ctrl Pts',(23.4697878015651,-4.31850354734918,34.7535560407194));
#32764=CARTESIAN_POINT('Ctrl Pts',(23.6135578037238,-4.2170896233612,30.3929554510995));
#32765=CARTESIAN_POINT('Ctrl Pts',(23.2191400843552,-4.13063759391767,26.0539326403806));
#32766=CARTESIAN_POINT('Ctrl Pts',(22.1536599527665,-4.07121155600733,21.8071760633296));
#32767=CARTESIAN_POINT('Ctrl Pts',(20.4200758048662,-4.04803120464602,17.7504657469389));
#32768=CARTESIAN_POINT('Ctrl Pts',(18.4775377675087,-4.055480889925,14.4481772758194));
#32769=CARTESIAN_POINT('Ctrl Pts',(16.8791012600192,-4.07952578289679,12.3929056948357));
#32770=CARTESIAN_POINT('Ctrl Pts',(15.7266400983712,-4.10152925776619,11.0970184802139));
#32771=CARTESIAN_POINT('Ctrl Pts',(15.4437103800753,-4.1072571624472,10.7918674138708));
#32772=CARTESIAN_POINT('Ctrl Pts',(15.155735551125,-4.11341014061892,10.4938062779888));
#32773=CARTESIAN_POINT('Ctrl Pts',(16.0716182464065,-4.24009445412503,50.8866381127899));
#32774=CARTESIAN_POINT('Ctrl Pts',(16.3335846412505,-4.23725223817857,50.5777035993082));
#32775=CARTESIAN_POINT('Ctrl Pts',(16.5905075369587,-4.23400446880359,50.2625298947483));
#32776=CARTESIAN_POINT('Ctrl Pts',(17.6612842305945,-4.21832863439708,48.8952428878293));
#32777=CARTESIAN_POINT('Ctrl Pts',(19.1454696712926,-4.18572164472913,46.7268968947991));
#32778=CARTESIAN_POINT('Ctrl Pts',(20.9096158518361,-4.11799618192084,43.2893924007819));
#32779=CARTESIAN_POINT('Ctrl Pts',(22.4288153906464,-4.02550335874969,39.115138864075));
#32780=CARTESIAN_POINT('Ctrl Pts',(23.2747425690519,-3.92690475481451,34.801140787119));
#32781=CARTESIAN_POINT('Ctrl Pts',(23.448651990639,-3.83755718932749,30.4450413824504));
#32782=CARTESIAN_POINT('Ctrl Pts',(23.0859365661942,-3.76285616468038,26.1073385430749));
#32783=CARTESIAN_POINT('Ctrl Pts',(22.0538376043168,-3.71481495977278,21.8577037769588));
#32784=CARTESIAN_POINT('Ctrl Pts',(20.3548967622918,-3.70275434803773,17.7935954675031));
#32785=CARTESIAN_POINT('Ctrl Pts',(18.4427064539546,-3.71962751323487,14.4817346886381));
#32786=CARTESIAN_POINT('Ctrl Pts',(16.8648199692177,-3.74992063397164,12.4178382951194));
#32787=CARTESIAN_POINT('Ctrl Pts',(15.7259553229615,-3.77604797989279,11.1155040507245));
#32788=CARTESIAN_POINT('Ctrl Pts',(15.4462443232874,-3.78276245762616,10.8087153709496));
#32789=CARTESIAN_POINT('Ctrl Pts',(15.1614301028927,-3.78989370687861,10.5089349485779));
#32790=CARTESIAN_POINT('Ctrl Pts',(15.775594122299,-3.80075287541765,50.8831473876396));
#32791=CARTESIAN_POINT('Ctrl Pts',(16.0391680422694,-3.79905339336963,50.5757898857823));
#32792=CARTESIAN_POINT('Ctrl Pts',(16.2977495463562,-3.79695621683146,50.262175383072));
#32793=CARTESIAN_POINT('Ctrl Pts',(17.3758025240791,-3.78620663871065,48.9014382062803));
#32794=CARTESIAN_POINT('Ctrl Pts',(18.8718656085796,-3.76109400159902,46.7425044935959));
#32795=CARTESIAN_POINT('Ctrl Pts',(20.6559095081701,-3.70440674399875,43.3171275041978));
#32796=CARTESIAN_POINT('Ctrl Pts',(22.2005654978869,-3.62448835210827,39.1545089959556));
#32797=CARTESIAN_POINT('Ctrl Pts',(23.0745120366084,-3.53802316526296,34.8487637167761));
#32798=CARTESIAN_POINT('Ctrl Pts',(23.2786330544031,-3.46032715355504,30.4971820176086));
#32799=CARTESIAN_POINT('Ctrl Pts',(22.9476767342877,-3.39690914788247,26.1608222559414));
#32800=CARTESIAN_POINT('Ctrl Pts',(21.9490106855406,-3.35971861494906,21.9083363993147));
#32801=CARTESIAN_POINT('Ctrl Pts',(20.2847821490872,-3.35817927654809,17.8368515221065));
#32802=CARTESIAN_POINT('Ctrl Pts',(18.4030315624581,-3.38391914529348,14.515421853483));
#32803=CARTESIAN_POINT('Ctrl Pts',(16.8457803567792,-3.42007079724739,12.4428866920255));
#32804=CARTESIAN_POINT('Ctrl Pts',(15.7205799195479,-3.45006162272336,11.1340878840826));
#32805=CARTESIAN_POINT('Ctrl Pts',(15.4441049216842,-3.45770043113048,10.8256556958562));
#32806=CARTESIAN_POINT('Ctrl Pts',(15.1624694438579,-3.46574819271174,10.5241484978699));
#32807=CARTESIAN_POINT('Ctrl Pts',(14.711130350501,-2.2653457359543,50.8708167537008));
#32808=CARTESIAN_POINT('Ctrl Pts',(14.9804500746946,-2.26761569662348,50.5690252215433));
#32809=CARTESIAN_POINT('Ctrl Pts',(15.2449567812268,-2.26951335386862,50.2609131963582));
#32810=CARTESIAN_POINT('Ctrl Pts',(16.3489904126773,-2.27586002752392,48.9232880647604));
#32811=CARTESIAN_POINT('Ctrl Pts',(17.8873879492628,-2.27671432942662,46.7975592517765));
#32812=CARTESIAN_POINT('Ctrl Pts',(19.7421505042058,-2.25814179129592,43.4149557959663));
#32813=CARTESIAN_POINT('Ctrl Pts',(21.3770820388576,-2.2214798205824,39.2933713189624));
#32814=CARTESIAN_POINT('Ctrl Pts',(22.3501898623555,-2.17652897108851,35.016748143073));
#32815=CARTESIAN_POINT('Ctrl Pts',(22.6610854561747,-2.13845241575724,30.6811445102227));
#32816=CARTESIAN_POINT('Ctrl Pts',(22.442302689862,-2.11316923258448,26.3495962450917));
#32817=CARTESIAN_POINT('Ctrl Pts',(21.5616897778755,-2.11235831802136,22.0871532550128));
#32818=CARTESIAN_POINT('Ctrl Pts',(20.0200811689669,-2.14581153060268,17.9897419444869));
#32819=CARTESIAN_POINT('Ctrl Pts',(18.2459645155416,-2.20085463389179,14.6345975930576));
#32820=CARTESIAN_POINT('Ctrl Pts',(16.7617576425575,-2.25628908058851,12.5315664711582));
#32821=CARTESIAN_POINT('Ctrl Pts',(15.684964406382,-2.29898278275007,11.1999224907658));
#32822=CARTESIAN_POINT('Ctrl Pts',(15.4199619835964,-2.30966173471912,10.8856758941311));
#32823=CARTESIAN_POINT('Ctrl Pts',(15.1496042586498,-2.32072459453129,10.5780537474731));
#32824=CARTESIAN_POINT('Ctrl Pts',(12.7120990401115,0.42091842584111,50.8486555071386));
#32825=CARTESIAN_POINT('Ctrl Pts',(12.9919285081875,0.412015546281074,50.5568402051828));
#32826=CARTESIAN_POINT('Ctrl Pts',(13.2672633776138,0.403442573942463,50.2585955704578));
#32827=CARTESIAN_POINT('Ctrl Pts',(14.4187373325809,0.368526239150617,48.962439393581));
#32828=CARTESIAN_POINT('Ctrl Pts',(16.0343139487426,0.324281374370589,46.8962890085149));
#32829=CARTESIAN_POINT('Ctrl Pts',(18.0176707105305,0.279215865745994,43.5904340408452));
#32830=CARTESIAN_POINT('Ctrl Pts',(19.8164276316666,0.243759038204317,39.5424793938405));
#32831=CARTESIAN_POINT('Ctrl Pts',(20.9691269648152,0.21967725703067,35.3181165575201));
#32832=CARTESIAN_POINT('Ctrl Pts',(21.4731024416312,0.192114722189047,31.0111945273764));
#32833=CARTESIAN_POINT('Ctrl Pts',(21.4569532754525,0.154437491851918,26.6882970928525));
#32834=CARTESIAN_POINT('Ctrl Pts',(20.7893622142715,0.0954817696064694,
22.4080135319735));
#32835=CARTESIAN_POINT('Ctrl Pts',(19.4688186408849,0.0048363712043943,
18.2641179914593));
#32836=CARTESIAN_POINT('Ctrl Pts',(17.8886301147695,-0.0979118428630517,
14.8485179207147));
#32837=CARTESIAN_POINT('Ctrl Pts',(16.5359594711211,-0.184631554593919,
12.6907998414015));
#32838=CARTESIAN_POINT('Ctrl Pts',(15.546316269121,-0.247909792323189,11.3181882229936));
#32839=CARTESIAN_POINT('Ctrl Pts',(15.3019963909978,-0.263520166061751,
10.9935053189798));
#32840=CARTESIAN_POINT('Ctrl Pts',(15.0519971607038,-0.279478515480188,
10.6748977105072));
#32841=CARTESIAN_POINT('Ctrl Pts',(9.60863066089747,3.93922736422659,50.8171955610112));
#32842=CARTESIAN_POINT('Ctrl Pts',(9.90380565178832,3.92273017306588,50.5393909649465));
#32843=CARTESIAN_POINT('Ctrl Pts',(10.1949269853701,3.90651491483579,50.2550114362429));
#32844=CARTESIAN_POINT('Ctrl Pts',(11.415467332142,3.83888692720806,49.0171607997061));
#32845=CARTESIAN_POINT('Ctrl Pts',(13.1430409691099,3.74496038387833,47.0347818971594));
#32846=CARTESIAN_POINT('Ctrl Pts',(15.312014670943,3.6271896762232,43.8368541553498));
#32847=CARTESIAN_POINT('Ctrl Pts',(17.3462446376419,3.50969140214063,39.8924608868101));
#32848=CARTESIAN_POINT('Ctrl Pts',(18.7559848214645,3.40771510315772,35.7416355306005));
#32849=CARTESIAN_POINT('Ctrl Pts',(19.5353770821765,3.30695483103527,31.4751239969068));
#32850=CARTESIAN_POINT('Ctrl Pts',(19.8076156218556,3.1998573133211,27.1644954735594));
#32851=CARTESIAN_POINT('Ctrl Pts',(19.4424544689053,3.07607789704229,22.8592635001078));
#32852=CARTESIAN_POINT('Ctrl Pts',(18.4351120717144,2.92448144596071,18.6501806821044));
#32853=CARTESIAN_POINT('Ctrl Pts',(17.1292759578971,2.77158317941627,15.1497511982359));
#32854=CARTESIAN_POINT('Ctrl Pts',(15.9624469754747,2.65236568914073,12.9152769022098));
#32855=CARTESIAN_POINT('Ctrl Pts',(15.0958611037723,2.56779645721963,11.4851600873672));
#32856=CARTESIAN_POINT('Ctrl Pts',(14.8808083544882,2.54707902977605,11.1458176192315));
#32857=CARTESIAN_POINT('Ctrl Pts',(14.6596795118079,2.52604544176493,10.81176741508));
#32858=CARTESIAN_POINT('Ctrl Pts',(5.74244455804017,7.64857049485316,50.7803662328039));
#32859=CARTESIAN_POINT('Ctrl Pts',(6.05569741160819,7.62538079009264,50.5186066375066));
#32860=CARTESIAN_POINT('Ctrl Pts',(6.36538250903781,7.6024320797305,50.2501220962308));
#32861=CARTESIAN_POINT('Ctrl Pts',(7.66700342527438,7.50598047950645,49.0791935344687));
#32862=CARTESIAN_POINT('Ctrl Pts',(9.52575081707664,7.36825978906471,47.1929758832822));
#32863=CARTESIAN_POINT('Ctrl Pts',(11.9112808060609,7.18657585481396,44.1189689523312));
#32864=CARTESIAN_POINT('Ctrl Pts',(14.2193661405577,6.99739878870591,40.2935266180449));
#32865=CARTESIAN_POINT('Ctrl Pts',(15.9270736912541,6.82819742189185,36.2272337144719));
#32866=CARTESIAN_POINT('Ctrl Pts',(17.024880309348,6.66543158101024,32.0072748538597));
#32867=CARTESIAN_POINT('Ctrl Pts',(17.6299082160355,6.50060855796851,27.7109331227746));
#32868=CARTESIAN_POINT('Ctrl Pts',(17.6130179265134,6.32441606849526,23.3773141230994));
#32869=CARTESIAN_POINT('Ctrl Pts',(16.9656867939234,6.12505774886043,19.093703489216));
#32870=CARTESIAN_POINT('Ctrl Pts',(15.9747785941321,5.93384517916791,15.496190967554));
#32871=CARTESIAN_POINT('Ctrl Pts',(15.0210039512143,5.79035915091665,13.1738276179752));
#32872=CARTESIAN_POINT('Ctrl Pts',(14.295408729852,5.69001969995687,11.6778536150283));
#32873=CARTESIAN_POINT('Ctrl Pts',(14.1139837591531,5.66551509710643,11.3217339373774));
#32874=CARTESIAN_POINT('Ctrl Pts',(13.9261211880402,5.64071489355821,10.9700178599298));
#32875=CARTESIAN_POINT('Ctrl Pts',(2.10026812882245,10.6050661536892,50.7471135490468));
#32876=CARTESIAN_POINT('Ctrl Pts',(2.42970188215053,10.5777689837161,50.4994231232871));
#32877=CARTESIAN_POINT('Ctrl Pts',(2.75597229567527,10.5506896266998,50.2448900518966));
#32878=CARTESIAN_POINT('Ctrl Pts',(4.12990684291117,10.4365567481294,49.1327687224161));
#32879=CARTESIAN_POINT('Ctrl Pts',(6.10543909625537,10.2719415070743,47.3310635731816));
#32880=CARTESIAN_POINT('Ctrl Pts',(8.68319308440481,10.0511774947007,44.3660022123056));
#32881=CARTESIAN_POINT('Ctrl Pts',(11.2337573042792,9.81863871620139,40.6451852338454));
#32882=CARTESIAN_POINT('Ctrl Pts',(13.2046001804074,9.60967367489776,36.6533198393472));
#32883=CARTESIAN_POINT('Ctrl Pts',(14.5829691071597,9.41153176383594,32.4744597064717));
#32884=CARTESIAN_POINT('Ctrl Pts',(15.4807568161021,9.21500541081661,28.1908990385021));
#32885=CARTESIAN_POINT('Ctrl Pts',(15.769686211672,9.01175979868378,23.8326054364364));
#32886=CARTESIAN_POINT('Ctrl Pts',(15.4379491375815,8.78956564702969,19.4838165836314));
#32887=CARTESIAN_POINT('Ctrl Pts',(14.722757944353,8.58124477590158,15.8012895296554));
#32888=CARTESIAN_POINT('Ctrl Pts',(13.9552770836213,8.42762540105217,13.4019109616667));
#32889=CARTESIAN_POINT('Ctrl Pts',(13.3528872797445,8.32086564673385,11.8482144895222));
#32890=CARTESIAN_POINT('Ctrl Pts',(13.2009274270766,8.29482075310626,11.4774240473852));
#32891=CARTESIAN_POINT('Ctrl Pts',(13.0422921111672,8.26849188852043,11.1102890366025));
#32892=CARTESIAN_POINT('Ctrl Pts',(-2.32344597549834,13.6252616883324,50.7074105587169));
#32893=CARTESIAN_POINT('Ctrl Pts',(-1.9752998919414,13.5952855444977,50.4758359591679));
#32894=CARTESIAN_POINT('Ctrl Pts',(-1.62988469132187,13.5655149131873,50.2372979642494));
#32895=CARTESIAN_POINT('Ctrl Pts',(-0.172623734997204,13.4398628522405,
49.1926684568959));
#32896=CARTESIAN_POINT('Ctrl Pts',(1.93734073331834,13.2576618204372,47.4879749039095));
#32897=CARTESIAN_POINT('Ctrl Pts',(4.73595880494755,13.0115743729063,44.6480286235722));
#32898=CARTESIAN_POINT('Ctrl Pts',(7.56468089622281,12.751644575675,41.0474413376908));
#32899=CARTESIAN_POINT('Ctrl Pts',(9.83683823314094,12.5189796899122,37.1412195468378));
#32900=CARTESIAN_POINT('Ctrl Pts',(11.535949107776,12.301865256328,33.0098190474629));
#32901=CARTESIAN_POINT('Ctrl Pts',(12.7680096168006,12.0904144587841,28.7412692264177));
#32902=CARTESIAN_POINT('Ctrl Pts',(13.4056044510136,11.8774764455751,24.3550594803262));
#32903=CARTESIAN_POINT('Ctrl Pts',(13.4331412637371,11.6504923923572,19.9319241108741));
#32904=CARTESIAN_POINT('Ctrl Pts',(13.0314530758916,11.4410171343385,16.1522546984861));
#32905=CARTESIAN_POINT('Ctrl Pts',(12.4755385167765,11.2882220371981,13.6647941021625));
#32906=CARTESIAN_POINT('Ctrl Pts',(12.0129796713749,11.1823584691134,12.0450596698024));
#32907=CARTESIAN_POINT('Ctrl Pts',(11.8945374044748,11.1565388193505,11.657551735864));
#32908=CARTESIAN_POINT('Ctrl Pts',(11.7692258288562,11.1304479812224,11.2729059637599));
#32909=CARTESIAN_POINT('Ctrl Pts',(-6.40110428036058,15.9398275064074,50.6708432675152));
#32910=CARTESIAN_POINT('Ctrl Pts',(-6.03650538939953,15.9092719019138,50.4534079698693));
#32911=CARTESIAN_POINT('Ctrl Pts',(-5.67428759415347,15.8789225535602,50.2289124185247));
#32912=CARTESIAN_POINT('Ctrl Pts',(-4.14402253391207,15.7507918597713,49.2435830363373));
#32913=CARTESIAN_POINT('Ctrl Pts',(-1.91634595810908,15.5646999212503,47.6241454237767));
#32914=CARTESIAN_POINT('Ctrl Pts',(1.07545108130911,15.3133344724918,44.8942114163047));
#32915=CARTESIAN_POINT('Ctrl Pts',(4.14720811862536,15.0487502016962,41.3994183816965));
#32916=CARTESIAN_POINT('Ctrl Pts',(6.68230321143587,14.8142492774957,37.5686748221223));
#32917=CARTESIAN_POINT('Ctrl Pts',(8.66095132605825,14.5991383033468,33.4792697502678));
#32918=CARTESIAN_POINT('Ctrl Pts',(10.1840492935139,14.3930646018661,29.2242550823646));
#32919=CARTESIAN_POINT('Ctrl Pts',(11.1248270635106,14.1899609567462,24.8139220984123));
#32920=CARTESIAN_POINT('Ctrl Pts',(11.46434688115,13.977122935371,20.3259202309031));
#32921=CARTESIAN_POINT('Ctrl Pts',(11.3345865749015,13.7824369346935,16.4613224208427));
#32922=CARTESIAN_POINT('Ctrl Pts',(10.9619607427361,13.6409944051188,13.8967724687642));
#32923=CARTESIAN_POINT('Ctrl Pts',(10.6204652415869,13.5429643472183,12.2192199886043));
#32924=CARTESIAN_POINT('Ctrl Pts',(10.5310903287026,13.5190447294408,11.8171499065311));
#32925=CARTESIAN_POINT('Ctrl Pts',(10.4347273407624,13.4948677704672,11.4173185836932));
#32926=CARTESIAN_POINT('Ctrl Pts',(-11.2581355126793,18.188947172369,50.6263769819591));
#32927=CARTESIAN_POINT('Ctrl Pts',(-10.874837896557,18.1597316481657,50.4251496671371));
#32928=CARTESIAN_POINT('Ctrl Pts',(-10.4935569470502,18.1307342364494,50.2167577112658));
#32929=CARTESIAN_POINT('Ctrl Pts',(-8.88060641151116,18.0083786966032,49.2994700730556));
#32930=CARTESIAN_POINT('Ctrl Pts',(-6.51959375012864,17.830846834045,47.7778825471059));
#32931=CARTESIAN_POINT('Ctrl Pts',(-3.30898627378599,17.5925027676131,45.1742926484351));
#32932=CARTESIAN_POINT('Ctrl Pts',(0.0379893981926304,17.3443426911773,
41.801106220426));
#32933=CARTESIAN_POINT('Ctrl Pts',(2.87070487089537,17.1289494695207,38.0572826893845));
#32934=CARTESIAN_POINT('Ctrl Pts',(5.16554290078262,16.9369213116231,34.0164684807631));
#32935=CARTESIAN_POINT('Ctrl Pts',(7.01762411454711,16.7575317657622,29.7774553228848));
#32936=CARTESIAN_POINT('Ctrl Pts',(8.30079284685546,16.5859876106103,25.3399902329922));
#32937=CARTESIAN_POINT('Ctrl Pts',(8.99223520193867,16.4095763329362,20.7781720131405));
#32938=CARTESIAN_POINT('Ctrl Pts',(9.16889682817149,16.2491906636996,16.8166904505901));
#32939=CARTESIAN_POINT('Ctrl Pts',(9.00256941244382,16.1323920433636,14.1640860328959));
#32940=CARTESIAN_POINT('Ctrl Pts',(8.7972460292566,16.0510402241362,12.4204614509089));
#32941=CARTESIAN_POINT('Ctrl Pts',(8.74059622159544,16.0311583490605,12.0018473869615));
#32942=CARTESIAN_POINT('Ctrl Pts',(8.67685658165753,16.01103806515,11.5848534084937));
#32943=CARTESIAN_POINT('Ctrl Pts',(-15.657276494051,19.7983627848149,50.5847597853741));
#32944=CARTESIAN_POINT('Ctrl Pts',(-15.2578253879166,19.7720645135703,50.3977633519486));
#32945=CARTESIAN_POINT('Ctrl Pts',(-14.860102865805,19.7460021313493,50.2035126492778));
#32946=CARTESIAN_POINT('Ctrl Pts',(-13.175951969311,19.6361820466171,49.3459910091793));
#32947=CARTESIAN_POINT('Ctrl Pts',(-10.7000587998586,19.4774394485581,47.9103778968689));
#32948=CARTESIAN_POINT('Ctrl Pts',(-7.30079683975733,19.2670183310104,45.4178765118453));
#32949=CARTESIAN_POINT('Ctrl Pts',(-3.71645296456281,19.0520629838802,42.1517164114004));
#32950=CARTESIAN_POINT('Ctrl Pts',(-0.627027603513927,18.8717166252608,
38.4845463961827));
#32951=CARTESIAN_POINT('Ctrl Pts',(1.94045298184077,18.7178122962125,34.4868040712865));
#32952=CARTESIAN_POINT('Ctrl Pts',(4.07608978829918,18.5794411422907,30.2623003349598));
#32953=CARTESIAN_POINT('Ctrl Pts',(5.65415883179733,18.4529446490623,25.8015291609108));
#32954=CARTESIAN_POINT('Ctrl Pts',(6.64840096894227,18.3257380682571,21.1754591429953));
#32955=CARTESIAN_POINT('Ctrl Pts',(7.08845542629894,18.2102139945187,17.1294161466707));
#32956=CARTESIAN_POINT('Ctrl Pts',(7.09925335497196,18.1249152482566,14.3998463939675));
#32957=CARTESIAN_POINT('Ctrl Pts',(7.0107674651366,18.064727637235,12.5984411589748));
#32958=CARTESIAN_POINT('Ctrl Pts',(6.982201638659,18.0499634327475,12.1654452776201));
#32959=CARTESIAN_POINT('Ctrl Pts',(6.94646609919288,18.0349776243875,11.7336121997143));
#32960=CARTESIAN_POINT('Ctrl Pts',(-18.8793254736515,20.6836496418694,50.5527496580464));
#32961=CARTESIAN_POINT('Ctrl Pts',(-18.468609657083,20.6606519170286,50.3759538221809));
#32962=CARTESIAN_POINT('Ctrl Pts',(-18.0594351009059,20.6379063239872,50.1918393727547));
#32963=CARTESIAN_POINT('Ctrl Pts',(-16.3257493528884,20.5422448076096,49.3771603969211));
#32964=CARTESIAN_POINT('Ctrl Pts',(-13.7698304039347,20.4047755971079,48.0031978573159));
#32965=CARTESIAN_POINT('Ctrl Pts',(-10.2389125796356,20.225761668211,45.5904189129039));
#32966=CARTESIAN_POINT('Ctrl Pts',(-6.4887184482965,20.0475517349526,42.4011488849344));
#32967=CARTESIAN_POINT('Ctrl Pts',(-3.21976533941777,19.9048724048602,38.7891722537331));
#32968=CARTESIAN_POINT('Ctrl Pts',(-0.461559957111977,19.790507905872,34.8226183318397));
#32969=CARTESIAN_POINT('Ctrl Pts',(1.87242626469179,19.6935273080542,30.6088777136648));
#32970=CARTESIAN_POINT('Ctrl Pts',(3.65670540538569,19.6110850660289,26.1318176353169));
#32971=CARTESIAN_POINT('Ctrl Pts',(4.86251201139915,19.530779076001,21.4601528010746));
#32972=CARTESIAN_POINT('Ctrl Pts',(5.48643851700597,19.4573327991495,17.3539164024331));
#32973=CARTESIAN_POINT('Ctrl Pts',(5.6207501220497,19.4012238336331,14.5694714880378));
#32974=CARTESIAN_POINT('Ctrl Pts',(5.61368274593469,19.3605693891818,12.7268457580551));
#32975=CARTESIAN_POINT('Ctrl Pts',(5.60468015267822,19.3505226070412,12.2836407679017));
#32976=CARTESIAN_POINT('Ctrl Pts',(5.58844640000097,19.3402634731691,11.8413221987243));
#32977=CARTESIAN_POINT('Ctrl Pts',(-20.6920217811532,21.117312799858,50.5343146756899));
#32978=CARTESIAN_POINT('Ctrl Pts',(-20.2750932994788,21.0964267127388,50.3632222074524));
#32979=CARTESIAN_POINT('Ctrl Pts',(-19.8596072866037,21.0758020890032,50.1847744350595));
#32980=CARTESIAN_POINT('Ctrl Pts',(-18.098641284761,20.9891913310095,49.3940446371234));
#32981=CARTESIAN_POINT('Ctrl Pts',(-15.4986177759893,20.8653273744228,48.0545498997513));
#32982=CARTESIAN_POINT('Ctrl Pts',(-11.8950631088073,20.7063681300896,45.6863574981545));
#32983=CARTESIAN_POINT('Ctrl Pts',(-8.05329901501471,20.5515335415639,42.540109695465));
#32984=CARTESIAN_POINT('Ctrl Pts',(-4.68516379227482,20.4326519806542,38.9590447934805));
#32985=CARTESIAN_POINT('Ctrl Pts',(-1.8215597727922,20.3430531321453,35.0099997569466));
#32986=CARTESIAN_POINT('Ctrl Pts',(0.62204841812851,20.2718184169426,30.8023618711775));
#32987=CARTESIAN_POINT('Ctrl Pts',(2.52028916562565,20.2165549432469,26.3162953955452));
#32988=CARTESIAN_POINT('Ctrl Pts',(3.84298678509366,20.164982094833,21.6192526187751));
#32989=CARTESIAN_POINT('Ctrl Pts',(4.56847237094525,20.117197691553,17.4794679698934));
#32990=CARTESIAN_POINT('Ctrl Pts',(4.77097609751765,20.0788282397779,14.6644175519522));
#32991=CARTESIAN_POINT('Ctrl Pts',(4.8088478494176,20.0500302875854,12.7987962353339));
#32992=CARTESIAN_POINT('Ctrl Pts',(4.81063894211702,20.0428451797642,12.3499110360814));
#32993=CARTESIAN_POINT('Ctrl Pts',(4.80516116754767,20.0354515632684,11.9017729301386));
#32994=CARTESIAN_POINT('Ctrl Pts',(-21.2075547412075,21.2334813897109,50.5290240335005));
#32995=CARTESIAN_POINT('Ctrl Pts',(-20.7888675617946,21.2132228077857,50.3595499677703));
#32996=CARTESIAN_POINT('Ctrl Pts',(-20.371595394195,21.1932283095702,50.1827099013443));
#32997=CARTESIAN_POINT('Ctrl Pts',(-18.6029112980843,21.1093059289188,49.3987736984652));
#32998=CARTESIAN_POINT('Ctrl Pts',(-15.9904109360945,20.9894835119608,48.0690557864224));
#32999=CARTESIAN_POINT('Ctrl Pts',(-12.3663152507135,20.8364792943525,45.7135099205708));
#33000=CARTESIAN_POINT('Ctrl Pts',(-8.49866891037799,20.6885792302246,42.5794650410989));
#33001=CARTESIAN_POINT('Ctrl Pts',(-5.10252178725963,20.5767478260626,39.0071711643947));
#33002=CARTESIAN_POINT('Ctrl Pts',(-2.20917801324067,20.4944756050622,35.0631014711985));
#33003=CARTESIAN_POINT('Ctrl Pts',(0.265331834530177,20.4308554028779,30.8572109582053));
#33004=CARTESIAN_POINT('Ctrl Pts',(2.19565922030913,20.3836340081555,26.3686156145749));
#33005=CARTESIAN_POINT('Ctrl Pts',(3.55122733547804,20.340580727313,21.6644068254319));
#33006=CARTESIAN_POINT('Ctrl Pts',(4.30524135296048,20.3004356869138,17.5151329967541));
#33007=CARTESIAN_POINT('Ctrl Pts',(4.52688653784348,20.2673681898868,14.6914125247235));
#33008=CARTESIAN_POINT('Ctrl Pts',(4.57736918620936,20.2421246596599,12.8192708069574));
#33009=CARTESIAN_POINT('Ctrl Pts',(4.58218835934103,20.2357981340653,12.3687776821398));
#33010=CARTESIAN_POINT('Ctrl Pts',(4.57972725339752,20.2292648564311,11.9189947438633));
#33011=CARTESIAN_POINT('Ctrl Pts',(-21.7245808409968,21.3428689572265,50.5236748853477));
#33012=CARTESIAN_POINT('Ctrl Pts',(-21.3041387087102,21.323266505305,50.3558195556542));
#33013=CARTESIAN_POINT('Ctrl Pts',(-20.8850843833989,21.303930781031,50.180587353719));
#33014=CARTESIAN_POINT('Ctrl Pts',(-19.1087003760649,21.2228186866547,49.4034447585614));
#33015=CARTESIAN_POINT('Ctrl Pts',(-16.4837535272471,21.1072213437662,48.0835031545822));
#33016=CARTESIAN_POINT('Ctrl Pts',(-12.8391736157711,20.9604400919523,45.7406026391106));
#33017=CARTESIAN_POINT('Ctrl Pts',(-8.94572887548127,20.819779963638,42.6187594657614));
#33018=CARTESIAN_POINT('Ctrl Pts',(-5.52168169435916,20.7152993064879,39.055238489401));
#33019=CARTESIAN_POINT('Ctrl Pts',(-2.59874401318366,20.6406553883908,35.1161518300549));
#33020=CARTESIAN_POINT('Ctrl Pts',(-0.0935133882118095,20.5849601975755,
30.912023564341));
#33021=CARTESIAN_POINT('Ctrl Pts',(1.8686749135023,20.5461109852346,26.4209236529955));
#33022=CARTESIAN_POINT('Ctrl Pts',(3.25684131524749,20.5119420676311,21.7095802099905));
#33023=CARTESIAN_POINT('Ctrl Pts',(4.03911612791383,20.4797911688045,17.5508438837181));
#33024=CARTESIAN_POINT('Ctrl Pts',(4.27970845737112,20.4522911786996,14.7184653460843));
#33025=CARTESIAN_POINT('Ctrl Pts',(4.34267005657433,20.4307901345004,12.839806484766));
#33026=CARTESIAN_POINT('Ctrl Pts',(4.35048498829163,20.4253683033402,12.3877080831818));
#33027=CARTESIAN_POINT('Ctrl Pts',(4.3510077184132,20.4197421663948,11.9362847456263));
#33028=CARTESIAN_POINT('',(20.8964130901555,-3.27137079310494,41.9595781864667));
#33029=CARTESIAN_POINT('Ctrl Pts',(20.8964126143753,-3.27137063675447,41.9595776658638));
#33030=CARTESIAN_POINT('Ctrl Pts',(21.1817218893114,-3.25992113527386,41.237174740169));
#33031=CARTESIAN_POINT('Ctrl Pts',(21.4383847013129,-3.24789097083339,40.506795170327));
#33032=CARTESIAN_POINT('Ctrl Pts',(21.666400175533,-3.23555894847836,39.7701345246277));
#33033=CARTESIAN_POINT('Ctrl Pts',(22.2248182238258,-3.20535738484082,37.9660262664815));
#33034=CARTESIAN_POINT('Ctrl Pts',(22.6114159538701,-3.17334534500276,36.1242455215656));
#33035=CARTESIAN_POINT('Ctrl Pts',(22.8263278926835,-3.14345008158506,34.2697199800252));
#33036=CARTESIAN_POINT('Ctrl Pts',(22.9696025185028,-3.12351990598109,33.0333696194841));
#33037=CARTESIAN_POINT('Ctrl Pts',(23.0365723482865,-3.10453051989494,31.7913549048711));
#33038=CARTESIAN_POINT('Ctrl Pts',(23.0273212361039,-3.08752071373526,30.5510624649799));
#33039=CARTESIAN_POINT('Ctrl Pts',(23.0180701239261,-3.07051090758448,29.310770025738));
#33040=CARTESIAN_POINT('Ctrl Pts',(22.9325980698661,-3.0554806813514,28.0721998612096));
#33041=CARTESIAN_POINT('Ctrl Pts',(22.7710068479441,-3.04339100491456,26.842736737895));
#33042=CARTESIAN_POINT('Ctrl Pts',(22.5286200153623,-3.02525649028182,24.9985420552148));
#33043=CARTESIAN_POINT('Ctrl Pts',(22.1149650555836,-3.01373821257335,23.1748382152102));
#33044=CARTESIAN_POINT('Ctrl Pts',(21.5304984053267,-3.01128625574909,21.396513212607));
#33045=CARTESIAN_POINT('Ctrl Pts',(21.1408539727369,-3.00965161787009,20.2109632136553));
#33046=CARTESIAN_POINT('Ctrl Pts',(20.6752932336029,-3.01204645592803,19.0455815867227));
#33047=CARTESIAN_POINT('Ctrl Pts',(20.133973937495,-3.01891855380822,17.9077259948654));
#33048=CARTESIAN_POINT('Ctrl Pts',(19.5926547062943,-3.02579065086441,16.769870539443));
#33049=CARTESIAN_POINT('Ctrl Pts',(18.97557693629,-3.03714000665748,15.6595411124551));
#33050=CARTESIAN_POINT('Ctrl Pts',(18.2829028015464,-3.05321938564873,14.5840810598834));
#33051=CARTESIAN_POINT('Ctrl Pts',(17.9974751370287,-3.05984515577954,14.1409202203334));
#33052=CARTESIAN_POINT('Ctrl Pts',(17.6992113166365,-3.06727406915266,13.703680165412));
#33053=CARTESIAN_POINT('Ctrl Pts',(17.3881232046069,-3.07550335254719,13.2728733070379));
#33054=CARTESIAN_POINT('Ctrl Pts',(20.8964126457139,-3.2713711968523,41.9595783997524));
#33055=CARTESIAN_POINT('Ctrl Pts',(17.2051685289687,1.76302070836308,43.7978652212161));
#33056=CARTESIAN_POINT('Ctrl Pts',(12.2598686672308,6.26298698655195,45.6247956227673));
#33057=CARTESIAN_POINT('Ctrl Pts',(3.58378438842023,12.5188402359751,46.8259364130367));
#33058=CARTESIAN_POINT('Ctrl Pts',(0.582129726745584,14.4577038460462,46.9709992271213));
#33059=CARTESIAN_POINT('Ctrl Pts',(-5.33701510283081,17.8486390793514,46.6585370539501));
#33060=CARTESIAN_POINT('Ctrl Pts',(-8.30844082698423,19.3555621015299,46.2345691905119));
#33061=CARTESIAN_POINT('Ctrl Pts',(-11.284173078362,20.5529756002005,45.4965192546307));
#33062=CARTESIAN_POINT('Ctrl Pts',(-21.7707507075119,21.2883239772394,50.5183817307192));
#33063=CARTESIAN_POINT('Ctrl Pts',(-21.3522076240192,21.2711623310641,50.3520726044098));
#33064=CARTESIAN_POINT('Ctrl Pts',(-20.9350453013657,21.2542807820542,50.1784403181166));
#33065=CARTESIAN_POINT('Ctrl Pts',(-19.1614547553146,21.1834525291307,49.4060644176876));
#33066=CARTESIAN_POINT('Ctrl Pts',(-16.5379429433396,21.0834264338425,48.0919810552141));
#33067=CARTESIAN_POINT('Ctrl Pts',(-12.8944921326136,20.9598507183575,45.7566603943191));
#33068=CARTESIAN_POINT('Ctrl Pts',(-9.00132135085463,20.8461335954997,42.6421286282473));
#33069=CARTESIAN_POINT('Ctrl Pts',(-5.57643150485377,20.7684839093916,39.0838481962268));
#33070=CARTESIAN_POINT('Ctrl Pts',(-2.6518075273083,20.7206230093664,35.1477051131834));
#33071=CARTESIAN_POINT('Ctrl Pts',(-0.144357875366567,20.6916936542703,
30.9445642263901));
#33072=CARTESIAN_POINT('Ctrl Pts',(1.82053721598537,20.6796111419738,26.4518611209923));
#33073=CARTESIAN_POINT('Ctrl Pts',(3.21164056637826,20.6722203558656,21.7361128259805));
#33074=CARTESIAN_POINT('Ctrl Pts',(3.99646962984073,20.6630225594897,17.5715878573721));
#33075=CARTESIAN_POINT('Ctrl Pts',(4.23871507783227,20.6508204531822,14.7339475749565));
#33076=CARTESIAN_POINT('Ctrl Pts',(4.30264169687323,20.6394053700742,12.8537551580576));
#33077=CARTESIAN_POINT('Ctrl Pts',(4.31069886437243,20.6364191357732,12.403140363483));
#33078=CARTESIAN_POINT('Ctrl Pts',(4.31153534930859,20.6332209087108,11.9532190478412));
#33079=CARTESIAN_POINT('Ctrl Pts',(-21.2368317850234,21.2398788304839,50.5241377112808));
#33080=CARTESIAN_POINT('Ctrl Pts',(-20.8200215229436,21.2217224127637,50.3562407150369));
#33081=CARTESIAN_POINT('Ctrl Pts',(-20.4046183737684,21.2038412173392,50.1810308199636));
#33082=CARTESIAN_POINT('Ctrl Pts',(-18.6386486286545,21.1287309618461,49.4019675760705));
#33083=CARTESIAN_POINT('Ctrl Pts',(-16.0274699089574,21.0222253289507,48.0782465856348));
#33084=CARTESIAN_POINT('Ctrl Pts',(-12.4043187325921,20.8890564489947,45.7304459674085));
#33085=CARTESIAN_POINT('Ctrl Pts',(-8.5367091551944,20.7641817659416,42.6038549902468));
#33086=CARTESIAN_POINT('Ctrl Pts',(-5.1394481455897,20.6752847595175,39.0368823073392));
#33087=CARTESIAN_POINT('Ctrl Pts',(-2.24410526599034,20.6159219251614,35.0957729594708));
#33088=CARTESIAN_POINT('Ctrl Pts',(0.232973273656757,20.5752144761384,30.8908341256496));
#33089=CARTESIAN_POINT('Ctrl Pts',(2.16640899202804,20.5509334123338,26.4005312505802));
#33090=CARTESIAN_POINT('Ctrl Pts',(3.52537408730755,20.5308579865904,21.6917378372941));
#33091=CARTESIAN_POINT('Ctrl Pts',(4.28238402432898,20.510426256151,17.5364645633748));
#33092=CARTESIAN_POINT('Ctrl Pts',(4.50600998813618,20.4905046142392,14.7073007255026));
#33093=CARTESIAN_POINT('Ctrl Pts',(4.55770179730602,20.4739374093561,12.8334827801716));
#33094=CARTESIAN_POINT('Ctrl Pts',(4.56283498494982,20.469713411733,12.3844319227925));
#33095=CARTESIAN_POINT('Ctrl Pts',(4.5607603471881,20.4652767483487,11.936108840748));
#33096=CARTESIAN_POINT('Ctrl Pts',(-20.7026953550296,21.1822016013635,50.5298372191554));
#33097=CARTESIAN_POINT('Ctrl Pts',(-20.2876361428746,21.1630886105529,50.360345202981));
#33098=CARTESIAN_POINT('Ctrl Pts',(-19.8740110101105,21.1442460408093,50.1835506652342));
#33099=CARTESIAN_POINT('Ctrl Pts',(-18.1157451993227,21.0650173413637,49.3977706957327));
#33100=CARTESIAN_POINT('Ctrl Pts',(-15.5170269909309,20.9522796229575,48.0643704677906));
#33101=CARTESIAN_POINT('Ctrl Pts',(-11.914371579572,20.8098799445818,45.7040379574521));
#33102=CARTESIAN_POINT('Ctrl Pts',(-8.07256301685713,20.6742608619688,42.5653401166904));
#33103=CARTESIAN_POINT('Ctrl Pts',(-4.70319179318808,20.5745198093833,38.9896454840175));
#33104=CARTESIAN_POINT('Ctrl Pts',(-1.83741971061299,20.5040526001987,35.0435609972412));
#33105=CARTESIAN_POINT('Ctrl Pts',(0.608966176495263,20.4519664047462,30.8368346587396));
#33106=CARTESIAN_POINT('Ctrl Pts',(2.51057796417895,20.4158956934967,26.3489677971651));
#33107=CARTESIAN_POINT('Ctrl Pts',(3.83699263811829,20.3835681705302,21.6471901234823));
#33108=CARTESIAN_POINT('Ctrl Pts',(4.56579136351948,20.3523071857454,17.5012346735257));
#33109=CARTESIAN_POINT('Ctrl Pts',(4.77051650292995,20.3249607749065,14.6805961850593));
#33110=CARTESIAN_POINT('Ctrl Pts',(4.80978218635625,20.3034475984546,12.8131842367604));
#33111=CARTESIAN_POINT('Ctrl Pts',(4.81194485833614,20.2980359714688,12.3657068298895));
#33112=CARTESIAN_POINT('Ctrl Pts',(4.80691198455189,20.29241155197,11.9189933731304));
#33113=CARTESIAN_POINT('Ctrl Pts',(-18.7931495275701,20.942701117012,50.5499825156838));
#33114=CARTESIAN_POINT('Ctrl Pts',(-18.3844104556852,20.9203083949833,50.374767548075));
#33115=CARTESIAN_POINT('Ctrl Pts',(-17.9772051846334,20.898168919688,50.1922871944566));
#33116=CARTESIAN_POINT('Ctrl Pts',(-16.2467663305493,20.8048139743737,49.3824073503764));
#33117=CARTESIAN_POINT('Ctrl Pts',(-13.6930315374653,20.6706999592586,48.0142800257256));
#33118=CARTESIAN_POINT('Ctrl Pts',(-10.1643218718747,20.496623371127,45.6089923970645));
#33119=CARTESIAN_POINT('Ctrl Pts',(-6.41557697784693,20.3241023157428,42.4268731843061));
#33120=CARTESIAN_POINT('Ctrl Pts',(-3.14681387909189,20.1870685788371,38.8199146290123));
#33121=CARTESIAN_POINT('Ctrl Pts',(-0.387764824647273,20.0783595881962,
34.8560273198493));
#33122=CARTESIAN_POINT('Ctrl Pts',(1.94777122640899,19.9870599496472,30.6429562278427));
#33123=CARTESIAN_POINT('Ctrl Pts',(3.73433174589954,19.9103458023656,26.1639249023865));
#33124=CARTESIAN_POINT('Ctrl Pts',(4.9429249685331,19.8358125374395,21.4874335311705));
#33125=CARTESIAN_POINT('Ctrl Pts',(5.56948361862012,19.767331746443,17.3750052192677));
#33126=CARTESIAN_POINT('Ctrl Pts',(5.70564434247915,19.7145309927478,14.5849983059168));
#33127=CARTESIAN_POINT('Ctrl Pts',(5.69981136771872,19.6760973304852,12.7405833232543));
#33128=CARTESIAN_POINT('Ctrl Pts',(5.69118929611297,19.6666248028076,12.298763756689));
#33129=CARTESIAN_POINT('Ctrl Pts',(5.67541272468907,19.6569408091057,11.8578469720222));
#33130=CARTESIAN_POINT('Ctrl Pts',(-16.0729951996959,20.4780024533914,50.577823881251));
#33131=CARTESIAN_POINT('Ctrl Pts',(-15.6734865422844,20.4514551579611,50.3943799261068));
#33132=CARTESIAN_POINT('Ctrl Pts',(-15.2756635218504,20.4251375618498,50.2037236209258));
#33133=CARTESIAN_POINT('Ctrl Pts',(-13.585918711749,20.3138746691076,49.3591889780907));
#33134=CARTESIAN_POINT('Ctrl Pts',(-11.0979122802499,20.1526659052326,47.9411348740909));
#33135=CARTESIAN_POINT('Ctrl Pts',(-7.67711842462297,19.938389785095,45.4712448274525));
#33136=CARTESIAN_POINT('Ctrl Pts',(-4.06407758685823,19.7189203495023,42.2267652427763));
#33137=CARTESIAN_POINT('Ctrl Pts',(-0.941922279639655,19.5342279169114,
38.5749629248337));
#33138=CARTESIAN_POINT('Ctrl Pts',(1.66165202444,19.3763677050182,34.5856193142543));
#33139=CARTESIAN_POINT('Ctrl Pts',(3.83571038720547,19.2344308170631,30.3635908493067));
#33140=CARTESIAN_POINT('Ctrl Pts',(5.45465393399974,19.1049298841923,25.8974565196366));
#33141=CARTESIAN_POINT('Ctrl Pts',(6.49153137845572,18.9752993129734,21.2575392892134));
#33142=CARTESIAN_POINT('Ctrl Pts',(6.96902001911252,18.8580619466085,17.1935174826788));
#33143=CARTESIAN_POINT('Ctrl Pts',(7.00515567331294,18.7718242877839,14.4476953676603));
#33144=CARTESIAN_POINT('Ctrl Pts',(6.93350774385575,18.7111415689428,12.6364417245434));
#33145=CARTESIAN_POINT('Ctrl Pts',(6.90914089038382,18.6963263828107,12.2028004749143));
#33146=CARTESIAN_POINT('Ctrl Pts',(6.87767405528031,18.6812985797984,11.7702816402821));
#33147=CARTESIAN_POINT('Ctrl Pts',(-12.1032860351762,19.4355555088431,50.6164198137043));
#33148=CARTESIAN_POINT('Ctrl Pts',(-11.7178979337882,19.4044605226273,50.4206764214417));
#33149=CARTESIAN_POINT('Ctrl Pts',(-11.3344425025602,19.3735658358572,50.2178005709574));
#33150=CARTESIAN_POINT('Ctrl Pts',(-9.70707833240668,19.2426748194849,49.3214781077038));
#33151=CARTESIAN_POINT('Ctrl Pts',(-7.31971757114185,19.0517849995255,47.8288402064322));
#33152=CARTESIAN_POINT('Ctrl Pts',(-4.06391667596133,18.7933185397158,45.2625228787868));
#33153=CARTESIAN_POINT('Ctrl Pts',(-0.65815408706669,18.5218580841843,41.9250672284237));
#33154=CARTESIAN_POINT('Ctrl Pts',(2.24021981970534,18.2836948825759,38.2065612420059));
#33155=CARTESIAN_POINT('Ctrl Pts',(4.60650328315228,18.0697821020849,34.1795723756759));
#33156=CARTESIAN_POINT('Ctrl Pts',(6.53406799563972,17.8693333343866,29.9446179095315));
#33157=CARTESIAN_POINT('Ctrl Pts',(7.89702239493376,17.6778661310593,25.4982889661853));
#33158=CARTESIAN_POINT('Ctrl Pts',(8.6714190430009,17.4826662284719,20.9136218061456));
#33159=CARTESIAN_POINT('Ctrl Pts',(8.92083514113572,17.3068805329357,16.9224847476292));
#33160=CARTESIAN_POINT('Ctrl Pts',(8.80376329647722,17.1802068447994,14.2430779026764));
#33161=CARTESIAN_POINT('Ctrl Pts',(8.63123896138171,17.0925519552341,12.4816401372632));
#33162=CARTESIAN_POINT('Ctrl Pts',(8.58273039837833,17.0712544126695,12.0603344267302));
#33163=CARTESIAN_POINT('Ctrl Pts',(8.52719757288954,17.0497370990139,11.6405300048787));
#33164=CARTESIAN_POINT('Ctrl Pts',(-7.62272160330697,17.8320672383652,50.6581802616326));
#33165=CARTESIAN_POINT('Ctrl Pts',(-7.25398775498929,17.7976045693245,50.4481370270082));
#33166=CARTESIAN_POINT('Ctrl Pts',(-6.88750202682987,17.7633163796081,50.2310564733353));
#33167=CARTESIAN_POINT('Ctrl Pts',(-5.33391956582982,17.6178640028275,49.2745483347903));
#33168=CARTESIAN_POINT('Ctrl Pts',(-3.06553206003439,17.4049846203341,47.6952600514936));
#33169=CARTESIAN_POINT('Ctrl Pts',(-0.00463583136575324,17.1135517229592,
45.0169995840933));
#33170=CARTESIAN_POINT('Ctrl Pts',(3.15635102645389,16.8027253827761,41.5717186110543));
#33171=CARTESIAN_POINT('Ctrl Pts',(5.7904790976245,16.523022337621,37.7760221244729));
#33172=CARTESIAN_POINT('Ctrl Pts',(7.87647490362216,16.2641978724915,33.7057056652031));
#33173=CARTESIAN_POINT('Ctrl Pts',(9.51275839490381,16.0157341831644,29.4562199413809));
#33174=CARTESIAN_POINT('Ctrl Pts',(10.572992548482,15.7719994721116,25.0334778672443));
#33175=CARTESIAN_POINT('Ctrl Pts',(11.0366764891831,15.5202180684676,20.5136585803792));
#33176=CARTESIAN_POINT('Ctrl Pts',(11.0158502606114,15.2931736272884,16.6078147103202));
#33177=CARTESIAN_POINT('Ctrl Pts',(10.7170384335309,15.130708702949,14.0060109473856));
#33178=CARTESIAN_POINT('Ctrl Pts',(10.424772847932,15.0190926843839,12.3027493029688));
#33179=CARTESIAN_POINT('Ctrl Pts',(10.3476075850064,14.9920326361705,11.8959214149251));
#33180=CARTESIAN_POINT('Ctrl Pts',(10.2635094955229,14.9647422323135,11.4911075898942));
#33181=CARTESIAN_POINT('Ctrl Pts',(-3.35795326833651,15.7638142683891,50.6963817466487));
#33182=CARTESIAN_POINT('Ctrl Pts',(-3.00594729840862,15.7283726072843,50.4720971928266));
#33183=CARTESIAN_POINT('Ctrl Pts',(-2.65653363487031,15.6930928161318,50.2408753340372));
#33184=CARTESIAN_POINT('Ctrl Pts',(-1.17729495989077,15.543379415412,49.2244801690097));
#33185=CARTESIAN_POINT('Ctrl Pts',(0.971223374172476,15.3241289383934,47.55900262026));
#33186=CARTESIAN_POINT('Ctrl Pts',(3.8357234634446,15.0227233638938,44.7694897092564));
#33187=CARTESIAN_POINT('Ctrl Pts',(6.74997776965196,14.6988957424381,41.2171739295578));
#33188=CARTESIAN_POINT('Ctrl Pts',(9.11758018092376,14.4035050799014,37.3450408571422));
#33189=CARTESIAN_POINT('Ctrl Pts',(10.9206141805866,14.1252237593235,33.2320880582171));
#33190=CARTESIAN_POINT('Ctrl Pts',(12.2625916131558,13.8539516979883,28.9686983169118));
#33191=CARTESIAN_POINT('Ctrl Pts',(13.0165992412534,13.5829362127958,24.5700729333908));
#33192=CARTESIAN_POINT('Ctrl Pts',(13.1655210239449,13.2994842764397,20.115507858));
#33193=CARTESIAN_POINT('Ctrl Pts',(12.8705817285104,13.0425486753816,16.295208978186));
#33194=CARTESIAN_POINT('Ctrl Pts',(12.3871650850191,12.8585920936854,13.7711041013664));
#33195=CARTESIAN_POINT('Ctrl Pts',(11.9731744450198,12.7324540777387,12.1260554282844));
#33196=CARTESIAN_POINT('Ctrl Pts',(11.8668941925931,12.7018988467546,11.733793887101));
#33197=CARTESIAN_POINT('Ctrl Pts',(11.7537921409323,12.6711030837425,11.3441365131014));
#33198=CARTESIAN_POINT('Ctrl Pts',(0.649628458040476,13.2592937677246,50.7317627733558));
#33199=CARTESIAN_POINT('Ctrl Pts',(0.985066924078268,13.2252177231213,50.4932939999314));
#33200=CARTESIAN_POINT('Ctrl Pts',(1.31754402223974,13.191306123502,50.2479943303873));
#33201=CARTESIAN_POINT('Ctrl Pts',(2.72290890156926,13.0474600457288,49.1720182643306));
#33202=CARTESIAN_POINT('Ctrl Pts',(4.7522202374985,12.8372075593629,47.4208175921215));
#33203=CARTESIAN_POINT('Ctrl Pts',(7.42110856617907,12.5484949329477,44.5207322457509));
#33204=CARTESIAN_POINT('Ctrl Pts',(10.0892640390092,12.2377054846042,40.8621397595677));
#33205=CARTESIAN_POINT('Ctrl Pts',(12.1905795141142,11.9522310106351,36.9142683953372));
#33206=CARTESIAN_POINT('Ctrl Pts',(13.7104379500398,11.6797819251771,32.7592945131865));
#33207=CARTESIAN_POINT('Ctrl Pts',(14.7575062139052,11.4108111467242,28.4825373574617));
#33208=CARTESIAN_POINT('Ctrl Pts',(15.2041645593447,11.1374939458242,24.1084517121114));
#33209=CARTESIAN_POINT('Ctrl Pts',(15.0366365526659,10.8473681096278,19.7194278841075));
#33210=CARTESIAN_POINT('Ctrl Pts',(14.4657312097101,10.5820480444149,15.9848167741326));
#33211=CARTESIAN_POINT('Ctrl Pts',(13.7961914563873,10.3910369789073,13.5384306970429));
#33212=CARTESIAN_POINT('Ctrl Pts',(13.2593802947326,10.2599216927486,11.9515813330258));
#33213=CARTESIAN_POINT('Ctrl Pts',(13.1237579689611,10.2281653805015,11.5739532609048));
#33214=CARTESIAN_POINT('Ctrl Pts',(12.9814618015971,10.1961599190035,11.1995871689857));
#33215=CARTESIAN_POINT('Ctrl Pts',(4.42912516463123,10.420684636249,50.7652541888306));
#33216=CARTESIAN_POINT('Ctrl Pts',(4.74825780617854,10.3898269637342,50.5126392026911));
#33217=CARTESIAN_POINT('Ctrl Pts',(5.06403756009174,10.3591499865554,50.2533088244876));
#33218=CARTESIAN_POINT('Ctrl Pts',(6.39645270620807,10.2291883131935,49.1179996982607));
#33219=CARTESIAN_POINT('Ctrl Pts',(8.30791494002339,10.0401067219452,47.2814499847572));
#33220=CARTESIAN_POINT('Ctrl Pts',(10.7830309301442,9.78206378055234,44.2713285475977));
#33221=CARTESIAN_POINT('Ctrl Pts',(13.2069767395828,9.50499638561923,40.507046655879));
#33222=CARTESIAN_POINT('Ctrl Pts',(15.0435435138209,9.24981780003299,36.483964634552));
#33223=CARTESIAN_POINT('Ctrl Pts',(16.2813751655171,9.00337535985762,32.2874206634502));
#33224=CARTESIAN_POINT('Ctrl Pts',(17.0343538672163,8.75677479408939,27.9976769484779));
#33225=CARTESIAN_POINT('Ctrl Pts',(17.1740502474811,8.50116890088297,23.6484132748248));
#33226=CARTESIAN_POINT('Ctrl Pts',(16.6900004076409,8.22444592813344,19.3250984247532));
#33227=CARTESIAN_POINT('Ctrl Pts',(15.8427415672468,7.96804930448713,15.6762334080315));
#33228=CARTESIAN_POINT('Ctrl Pts',(14.9865968963869,7.78162503245108,13.3075436526941));
#33229=CARTESIAN_POINT('Ctrl Pts',(14.3265730286372,7.65323614745839,11.7788572968638));
#33230=CARTESIAN_POINT('Ctrl Pts',(14.1615675750574,7.62212996336316,11.4159103189612));
#33231=CARTESIAN_POINT('Ctrl Pts',(13.9900895826365,7.59076668565169,11.0569364769952));
#33232=CARTESIAN_POINT('Ctrl Pts',(7.89549180552655,7.18298363715391,50.7967927897824));
#33233=CARTESIAN_POINT('Ctrl Pts',(8.19878346721173,7.15763661423686,50.5300854115103));
#33234=CARTESIAN_POINT('Ctrl Pts',(8.49831389186478,7.13250342173354,50.2567869804956));
#33235=CARTESIAN_POINT('Ctrl Pts',(9.75961916607793,7.02634360727853,49.0624579541012));
#33236=CARTESIAN_POINT('Ctrl Pts',(11.5559647746267,6.87350147707393,47.1410278166122));
#33237=CARTESIAN_POINT('Ctrl Pts',(13.8411235870497,6.66841421880391,44.0215306056881));
#33238=CARTESIAN_POINT('Ctrl Pts',(16.0249513960127,6.45075222930465,40.1522690131667));
#33239=CARTESIAN_POINT('Ctrl Pts',(17.6003804394465,6.25122984378583,36.0545969342759));
#33240=CARTESIAN_POINT('Ctrl Pts',(18.5592768296093,6.05595707526583,31.8169952215559));
#33241=CARTESIAN_POINT('Ctrl Pts',(19.0208253379016,5.8568061689083,27.5146808861226));
#33242=CARTESIAN_POINT('Ctrl Pts',(18.8556599138234,5.64398234710963,23.1905225310631));
#33243=CARTESIAN_POINT('Ctrl Pts',(18.0566069174411,5.40587468584602,18.9330502545293));
#33244=CARTESIAN_POINT('Ctrl Pts',(16.9338900015705,5.18017895256177,15.3699358641023));
#33245=CARTESIAN_POINT('Ctrl Pts',(15.8914626446178,5.01301666232781,13.0788676150056));
#33246=CARTESIAN_POINT('Ctrl Pts',(15.1083470249008,4.89707445701614,11.6082681357848));
#33247=CARTESIAN_POINT('Ctrl Pts',(14.9140516856407,4.86894780999335,11.2600237011743));
#33248=CARTESIAN_POINT('Ctrl Pts',(14.7135487892971,4.84055053954568,10.9165003544731));
#33249=CARTESIAN_POINT('Ctrl Pts',(11.0060924800857,3.57357815210241,50.8268930609901));
#33250=CARTESIAN_POINT('Ctrl Pts',(11.2942348360949,3.55599962931061,50.5461528505987));
#33251=CARTESIAN_POINT('Ctrl Pts',(11.5781977781179,3.53868515668548,50.2589525717582));
#33252=CARTESIAN_POINT('Ctrl Pts',(12.7712619273494,3.46609807861293,49.0059215208389));
#33253=CARTESIAN_POINT('Ctrl Pts',(14.4567798870219,3.36435917107101,47.0000807098697));
#33254=CARTESIAN_POINT('Ctrl Pts',(16.5580799000384,3.23426720235262,43.7718526676594));
#33255=CARTESIAN_POINT('Ctrl Pts',(18.5084918938618,3.10147907156715,39.7982847372331));
#33256=CARTESIAN_POINT('Ctrl Pts',(19.8289470704012,2.98285053627008,35.6265858547269));
#33257=CARTESIAN_POINT('Ctrl Pts',(20.5145093436472,2.86388130857434,31.3483637201532));
#33258=CARTESIAN_POINT('Ctrl Pts',(20.6897703805126,2.73730530568202,27.0338075077601));
#33259=CARTESIAN_POINT('Ctrl Pts',(20.2243046828408,2.59247375589619,22.7349380039858));
#33260=CARTESIAN_POINT('Ctrl Pts',(19.1142246129334,2.41842603756845,18.5433338285095));
#33261=CARTESIAN_POINT('Ctrl Pts',(17.71905778023,2.24547053120763,15.0658785351744));
#33262=CARTESIAN_POINT('Ctrl Pts',(16.492089181663,2.11246131963295,12.8522922345518));
#33263=CARTESIAN_POINT('Ctrl Pts',(15.5869422351719,2.01884144332686,11.4396612518973));
#33264=CARTESIAN_POINT('Ctrl Pts',(15.3636796831515,1.99605339732081,11.1061079698993));
#33265=CARTESIAN_POINT('Ctrl Pts',(15.1345413251225,1.9729679754383,10.7780380956973));
#33266=CARTESIAN_POINT('Ctrl Pts',(13.4086040565199,0.237308438758995,50.8518932795148));
#33267=CARTESIAN_POINT('Ctrl Pts',(13.6843431150251,0.227921876287717,50.5591653280353));
#33268=CARTESIAN_POINT('Ctrl Pts',(13.955539055312,0.218854274805993,50.2600946828327));
#33269=CARTESIAN_POINT('Ctrl Pts',(15.092550531276,0.181679983795775,48.9569680233745));
#33270=CARTESIAN_POINT('Ctrl Pts',(16.6867297894324,0.133848323063104,46.8790983035039));
#33271=CARTESIAN_POINT('Ctrl Pts',(18.6356692131024,0.0830496793456984,
43.558108432264));
#33272=CARTESIAN_POINT('Ctrl Pts',(20.391809639507,0.0403924264632703,39.4955813035581));
#33273=CARTESIAN_POINT('Ctrl Pts',(21.499121492597,0.00837005963384143,
35.2607922709484));
#33274=CARTESIAN_POINT('Ctrl Pts',(21.9553996260992,-0.0279539839125438,
30.9480199544426));
#33275=CARTESIAN_POINT('Ctrl Pts',(21.8899491514933,-0.0750512999789021,
26.6231583667432));
#33276=CARTESIAN_POINT('Ctrl Pts',(21.1713548702409,-0.14423024726241,22.3460478681646));
#33277=CARTESIAN_POINT('Ctrl Pts',(19.7985513468811,-0.245792879606331,
18.210873465606));
#33278=CARTESIAN_POINT('Ctrl Pts',(18.172904950709,-0.358291148292244,14.8067369437337));
#33279=CARTESIAN_POINT('Ctrl Pts',(16.7896161629616,-0.451704594358635,
12.659441105225));
#33280=CARTESIAN_POINT('Ctrl Pts',(15.7810380374713,-0.519340602547392,
11.2963988201152));
#33281=CARTESIAN_POINT('Ctrl Pts',(15.5332807033662,-0.535923052101836,
10.9754131301141));
#33282=CARTESIAN_POINT('Ctrl Pts',(15.2799843900674,-0.552841667182328,
10.6605612070475));
#33283=CARTESIAN_POINT('Ctrl Pts',(14.8211913517824,-2.14030259993981,50.8681119118098));
#33284=CARTESIAN_POINT('Ctrl Pts',(15.0891137342418,-2.14321532053782,50.5674285935912));
#33285=CARTESIAN_POINT('Ctrl Pts',(15.3522519677804,-2.14576465810466,50.2604798846934));
#33286=CARTESIAN_POINT('Ctrl Pts',(16.4538380030325,-2.15494826818845,48.9241050232901));
#33287=CARTESIAN_POINT('Ctrl Pts',(17.9900417596044,-2.16016260296573,46.7984325485291));
#33288=CARTESIAN_POINT('Ctrl Pts',(19.841600565389,-2.1481556077715,43.4158887130568));
#33289=CARTESIAN_POINT('Ctrl Pts',(21.4729001795181,-2.11918777525101,39.2943434845245));
#33290=CARTESIAN_POINT('Ctrl Pts',(22.4425122487173,-2.08197924289826,35.0177196733706));
#33291=CARTESIAN_POINT('Ctrl Pts',(22.7500500882429,-2.05170003121316,30.6820714739305));
#33292=CARTESIAN_POINT('Ctrl Pts',(22.5280186102684,-2.03426137368081,26.3504407431274));
#33293=CARTESIAN_POINT('Ctrl Pts',(21.6442903605272,-2.04135770257883,22.0878641606114));
#33294=CARTESIAN_POINT('Ctrl Pts',(20.0996909490575,-2.08278583441843,17.9902613908005));
#33295=CARTESIAN_POINT('Ctrl Pts',(18.3230901845701,-2.14471303148954,14.6349096946119));
#33296=CARTESIAN_POINT('Ctrl Pts',(16.8372754744228,-2.20477046252904,12.5317089640345));
#33297=CARTESIAN_POINT('Ctrl Pts',(15.7608189202074,-2.25046208753918,11.2016493161336));
#33298=CARTESIAN_POINT('Ctrl Pts',(15.4970132544121,-2.26180965939547,10.8890156234971));
#33299=CARTESIAN_POINT('Ctrl Pts',(15.2279154659668,-2.27353152926925,10.582940513715));
#33300=CARTESIAN_POINT('Ctrl Pts',(15.7277767926436,-3.83428286431684,50.8791923579944));
#33301=CARTESIAN_POINT('Ctrl Pts',(15.9904775111148,-3.83237339034492,50.5730212587592));
#33302=CARTESIAN_POINT('Ctrl Pts',(16.2482277522975,-3.83006698099443,50.2606381905767));
#33303=CARTESIAN_POINT('Ctrl Pts',(17.3261040612264,-3.81839846831683,48.9013292866715));
#33304=CARTESIAN_POINT('Ctrl Pts',(18.8234014267205,-3.79185933798401,46.7426835888032));
#33305=CARTESIAN_POINT('Ctrl Pts',(20.6093307672563,-3.73301479320489,43.3176825681743));
#33306=CARTESIAN_POINT('Ctrl Pts',(22.1562183974292,-3.65055513724086,39.1554316071207));
#33307=CARTESIAN_POINT('Ctrl Pts',(23.0324273075003,-3.56151400652134,34.8499580812955));
#33308=CARTESIAN_POINT('Ctrl Pts',(23.2388288624445,-3.48120332570528,30.4985424034584));
#33309=CARTESIAN_POINT('Ctrl Pts',(22.9101616831314,-3.41513875248544,26.1622590588885));
#33310=CARTESIAN_POINT('Ctrl Pts',(21.9137885476468,-3.37526128513496,21.9097314946167));
#33311=CARTESIAN_POINT('Ctrl Pts',(20.2518478400219,-3.37099617994084,17.8380781703545));
#33312=CARTESIAN_POINT('Ctrl Pts',(18.3720514471088,-3.39437469848804,14.516413522755));
#33313=CARTESIAN_POINT('Ctrl Pts',(16.8160965878723,-3.42893690611626,12.443658949834));
#33314=CARTESIAN_POINT('Ctrl Pts',(15.6931888427596,-3.45783930783476,11.1363723028377));
#33315=CARTESIAN_POINT('Ctrl Pts',(15.4184128726594,-3.46518513130081,10.8295005505935));
#33316=CARTESIAN_POINT('Ctrl Pts',(15.1385252299473,-3.47293757911652,10.5294756446789));
#33317=CARTESIAN_POINT('Ctrl Pts',(15.9701665800735,-4.30636894546118,50.8822308776832));
#33318=CARTESIAN_POINT('Ctrl Pts',(16.2314548017925,-4.3031084050989,50.5745495731437));
#33319=CARTESIAN_POINT('Ctrl Pts',(16.4877466093682,-4.29944065268701,50.260670552203));
#33320=CARTESIAN_POINT('Ctrl Pts',(17.5592011847449,-4.28192251284736,48.8950465059731));
#33321=CARTESIAN_POINT('Ctrl Pts',(19.0459352980637,-4.24645759656194,46.7273192303219));
#33322=CARTESIAN_POINT('Ctrl Pts',(20.8139790917651,-4.17439213330946,43.290622721956));
#33323=CARTESIAN_POINT('Ctrl Pts',(22.3377993873479,-4.07676875425951,39.1171604186841));
#33324=CARTESIAN_POINT('Ctrl Pts',(23.1884224645965,-3.97294922980807,34.8037494417951));
#33325=CARTESIAN_POINT('Ctrl Pts',(23.3670805064487,-3.87828739688684,30.4480108044923));
#33326=CARTESIAN_POINT('Ctrl Pts',(23.0091488885558,-3.79820251809058,26.1104754031575));
#33327=CARTESIAN_POINT('Ctrl Pts',(21.9818628449813,-3.74469501429227,21.8607506502009));
#33328=CARTESIAN_POINT('Ctrl Pts',(20.2877455250282,-3.72710099262819,17.7962731039455));
#33329=CARTESIAN_POINT('Ctrl Pts',(18.379688708248,-3.7392015362719,14.4838944016608));
#33330=CARTESIAN_POINT('Ctrl Pts',(16.8045486295666,-3.76629674044718,12.4195139572451));
#33331=CARTESIAN_POINT('Ctrl Pts',(15.6689453809918,-3.79028538091932,11.1184838099602));
#33332=CARTESIAN_POINT('Ctrl Pts',(15.3911733460635,-3.79646095010219,10.8131933790853));
#33333=CARTESIAN_POINT('Ctrl Pts',(15.1083410178804,-3.80305340259771,10.5148273212522));
#33334=CARTESIAN_POINT('Ctrl Pts',(16.2040281833702,-4.78145508078572,50.8852370446122));
#33335=CARTESIAN_POINT('Ctrl Pts',(16.4639362979632,-4.77682808742727,50.5760559448111));
#33336=CARTESIAN_POINT('Ctrl Pts',(16.7188024266086,-4.7717826224726,50.260690536201));
#33337=CARTESIAN_POINT('Ctrl Pts',(17.7839765354645,-4.74834091216943,48.8887884576835));
#33338=CARTESIAN_POINT('Ctrl Pts',(19.2603541657225,-4.70381966688121,46.7120309167521));
#33339=CARTESIAN_POINT('Ctrl Pts',(21.0107955623606,-4.61828583278682,43.2637031873351));
#33340=CARTESIAN_POINT('Ctrl Pts',(22.5118507531063,-4.50515190400754,39.0790928379428));
#33341=CARTESIAN_POINT('Ctrl Pts',(23.3371620822167,-4.38613315046716,34.7577977729984));
#33342=CARTESIAN_POINT('Ctrl Pts',(23.488334854988,-4.27662792828432,30.3977805929722));
#33343=CARTESIAN_POINT('Ctrl Pts',(23.1013992673138,-4.18197237106197,26.0590299164957));
#33344=CARTESIAN_POINT('Ctrl Pts',(22.0434765995787,-4.11421750462538,21.8121276651408));
#33345=CARTESIAN_POINT('Ctrl Pts',(20.3174958444881,-4.08262421860679,17.7548145479695));
#33346=CARTESIAN_POINT('Ctrl Pts',(18.3814912904369,-4.0828488851085,14.4516774578153));
#33347=CARTESIAN_POINT('Ctrl Pts',(16.7874012762348,-4.10207414795096,12.3956126071312));
#33348=CARTESIAN_POINT('Ctrl Pts',(15.639268392688,-4.12088738197538,11.1007880383459));
#33349=CARTESIAN_POINT('Ctrl Pts',(15.3585405257443,-4.12583098108427,10.7970646604656));
#33350=CARTESIAN_POINT('Ctrl Pts',(15.0728040607247,-4.13120272145022,10.5003411970122));
#33351=CARTESIAN_POINT('Ctrl Pts',(-11.2641171037461,20.7105311502992,45.5014889049172));
#33352=CARTESIAN_POINT('Ctrl Pts',(-8.19359489044161,19.964194825681,46.2616123376652));
#33353=CARTESIAN_POINT('Ctrl Pts',(-5.14011995665627,18.7336174305176,46.6827377201639));
#33354=CARTESIAN_POINT('Ctrl Pts',(1.02851041262146,15.6437709209759,46.9777867249755));
#33355=CARTESIAN_POINT('Ctrl Pts',(4.2178450202458,13.6706054870974,46.7792896653727));
#33356=CARTESIAN_POINT('Ctrl Pts',(9.98319411871419,9.45712578824497,45.8889713600162));
#33357=CARTESIAN_POINT('Ctrl Pts',(12.6385843053104,7.18268858965248,45.2073292047804));
#33358=CARTESIAN_POINT('Ctrl Pts',(17.2824959903431,2.26699035497259,43.6397205033547));
#33359=CARTESIAN_POINT('Ctrl Pts',(19.2859044761697,-0.365223927781814,
42.7616321300472));
#33360=CARTESIAN_POINT('Ctrl Pts',(20.8964136033761,-3.27137043593021,41.9595779228243));
#33361=CARTESIAN_POINT('Ctrl Pts',(-53.0706963107889,21.2883239772394,14.476633177513));
#33362=CARTESIAN_POINT('Ctrl Pts',(-52.6797132558222,21.2711623310641,14.7001712927468));
#33363=CARTESIAN_POINT('Ctrl Pts',(-52.2838656141311,21.2542807820542,14.9180639701196));
#33364=CARTESIAN_POINT('Ctrl Pts',(-50.5741822007401,21.1834525291307,15.8231443989111));
#33365=CARTESIAN_POINT('Ctrl Pts',(-47.9110575975486,21.0834264338425,17.0549709528455));
#33366=CARTESIAN_POINT('Ctrl Pts',(-43.8135759591412,20.9598507183575,18.4474868853566));
#33367=CARTESIAN_POINT('Ctrl Pts',(-38.9511846919585,20.8461335954997,19.5494115754497));
#33368=CARTESIAN_POINT('Ctrl Pts',(-34.0338251352838,20.7684839093916,20.0085467195199));
#33369=CARTESIAN_POINT('Ctrl Pts',(-29.1329513291906,20.7206230093664,19.8409647486116));
#33370=CARTESIAN_POINT('Ctrl Pts',(-24.2834341719871,20.6916936542703,19.180752348512));
#33371=CARTESIAN_POINT('Ctrl Pts',(-19.545805391625,20.6796111419738,17.9158146216833));
#33372=CARTESIAN_POINT('Ctrl Pts',(-14.9915461588884,20.6722203558656,16.0632020463146));
#33373=CARTESIAN_POINT('Ctrl Pts',(-11.2462565116349,20.6630225594897,14.0802672689721));
#33374=CARTESIAN_POINT('Ctrl Pts',(-8.87666243655348,20.6508204531822,12.5004226092667));
#33375=CARTESIAN_POINT('Ctrl Pts',(-7.36681121688492,20.6394053700742,11.3781216551321));
#33376=CARTESIAN_POINT('Ctrl Pts',(-7.00948282225308,20.6364191357732,11.1034672733586));
#33377=CARTESIAN_POINT('Ctrl Pts',(-6.65719863322378,20.6332209087108,10.8235999116748));
#33378=CARTESIAN_POINT('Ctrl Pts',(-52.7423035144133,21.2398788304839,14.8976565953797));
#33379=CARTESIAN_POINT('Ctrl Pts',(-52.3511594092213,21.2217224127637,15.1188499155687));
#33380=CARTESIAN_POINT('Ctrl Pts',(-51.9551751700423,21.2038412173392,15.3343835927472));
#33381=CARTESIAN_POINT('Ctrl Pts',(-50.2450148726635,21.1287309618461,16.229336348993));
#33382=CARTESIAN_POINT('Ctrl Pts',(-47.5820448257753,21.0222253289507,17.4455115403598));
#33383=CARTESIAN_POINT('Ctrl Pts',(-43.4874625788319,20.8890564489947,18.8143754535216));
#33384=CARTESIAN_POINT('Ctrl Pts',(-38.6315801910077,20.7641817659416,19.8887967941821));
#33385=CARTESIAN_POINT('Ctrl Pts',(-33.7246510566663,20.6752847595175,20.3209113143506));
#33386=CARTESIAN_POINT('Ctrl Pts',(-28.8381509343392,20.6159219251614,20.127340043755));
#33387=CARTESIAN_POINT('Ctrl Pts',(-24.0061641643323,20.5752144761384,19.4422615502697));
#33388=CARTESIAN_POINT('Ctrl Pts',(-19.2900265578325,20.5509334123338,18.1542244143579));
#33389=CARTESIAN_POINT('Ctrl Pts',(-14.7612427448985,20.5308579865904,16.2808214371791));
#33390=CARTESIAN_POINT('Ctrl Pts',(-11.0405313054518,20.510426256151,14.2819051282588));
#33391=CARTESIAN_POINT('Ctrl Pts',(-8.68917344007867,20.4905046142392,12.6927881463597));
#33392=CARTESIAN_POINT('Ctrl Pts',(-7.19193426214825,20.4739374093561,11.5648960507006));
#33393=CARTESIAN_POINT('Ctrl Pts',(-6.8376516744731,20.469713411733,11.2889307083142));
#33394=CARTESIAN_POINT('Ctrl Pts',(-6.48843209010061,20.4652767483487,11.0077838216047));
#33395=CARTESIAN_POINT('Ctrl Pts',(-52.413730952202,21.1822016013635,15.3188148573173));
#33396=CARTESIAN_POINT('Ctrl Pts',(-52.0224315719836,21.1630886105529,15.5376446728873));
#33397=CARTESIAN_POINT('Ctrl Pts',(-51.6263169843739,21.1442460408093,15.7508002323129));
#33398=CARTESIAN_POINT('Ctrl Pts',(-49.9157086639418,21.0650173413637,16.6355420002449));
#33399=CARTESIAN_POINT('Ctrl Pts',(-47.2529400861698,20.9522796229575,17.8359402657105));
#33400=CARTESIAN_POINT('Ctrl Pts',(-43.1613389119008,20.8098799445818,19.180966437603));
#33401=CARTESIAN_POINT('Ctrl Pts',(-38.3120776664927,20.6742608619688,20.2276672267179));
#33402=CARTESIAN_POINT('Ctrl Pts',(-33.4157184343431,20.5745198093833,20.6325385874716));
#33403=CARTESIAN_POINT('Ctrl Pts',(-28.5437656821657,20.5040526001987,20.4127459884288));
#33404=CARTESIAN_POINT('Ctrl Pts',(-23.7295179405745,20.4519664047462,19.7025565219692));
#33405=CARTESIAN_POINT('Ctrl Pts',(-19.0351267823555,20.4158956934967,18.3911572647212));
#33406=CARTESIAN_POINT('Ctrl Pts',(-14.5321229512679,20.3835681705302,16.4966795854662));
#33407=CARTESIAN_POINT('Ctrl Pts',(-10.8362858826867,20.3523071857454,14.4815164313589));
#33408=CARTESIAN_POINT('Ctrl Pts',(-8.50337787513608,20.3249607749065,12.8829376583136));
#33409=CARTESIAN_POINT('Ctrl Pts',(-7.01889467003979,20.3034475984546,11.7493245001634));
#33410=CARTESIAN_POINT('Ctrl Pts',(-6.66769434173069,20.2980359714688,11.4720177454573));
#33411=CARTESIAN_POINT('Ctrl Pts',(-6.32157764307285,20.29241155197,11.1895616016432));
#33412=CARTESIAN_POINT('Ctrl Pts',(-51.2388988296486,20.942701117012,16.8243182893816));
#33413=CARTESIAN_POINT('Ctrl Pts',(-50.8470656088309,20.9203083949833,17.0346386184588));
#33414=CARTESIAN_POINT('Ctrl Pts',(-50.4505083896763,20.898168919688,17.2392298796734));
#33415=CARTESIAN_POINT('Ctrl Pts',(-48.7384078522966,20.8048139743737,18.0871896307673));
#33416=CARTESIAN_POINT('Ctrl Pts',(-46.0765352377201,20.6706999592586,19.2307664553104));
#33417=CARTESIAN_POINT('Ctrl Pts',(-41.995891155026,20.496623371127,20.4899504573511));
#33418=CARTESIAN_POINT('Ctrl Pts',(-37.1707059623287,20.3241023157428,21.4368183577897));
#33419=CARTESIAN_POINT('Ctrl Pts',(-32.3126317510767,20.1870685788371,21.7435383821734));
#33420=CARTESIAN_POINT('Ctrl Pts',(-27.4933009115434,20.0783595881962,21.4292064816315));
#33421=CARTESIAN_POINT('Ctrl Pts',(-22.7432063842296,19.9870599496472,20.6283952344143));
#33422=CARTESIAN_POINT('Ctrl Pts',(-18.1274564187216,19.9103458023656,19.2325541402588));
#33423=CARTESIAN_POINT('Ctrl Pts',(-13.7176826883073,19.8358125374395,17.2617256927776));
#33424=CARTESIAN_POINT('Ctrl Pts',(-10.1118038360732,19.767331746443,15.1875318576818));
#33425=CARTESIAN_POINT('Ctrl Pts',(-7.84559377217224,19.7145309927478,13.5544457406808));
#33426=CARTESIAN_POINT('Ctrl Pts',(-6.40720887226862,19.6760973304852,12.3999114052912));
#33427=CARTESIAN_POINT('Ctrl Pts',(-6.06715619927451,19.6666248028076,12.1177004042506));
#33428=CARTESIAN_POINT('Ctrl Pts',(-5.73227010726454,19.6569408091057,11.8304586653179));
#33429=CARTESIAN_POINT('Ctrl Pts',(-49.5646776028525,20.4780024533914,18.9683793875862));
#33430=CARTESIAN_POINT('Ctrl Pts',(-49.172165769802,20.4514551579611,19.166352398224));
#33431=CARTESIAN_POINT('Ctrl Pts',(-48.7750660718952,20.4251375618498,19.3585106981095));
#33432=CARTESIAN_POINT('Ctrl Pts',(-47.0612436432498,20.3138746691076,20.1530476508596));
#33433=CARTESIAN_POINT('Ctrl Pts',(-44.4013176639012,20.1526659052326,21.2141071352607));
#33434=CARTESIAN_POINT('Ctrl Pts',(-40.3374497839604,19.938389785095,22.3486402108316));
#33435=CARTESIAN_POINT('Ctrl Pts',(-35.5481193843904,19.7189203495023,23.1505293518543));
#33436=CARTESIAN_POINT('Ctrl Pts',(-30.7463933706032,19.5342279169114,23.3146671605512));
#33437=CARTESIAN_POINT('Ctrl Pts',(-26.0040969144944,19.3763677050182,22.8629084611189));
#33438=CARTESIAN_POINT('Ctrl Pts',(-21.3476789228923,19.2344308170631,21.9302640427997));
#33439=CARTESIAN_POINT('Ctrl Pts',(-16.8465197078137,19.1049298841923,20.4114158677415));
#33440=CARTESIAN_POINT('Ctrl Pts',(-12.5724038286273,18.9752993129734,18.3291382226407));
#33441=CARTESIAN_POINT('Ctrl Pts',(-9.09731433688908,18.8580619466085,16.1685777235212));
#33442=CARTESIAN_POINT('Ctrl Pts',(-6.92801395023321,18.7718242877839,14.4848376291825));
#33443=CARTESIAN_POINT('Ctrl Pts',(-5.5565905826503,18.7111415689428,13.2995228472163));
#33444=CARTESIAN_POINT('Ctrl Pts',(-5.23274868623665,18.6963263828107,13.0101011772342));
#33445=CARTESIAN_POINT('Ctrl Pts',(-4.91421109534465,18.6812985797984,12.7158283323917));
#33446=CARTESIAN_POINT('Ctrl Pts',(-47.1197799375165,19.4355555088431,22.0960871589275));
#33447=CARTESIAN_POINT('Ctrl Pts',(-46.7264560399874,19.4044605226273,22.2753517007042));
#33448=CARTESIAN_POINT('Ctrl Pts',(-46.3287607622083,19.3735658358572,22.4486582051412));
#33449=CARTESIAN_POINT('Ctrl Pts',(-44.6133426779924,19.2426748194849,23.1621348317923));
#33450=CARTESIAN_POINT('Ctrl Pts',(-41.9578562868468,19.0517849995255,24.0980041256472));
#33451=CARTESIAN_POINT('Ctrl Pts',(-37.9214699510629,18.7933185397158,25.0434190840267));
#33452=CARTESIAN_POINT('Ctrl Pts',(-33.1886838105404,18.5218580841843,25.6252819356792));
#33453=CARTESIAN_POINT('Ctrl Pts',(-28.4743321897673,18.2836948825759,25.5728713432753));
#33454=CARTESIAN_POINT('Ctrl Pts',(-23.8505519067561,18.0697821020849,24.9121197610862));
#33455=CARTESIAN_POINT('Ctrl Pts',(-19.3377142376472,17.8693333343866,23.7786996168262));
#33456=CARTESIAN_POINT('Ctrl Pts',(-15.011646119972,17.6778661310593,22.0720595234769));
#33457=CARTESIAN_POINT('Ctrl Pts',(-10.9443805849522,17.4826662284719,19.8190139836521));
#33458=CARTESIAN_POINT('Ctrl Pts',(-7.66847558815272,17.3068805329357,17.5255820876028));
#33459=CARTESIAN_POINT('Ctrl Pts',(-5.6466240636577,17.1802068447994,15.7634687908796));
#33460=CARTESIAN_POINT('Ctrl Pts',(-4.377043727754,17.0925519552341,14.5303453508661));
#33461=CARTESIAN_POINT('Ctrl Pts',(-4.07789825385118,17.0712544126695,14.2297400151586));
#33462=CARTESIAN_POINT('Ctrl Pts',(-3.78430609072903,17.0497370990139,13.9245789280815));
#33463=CARTESIAN_POINT('Ctrl Pts',(-44.3588433405874,17.8320672383652,25.6251707043937));
#33464=CARTESIAN_POINT('Ctrl Pts',(-43.9647231330525,17.7976045693245,25.7824986209223));
#33465=CARTESIAN_POINT('Ctrl Pts',(-43.5665026079252,17.7633163796081,25.9336811896756));
#33466=CARTESIAN_POINT('Ctrl Pts',(-41.8500316111937,17.6178640028275,26.551947798518));
#33467=CARTESIAN_POINT('Ctrl Pts',(-39.2009778348922,17.4049846203341,27.3407744261555));
#33468=CARTESIAN_POINT('Ctrl Pts',(-35.1985919001064,17.1135517229592,28.0640113741508));
#33469=CARTESIAN_POINT('Ctrl Pts',(-30.5341196997764,16.8027253827761,28.3872728640342));
#33470=CARTESIAN_POINT('Ctrl Pts',(-25.9241726995091,16.523022337621,28.0801390685936));
#33471=CARTESIAN_POINT('Ctrl Pts',(-21.4412740362845,16.2641978724915,27.1732354593264));
#33472=CARTESIAN_POINT('Ctrl Pts',(-17.0986862433379,16.0157341831644,25.8030223951057));
#33473=CARTESIAN_POINT('Ctrl Pts',(-12.9798020686036,15.7719994721116,23.8744122556853));
#33474=CARTESIAN_POINT('Ctrl Pts',(-9.1569628467535,15.5202180684676,21.4188737268354));
#33475=CARTESIAN_POINT('Ctrl Pts',(-6.11623608466224,15.2931736272884,18.9673373050427));
#33476=CARTESIAN_POINT('Ctrl Pts',(-4.26837011845563,15.130708702949,17.11151869867));
#33477=CARTESIAN_POINT('Ctrl Pts',(-3.11893115402554,15.0190926843839,15.8210499974158));
#33478=CARTESIAN_POINT('Ctrl Pts',(-2.84897205769882,14.9920326361705,15.5070667262007));
#33479=CARTESIAN_POINT('Ctrl Pts',(-2.58491016590009,14.9647422323135,15.1889189006689));
#33480=CARTESIAN_POINT('Ctrl Pts',(-41.7296709001059,15.7638142683891,28.9833190904297));
#33481=CARTESIAN_POINT('Ctrl Pts',(-41.3348460424531,15.7283726072843,29.1186893077136));
#33482=CARTESIAN_POINT('Ctrl Pts',(-40.9362136579705,15.6930928161318,29.2477074393503));
#33483=CARTESIAN_POINT('Ctrl Pts',(-39.2192736909589,15.543379415412,29.7705107854804));
#33484=CARTESIAN_POINT('Ctrl Pts',(-36.5775716396078,15.3241289383934,30.4118817928407));
#33485=CARTESIAN_POINT('Ctrl Pts',(-32.6106560319495,15.0227233638938,30.9122052920021));
#33486=CARTESIAN_POINT('Ctrl Pts',(-28.01633587977,14.6988957424381,30.9758283948891));
#33487=CARTESIAN_POINT('Ctrl Pts',(-23.5128043811657,14.4035050799014,30.4126590158976));
#33488=CARTESIAN_POINT('Ctrl Pts',(-19.1729950858667,14.1252237593235,29.2579436351381));
#33489=CARTESIAN_POINT('Ctrl Pts',(-15.0030335205516,13.8539516979883,27.6489638156294));
#33490=CARTESIAN_POINT('Ctrl Pts',(-11.0939336494892,13.5829362127958,25.4959726484748));
#33491=CARTESIAN_POINT('Ctrl Pts',(-7.51836322006334,13.2994842764397,22.8350284903861));
#33492=CARTESIAN_POINT('Ctrl Pts',(-4.71542492625827,13.0425486753816,20.2225182721821));
#33493=CARTESIAN_POINT('Ctrl Pts',(-3.04340561577518,12.8585920936854,18.2708142716326));
#33494=CARTESIAN_POINT('Ctrl Pts',(-2.01537371507192,12.7324540777387,16.9214722846062));
#33495=CARTESIAN_POINT('Ctrl Pts',(-1.77495594634031,12.7018988467546,16.5938079667051));
#33496=CARTESIAN_POINT('Ctrl Pts',(-1.54082751975146,12.6711030837425,16.2624338230772));
#33497=CARTESIAN_POINT('Ctrl Pts',(-39.2586465641561,13.2592937677246,32.138632362006));
#33498=CARTESIAN_POINT('Ctrl Pts',(-38.8630617067816,13.2252177231213,32.2522058668933));
#33499=CARTESIAN_POINT('Ctrl Pts',(-38.4639826224378,13.191306123502,32.3592050870755));
#33500=CARTESIAN_POINT('Ctrl Pts',(-36.7465199894602,13.0474600457288,32.7871034898597));
#33501=CARTESIAN_POINT('Ctrl Pts',(-34.1121212490597,12.8372075593629,33.281827219888));
#33502=CARTESIAN_POINT('Ctrl Pts',(-30.1807185681909,12.5484949329477,33.5602745004599));
#33503=CARTESIAN_POINT('Ctrl Pts',(-25.6567480538887,12.2377054846042,33.3652273449456));
#33504=CARTESIAN_POINT('Ctrl Pts',(-21.2600291633834,11.9522310106351,32.5466444033322));
#33505=CARTESIAN_POINT('Ctrl Pts',(-17.063923538417,11.6797819251771,31.1443337349231));
#33506=CARTESIAN_POINT('Ctrl Pts',(-13.0673837668308,11.4108111467242,29.2964501962854));
#33507=CARTESIAN_POINT('Ctrl Pts',(-9.36909897898788,11.1374939458242,26.9184639603245));
#33508=CARTESIAN_POINT('Ctrl Pts',(-6.04207397664205,10.8473681096278,24.0509736936325));
#33509=CARTESIAN_POINT('Ctrl Pts',(-3.4781910952484,10.5820480444149,21.2761299820227));
#33510=CARTESIAN_POINT('Ctrl Pts',(-1.98298065004395,10.3910369789073,19.2273659536365));
#33511=CARTESIAN_POINT('Ctrl Pts',(-1.0770281441367,10.2599216927486,17.818285691764));
#33512=CARTESIAN_POINT('Ctrl Pts',(-0.866345765711677,10.2281653805015,
17.4768046358873));
#33513=CARTESIAN_POINT('Ctrl Pts',(-0.662374778275869,10.1961599190035,
17.1321395719343));
#33514=CARTESIAN_POINT('Ctrl Pts',(-36.9283535544487,10.420684636249,35.1144434311013));
#33515=CARTESIAN_POINT('Ctrl Pts',(-36.5318752578966,10.3898269637342,35.2064485096914));
#33516=CARTESIAN_POINT('Ctrl Pts',(-36.1322371476585,10.3591499865554,35.2916452167048));
#33517=CARTESIAN_POINT('Ctrl Pts',(-34.4138694749954,10.2291883131935,35.6255156634962));
#33518=CARTESIAN_POINT('Ctrl Pts',(-31.7862198804387,10.0401067219452,35.9748869984656));
#33519=CARTESIAN_POINT('Ctrl Pts',(-27.8896025965576,9.78206378055234,36.0332305838768));
#33520=CARTESIAN_POINT('Ctrl Pts',(-23.4352630122845,9.50499638561923,35.5813563586842));
#33521=CARTESIAN_POINT('Ctrl Pts',(-19.1448101772899,9.24981780003299,34.5088914700998));
#33522=CARTESIAN_POINT('Ctrl Pts',(-15.0920445718706,9.00337535985762,32.8601648563575));
#33523=CARTESIAN_POINT('Ctrl Pts',(-11.2687133422595,8.75677479408939,30.774255852101));
#33524=CARTESIAN_POINT('Ctrl Pts',(-7.78122280819138,8.50116890088297,28.1717533340615));
#33525=CARTESIAN_POINT('Ctrl Pts',(-4.70291928851549,8.22444592813344,25.0977652109468));
#33526=CARTESIAN_POINT('Ctrl Pts',(-2.37837898968668,7.96804930448713,22.1603214494423));
#33527=CARTESIAN_POINT('Ctrl Pts',(-1.06026023796119,7.78162503245108,20.0141066859967));
#33528=CARTESIAN_POINT('Ctrl Pts',(-0.276603268679021,7.65323614745839,
18.5449588939088));
#33529=CARTESIAN_POINT('Ctrl Pts',(-0.0957191124462417,7.62212996336316,
18.1896586961835));
#33530=CARTESIAN_POINT('Ctrl Pts',(0.0780231590676284,7.59076668565169,
17.8317752735585));
#33531=CARTESIAN_POINT('Ctrl Pts',(-34.7917671754843,7.18298363715391,37.8442219967885));
#33532=CARTESIAN_POINT('Ctrl Pts',(-34.3941476924951,7.15763661423686,37.9150556358309));
#33533=CARTESIAN_POINT('Ctrl Pts',(-33.9937202099012,7.13250342173354,37.97883916718));
#33534=CARTESIAN_POINT('Ctrl Pts',(-32.2735452011381,7.02634360727853,38.2203153715421));
#33535=CARTESIAN_POINT('Ctrl Pts',(-29.6513074607424,6.87350147707393,38.4267628259902));
#33536=CARTESIAN_POINT('Ctrl Pts',(-25.7876131165973,6.66841421880391,38.2683972300439));
#33537=CARTESIAN_POINT('Ctrl Pts',(-21.4009082217558,6.45075222930465,37.5633374197196));
#33538=CARTESIAN_POINT('Ctrl Pts',(-17.2149552435157,6.25122984378583,36.2402006917209));
#33539=CARTESIAN_POINT('Ctrl Pts',(-13.3040026940452,6.05595707526583,34.3477946257551));
#33540=CARTESIAN_POINT('Ctrl Pts',(-9.6525471111465,5.8568061689083,32.0261986676909));
#33541=CARTESIAN_POINT('Ctrl Pts',(-6.37476293151624,5.64398234710963,29.2009985033296));
#33542=CARTESIAN_POINT('Ctrl Pts',(-3.54433846437633,5.40587468584602,25.9217831684824));
#33543=CARTESIAN_POINT('Ctrl Pts',(-1.45858600572521,5.18017895256177,22.822442252468));
#33544=CARTESIAN_POINT('Ctrl Pts',(-0.31729954633703,5.01301666232781,20.5789820379423));
#33545=CARTESIAN_POINT('Ctrl Pts',(0.344196822049049,4.89707445701614,19.0498138141221));
#33546=CARTESIAN_POINT('Ctrl Pts',(0.495324122044482,4.86894780999335,18.6807807474581));
#33547=CARTESIAN_POINT('Ctrl Pts',(0.638889978344851,4.84055053954568,18.3098379674021));
#33548=CARTESIAN_POINT('Ctrl Pts',(-32.8758727169027,3.57357815210241,40.2949547456763));
#33549=CARTESIAN_POINT('Ctrl Pts',(-32.4767273615688,3.55599962931061,40.3451948528862));
#33550=CARTESIAN_POINT('Ctrl Pts',(-32.0751371433406,3.53868515668548,40.3881395758659));
#33551=CARTESIAN_POINT('Ctrl Pts',(-30.3516146892127,3.46609807861293,40.5396626066785));
#33552=CARTESIAN_POINT('Ctrl Pts',(-27.7324819356722,3.36435917107101,40.6068323220244));
#33553=CARTESIAN_POINT('Ctrl Pts',(-23.8984124909247,3.23426720235262,40.2369275639187));
#33554=CARTESIAN_POINT('Ctrl Pts',(-19.5756899976202,3.10147907156715,39.2843419828594));
#33555=CARTESIAN_POINT('Ctrl Pts',(-15.4908341395163,2.98285053627008,37.7157037013977));
#33556=CARTESIAN_POINT('Ctrl Pts',(-11.718544299807,2.86388130857434,35.5842699988208));
#33557=CARTESIAN_POINT('Ctrl Pts',(-8.23601495093128,2.73730530568202,33.0312127971187));
#33558=CARTESIAN_POINT('Ctrl Pts',(-5.16523654947227,2.59247375589619,29.9869957655452));
#33559=CARTESIAN_POINT('Ctrl Pts',(-2.58023204587429,2.41842603756845,26.5056777619934));
#33560=CARTESIAN_POINT('Ctrl Pts',(-0.731320310752,2.24547053120763,23.2467344970765));
#33561=CARTESIAN_POINT('Ctrl Pts',(0.234328739827367,2.11246131963295,20.9073033347448));
#33562=CARTESIAN_POINT('Ctrl Pts',(0.774418224855581,2.01884144332686,19.3188699442435));
#33563=CARTESIAN_POINT('Ctrl Pts',(0.895998757480463,1.99605339732081,18.9363491825155));
#33564=CARTESIAN_POINT('Ctrl Pts',(1.0096286841352,1.9729679754383,18.5526533795054));
#33565=CARTESIAN_POINT('Ctrl Pts',(-31.3974772080596,0.237308438758995,
42.1889013144209));
#33566=CARTESIAN_POINT('Ctrl Pts',(-30.9966927888425,0.227921876287717,
42.2219698988398));
#33567=CARTESIAN_POINT('Ctrl Pts',(-30.5937820398667,0.218854274805993,
42.2475319255546));
#33568=CARTESIAN_POINT('Ctrl Pts',(-28.866041531999,0.181679983795775,42.3239971106882));
#33569=CARTESIAN_POINT('Ctrl Pts',(-26.2475430587419,0.133848323063104,
42.274846063482));
#33570=CARTESIAN_POINT('Ctrl Pts',(-22.4359447693504,0.0830496793456984,
41.7279849455362));
#33571=CARTESIAN_POINT('Ctrl Pts',(-18.1647975152526,0.0403924264632703,
40.5680465840115));
#33572=CARTESIAN_POINT('Ctrl Pts',(-14.1635084800691,0.00837005963384143,
38.7934300768119));
#33573=CARTESIAN_POINT('Ctrl Pts',(-10.5071625432585,-0.0279539839125438,
36.4611931292656));
#33574=CARTESIAN_POINT('Ctrl Pts',(-7.16665730012202,-0.0750512999789021,
33.7135147932952));
#33575=CARTESIAN_POINT('Ctrl Pts',(-4.27071386437358,-0.14423024726241,
30.4849603838039));
#33576=CARTESIAN_POINT('Ctrl Pts',(-1.89363332772792,-0.245792879606331,
26.8334203010956));
#33577=CARTESIAN_POINT('Ctrl Pts',(-0.245746173750661,-0.358291148292244,
23.4399943636853));
#33578=CARTESIAN_POINT('Ctrl Pts',(0.570610862782009,-0.451704594358635,
21.0196785831955));
#33579=CARTESIAN_POINT('Ctrl Pts',(1.00744205759503,-0.519340602547392,
19.3812974878904));
#33580=CARTESIAN_POINT('Ctrl Pts',(1.10392460430938,-0.535923052101836,
18.9874616998164));
#33581=CARTESIAN_POINT('Ctrl Pts',(1.19215808188825,-0.552841667182328,
18.5931197045587));
#33582=CARTESIAN_POINT('Ctrl Pts',(-30.5294236725591,-2.14030259993981,
43.3034186854275));
#33583=CARTESIAN_POINT('Ctrl Pts',(-30.1272931149697,-2.14321532053782,
43.3254158563938));
#33584=CARTESIAN_POINT('Ctrl Pts',(-29.72324694576,-2.14576465810466,43.3397662219238));
#33585=CARTESIAN_POINT('Ctrl Pts',(-27.9915993478864,-2.15494826818845,
43.3678047673857));
#33586=CARTESIAN_POINT('Ctrl Pts',(-25.3718743099029,-2.16016260296573,
43.2435221176539));
#33587=CARTESIAN_POINT('Ctrl Pts',(-21.572867015554,-2.1481556077715,42.5821474979001));
#33588=CARTESIAN_POINT('Ctrl Pts',(-17.333414526286,-2.11918777525101,41.2878074756749));
#33589=CARTESIAN_POINT('Ctrl Pts',(-13.3852721551486,-2.08197924289826,
39.379449384515));
#33590=CARTESIAN_POINT('Ctrl Pts',(-9.80377918929066,-2.05170003121316,
36.9166597127083));
#33591=CARTESIAN_POINT('Ctrl Pts',(-6.55560827573149,-2.03426137368081,
34.0423409270553));
#33592=CARTESIAN_POINT('Ctrl Pts',(-3.77398725841762,-2.04135770257883,
30.6937413306207));
#33593=CARTESIAN_POINT('Ctrl Pts',(-1.53339439133958,-2.08278583441843,
26.9313113438869));
#33594=CARTESIAN_POINT('Ctrl Pts',(-0.0177672591392232,-2.14471303148954,
23.4502813702109));
#33595=CARTESIAN_POINT('Ctrl Pts',(0.700190966747434,-2.20477046252904,
20.9773004459268));
#33596=CARTESIAN_POINT('Ctrl Pts',(1.06891378933942,-2.25046208753918,19.3064141960021));
#33597=CARTESIAN_POINT('Ctrl Pts',(1.14886051042696,-2.26180965939547,18.9052387021536));
#33598=CARTESIAN_POINT('Ctrl Pts',(1.22037994045603,-2.27353152926925,18.5040148697326));
#33599=CARTESIAN_POINT('Ctrl Pts',(-29.9728399373354,-3.83428286431684,
44.0191242698361));
#33600=CARTESIAN_POINT('Ctrl Pts',(-29.5696745140238,-3.83237339034492,
44.0336174040068));
#33601=CARTESIAN_POINT('Ctrl Pts',(-29.1647389499247,-3.83006698099443,
44.0403669998921));
#33602=CARTESIAN_POINT('Ctrl Pts',(-27.4299435681702,-3.81839846831683,
44.0355693932585));
#33603=CARTESIAN_POINT('Ctrl Pts',(-24.808696764347,-3.79185933798401,43.860310033771));
#33604=CARTESIAN_POINT('Ctrl Pts',(-21.0174144082698,-3.73301479320489,
43.1211526099474));
#33605=CARTESIAN_POINT('Ctrl Pts',(-16.7987669069511,-3.65055513724086,
41.7354370320634));
#33606=CARTESIAN_POINT('Ctrl Pts',(-12.8863048378013,-3.56151400652134,
39.7360659076511));
#33607=CARTESIAN_POINT('Ctrl Pts',(-9.35554180296775,-3.48120332570528,
37.1843738425572));
#33608=CARTESIAN_POINT('Ctrl Pts',(-6.17021960178868,-3.41513875248544,
34.2237830512071));
#33609=CARTESIAN_POINT('Ctrl Pts',(-3.46668816079854,-3.37526128513496,
30.7933795971532));
#33610=CARTESIAN_POINT('Ctrl Pts',(-1.31954448869267,-3.37099617994084,
26.9553877055552));
#33611=CARTESIAN_POINT('Ctrl Pts',(0.105403626449547,-3.39437469848804,
23.4146796719729));
#33612=CARTESIAN_POINT('Ctrl Pts',(0.7558264201022,-3.42893690611626,20.9058438397504));
#33613=CARTESIAN_POINT('Ctrl Pts',(1.07778274982802,-3.45783930783476,19.2128393202058));
#33614=CARTESIAN_POINT('Ctrl Pts',(1.14638473165933,-3.46518513130081,18.806679408153));
#33615=CARTESIAN_POINT('Ctrl Pts',(1.20644655773061,-3.47293757911652,18.4007919683856));
#33616=CARTESIAN_POINT('Ctrl Pts',(-29.8240879871509,-4.30636894546118,
44.2105267227162));
#33617=CARTESIAN_POINT('Ctrl Pts',(-29.4206225151076,-4.3031084050989,44.2229739248513));
#33618=CARTESIAN_POINT('Ctrl Pts',(-29.0154266865265,-4.29944065268701,
44.2276505601386));
#33619=CARTESIAN_POINT('Ctrl Pts',(-27.2796978130663,-4.28192251284736,
44.2138948132052));
#33620=CARTESIAN_POINT('Ctrl Pts',(-24.6579368258278,-4.24645759656194,
44.0247144994774));
#33621=CARTESIAN_POINT('Ctrl Pts',(-20.8686620252869,-4.17439213330946,
43.2642815747257));
#33622=CARTESIAN_POINT('Ctrl Pts',(-16.6556313915342,-4.07676875425951,
41.8535410709043));
#33623=CARTESIAN_POINT('Ctrl Pts',(-12.752916079089,-3.97294922980807,39.8292172170953));
#33624=CARTESIAN_POINT('Ctrl Pts',(-9.23607101592842,-3.87828739688684,
37.2531390788911));
#33625=CARTESIAN_POINT('Ctrl Pts',(-6.06801599636428,-3.79820251809058,
34.2688877835182));
#33626=CARTESIAN_POINT('Ctrl Pts',(-3.38594976443961,-3.74469501429227,
30.8160631689765));
#33627=CARTESIAN_POINT('Ctrl Pts',(-1.26447813113574,-3.72710099262819,
26.9573886132689));
#33628=CARTESIAN_POINT('Ctrl Pts',(0.135589853537579,-3.7392015362719,23.4003753828037));
#33629=CARTESIAN_POINT('Ctrl Pts',(0.767503701216293,-3.76629674044718,
20.8817611257437));
#33630=CARTESIAN_POINT('Ctrl Pts',(1.07665298555957,-3.79028538091932,19.182731725672));
#33631=CARTESIAN_POINT('Ctrl Pts',(1.14215062469445,-3.79646095010219,18.7752153335603));
#33632=CARTESIAN_POINT('Ctrl Pts',(1.19907952975018,-3.80305340259771,18.3680599208473));
#33633=CARTESIAN_POINT('Ctrl Pts',(-29.6806279783958,-4.78145508078572,
44.3952414011369));
#33634=CARTESIAN_POINT('Ctrl Pts',(-29.2768504019181,-4.77682808742727,
44.4056744850212));
#33635=CARTESIAN_POINT('Ctrl Pts',(-28.8713813649358,-4.7717826224726,44.4083097320835));
#33636=CARTESIAN_POINT('Ctrl Pts',(-27.1346599350118,-4.74834091216943,
44.3857294295924));
#33637=CARTESIAN_POINT('Ctrl Pts',(-24.5122959636537,-4.70381966688121,
44.1828218130499));
#33638=CARTESIAN_POINT('Ctrl Pts',(-20.7249024233729,-4.61828583278682,
43.4013748323987));
#33639=CARTESIAN_POINT('Ctrl Pts',(-16.5173497068994,-4.50515190400754,
41.9658851598471));
#33640=CARTESIAN_POINT('Ctrl Pts',(-12.6242519830332,-4.38613315046716,
39.9168561359679));
#33641=CARTESIAN_POINT('Ctrl Pts',(-9.12119860544565,-4.27662792828432,
37.3166215213372));
#33642=CARTESIAN_POINT('Ctrl Pts',(-5.97027712488791,-4.18197237106197,
34.3089362976155));
#33643=CARTESIAN_POINT('Ctrl Pts',(-3.30951923630238,-4.11421750462538,
30.833918806753));
#33644=CARTESIAN_POINT('Ctrl Pts',(-1.21351550607071,-4.08262421860679,
26.9547993627852));
#33645=CARTESIAN_POINT('Ctrl Pts',(0.161901966116654,-4.0828488851085,23.381697762374));
#33646=CARTESIAN_POINT('Ctrl Pts',(0.775499329277603,-4.10207414795096,
20.8534525370212));
#33647=CARTESIAN_POINT('Ctrl Pts',(1.07198479735696,-4.12088738197538,19.1484961887738));
#33648=CARTESIAN_POINT('Ctrl Pts',(1.13441433400836,-4.12583098108427,18.7396458756966));
#33649=CARTESIAN_POINT('Ctrl Pts',(1.18824830736423,-4.13120272145022,18.3312440582198));
#33650=CARTESIAN_POINT('',(-42.5975526516,20.7105311502984,19.56306858979));
#33651=CARTESIAN_POINT('Ctrl Pts',(-42.5975526516,20.7105311502984,19.56306858979));
#33652=CARTESIAN_POINT('Ctrl Pts',(-37.5762221249469,20.5483438544848,20.8499577962863));
#33653=CARTESIAN_POINT('Ctrl Pts',(-32.3097534431554,20.4520245495079,21.1410367283647));
#33654=CARTESIAN_POINT('Ctrl Pts',(-22.0288042740374,20.3052748660675,19.8252715829174));
#33655=CARTESIAN_POINT('Ctrl Pts',(-17.0125234745079,20.248474007324,18.2209789914172));
#33656=CARTESIAN_POINT('Ctrl Pts',(-12.4794056444224,20.1925493450898,15.715137789166));
#33657=CARTESIAN_POINT('',(-19.776612741422,-3.27137091447503,42.4988384174391));
#33658=CARTESIAN_POINT('Ctrl Pts',(-42.5975526515946,20.7105311502992,19.5630685897878));
#33659=CARTESIAN_POINT('Ctrl Pts',(-41.2774004556305,19.9641940681955,22.4376316497411));
#33660=CARTESIAN_POINT('Ctrl Pts',(-39.7028421419984,18.733618922395,25.0874965293065));
#33661=CARTESIAN_POINT('Ctrl Pts',(-36.0874408763569,15.6437709263415,30.09428841202));
#33662=CARTESIAN_POINT('Ctrl Pts',(-33.9437320263055,13.6706054953475,32.4640497220532));
#33663=CARTESIAN_POINT('Ctrl Pts',(-29.6530167610139,9.45712578015136,36.416476789843));
#33664=CARTESIAN_POINT('Ctrl Pts',(-27.4644787406163,7.18268855808106,38.0675475180451));
#33665=CARTESIAN_POINT('Ctrl Pts',(-23.3434412931498,2.26699026933705,40.7209158524528));
#33666=CARTESIAN_POINT('Ctrl Pts',(-21.4078194194595,-0.365223992194613,
41.73976451752));
#33667=CARTESIAN_POINT('Ctrl Pts',(-19.7766121648793,-3.27137053313467,
42.4988386384589));
#33668=CARTESIAN_POINT('Ctrl Pts',(-19.7766128803973,-3.27137100135121,
42.4988379590673));
#33669=CARTESIAN_POINT('Ctrl Pts',(-19.0339274479275,-3.25992112204952,
42.2714904731699));
#33670=CARTESIAN_POINT('Ctrl Pts',(-18.3028671461025,-3.24789096533568,
42.0167733291065));
#33671=CARTESIAN_POINT('Ctrl Pts',(-17.5847573966283,-3.23555894384663,
41.7357426201857));
#33672=CARTESIAN_POINT('Ctrl Pts',(-15.82608090219,-3.2053573815679,41.047488349364));
#33673=CARTESIAN_POINT('Ctrl Pts',(-14.1450790808029,-3.17334534347451,
40.201411150032));
#33674=CARTESIAN_POINT('Ctrl Pts',(-12.561157306208,-3.14345008158506,39.2131583578373));
#33675=CARTESIAN_POINT('Ctrl Pts',(-11.5052094029128,-3.12351990598109,
38.5543231296199));
#33676=CARTESIAN_POINT('Ctrl Pts',(-10.4924081914375,-3.10453051989494,
37.8322987426006));
#33677=CARTESIAN_POINT('Ctrl Pts',(-9.52847648856522,-3.08752071373526,
37.0517562442537));
#33678=CARTESIAN_POINT('Ctrl Pts',(-8.56454478619749,-3.07051090758448,
36.2712137463155));
#33679=CARTESIAN_POINT('Ctrl Pts',(-7.64948259237388,-3.0554806813514,35.4321531371102));
#33680=CARTESIAN_POINT('Ctrl Pts',(-6.78900009497131,-3.04339100491455,
34.5392583133731));
#33681=CARTESIAN_POINT('Ctrl Pts',(-5.49827635047142,-3.02525649028182,
33.1999160794317));
#33682=CARTESIAN_POINT('Ctrl Pts',(-4.33035692256822,-3.01373821257335,
31.7394468631442));
#33683=CARTESIAN_POINT('Ctrl Pts',(-3.30441544543477,-3.01128625574909,
30.1737249320072));
#33684=CARTESIAN_POINT('Ctrl Pts',(-2.62045446228512,-3.00965161787009,
29.1299103137002));
#33685=CARTESIAN_POINT('Ctrl Pts',(-1.99959479025531,-3.01204645592803,
28.0393167111781));
#33686=CARTESIAN_POINT('Ctrl Pts',(-1.44749052671152,-3.01891855380822,
26.9066548859025));
#33687=CARTESIAN_POINT('Ctrl Pts',(-0.895386329367994,-3.02579065086441,
25.7739931964392));
#33688=CARTESIAN_POINT('Ctrl Pts',(-0.412037523989561,-3.03714000665748,
24.5992632942881));
#33689=CARTESIAN_POINT('Ctrl Pts',(-0.00308425577624904,-3.05321938564873,
23.3871704735693));
#33690=CARTESIAN_POINT('Ctrl Pts',(0.165431602385786,-3.05984515577954,
22.8877078754395));
#33691=CARTESIAN_POINT('Ctrl Pts',(0.321315192441404,-3.06727406915266,
22.381901115368));
#33692=CARTESIAN_POINT('Ctrl Pts',(0.464173291851462,-3.07550335254719,
21.8700789527947));
#33693=CARTESIAN_POINT('Ctrl Pts',(-29.5860843849178,-4.68328060676847,
44.5216251990609));
#33694=CARTESIAN_POINT('Ctrl Pts',(-29.1809745858381,-4.67927906663786,
44.5315997635342));
#33695=CARTESIAN_POINT('Ctrl Pts',(-28.7741766395213,-4.67486342687383,
44.5337119281872));
#33696=CARTESIAN_POINT('Ctrl Pts',(-27.0369350215887,-4.65418501649615,
44.5086929582487));
#33697=CARTESIAN_POINT('Ctrl Pts',(-24.416253162149,-4.61395560865182,44.3020849732412));
#33698=CARTESIAN_POINT('Ctrl Pts',(-20.6316091853443,-4.53496565777432,
43.5151118207757));
#33699=CARTESIAN_POINT('Ctrl Pts',(-16.4275307990086,-4.42959393838223,
42.0732275761618));
#33700=CARTESIAN_POINT('Ctrl Pts',(-12.5382448797194,-4.31850354734918,
40.0179024219213));
#33701=CARTESIAN_POINT('Ctrl Pts',(-9.03935092612681,-4.2170896233612,37.4115163382363));
#33702=CARTESIAN_POINT('Ctrl Pts',(-5.89288171525852,-4.13063759391767,
34.3978116754749));
#33703=CARTESIAN_POINT('Ctrl Pts',(-3.23694972107052,-4.07121155600733,
30.9169763478869));
#33704=CARTESIAN_POINT('Ctrl Pts',(-1.14615791734321,-4.04803120464602,
27.0322881721863));
#33705=CARTESIAN_POINT('Ctrl Pts',(0.224522517554149,-4.055480889925,23.4546075941498));
#33706=CARTESIAN_POINT('Ctrl Pts',(0.834789683250672,-4.07952578289679,
20.9234587390748));
#33707=CARTESIAN_POINT('Ctrl Pts',(1.12940732404397,-4.10152925776619,19.214455857901));
#33708=CARTESIAN_POINT('Ctrl Pts',(1.19158024061946,-4.1072571624472,18.8029939189201));
#33709=CARTESIAN_POINT('Ctrl Pts',(1.2450644513097,-4.11341014061892,18.3920080529356));
#33710=CARTESIAN_POINT('Ctrl Pts',(-29.7642796229678,-4.24009445412503,
44.2925926955476));
#33711=CARTESIAN_POINT('Ctrl Pts',(-29.359411518692,-4.23725223817857,44.3047887517873));
#33712=CARTESIAN_POINT('Ctrl Pts',(-28.9528099886829,-4.23400446880359,
44.3091515696117));
#33713=CARTESIAN_POINT('Ctrl Pts',(-27.2162036125542,-4.21832863439708,
44.2938289943612));
#33714=CARTESIAN_POINT('Ctrl Pts',(-24.5955479639773,-4.18572164472913,
44.1022702841641));
#33715=CARTESIAN_POINT('Ctrl Pts',(-20.8080715768724,-4.11799618192084,
43.3382863119255));
#33716=CARTESIAN_POINT('Ctrl Pts',(-16.5973033266347,-4.02550335874969,
41.9234398290087));
#33717=CARTESIAN_POINT('Ctrl Pts',(-12.697056845913,-3.92690475481451,39.8950785227414));
#33718=CARTESIAN_POINT('Ctrl Pts',(-9.18289043977616,-3.83755718932749,
37.3150628289422));
#33719=CARTESIAN_POINT('Ctrl Pts',(-6.01768716647963,-3.76285616468038,
34.3269670070901));
#33720=CARTESIAN_POINT('Ctrl Pts',(-3.33869209457895,-3.71481495977278,
30.8704356073741));
#33721=CARTESIAN_POINT('Ctrl Pts',(-1.2205165590504,-3.70275434803773,27.0082200856332));
#33722=CARTESIAN_POINT('Ctrl Pts',(0.176569306956024,-3.71962751323487,
23.4482980813067));
#33723=CARTESIAN_POINT('Ctrl Pts',(0.806392352236958,-3.74992063397164,
20.9278383983267));
#33724=CARTESIAN_POINT('Ctrl Pts',(1.11452777256288,-3.77604797989279,19.2254460436222));
#33725=CARTESIAN_POINT('Ctrl Pts',(1.17998786511121,-3.78276245762616,18.815479564919));
#33726=CARTESIAN_POINT('Ctrl Pts',(1.23678687530853,-3.78989370687861,18.4058928046142));
#33727=CARTESIAN_POINT('Ctrl Pts',(-29.9461184866339,-3.80075287541765,
44.0589752842181));
#33728=CARTESIAN_POINT('Ctrl Pts',(-29.5414810641717,-3.79905339336963,
44.0734114048756));
#33729=CARTESIAN_POINT('Ctrl Pts',(-29.1350644418468,-3.79695621683146,
44.0800431213998));
#33730=CARTESIAN_POINT('Ctrl Pts',(-27.3990422401927,-3.78620663871065,
44.0744931264123));
#33731=CARTESIAN_POINT('Ctrl Pts',(-24.7783398189311,-3.76109400159902,
43.8980891928852));
#33732=CARTESIAN_POINT('Ctrl Pts',(-20.9879390718351,-3.70440674399875,
43.1572232592788));
#33733=CARTESIAN_POINT('Ctrl Pts',(-16.7703956156188,-3.62448835210827,
41.7695337527048));
#33734=CARTESIAN_POINT('Ctrl Pts',(-12.8591316466056,-3.53802316526296,
39.7682243997015));
#33735=CARTESIAN_POINT('Ctrl Pts',(-9.32966070272471,-3.46032715355504,
37.2146458262608));
#33736=CARTESIAN_POINT('Ctrl Pts',(-6.14570601219839,-3.39690914788247,
34.2522176672827));
#33737=CARTESIAN_POINT('Ctrl Pts',(-3.44363678759394,-3.35971861494906,
30.820047545745));
#33738=CARTESIAN_POINT('Ctrl Pts',(-1.29805125064107,-3.35817927654809,
26.9803719825628));
#33739=CARTESIAN_POINT('Ctrl Pts',(0.125494730687221,-3.38391914529348,
23.4382826058056));
#33740=CARTESIAN_POINT('Ctrl Pts',(0.774937722763661,-3.42007079724739,
20.9285700499322));
#33741=CARTESIAN_POINT('Ctrl Pts',(1.09664683736935,-3.45006162272336,19.2328302145806));
#33742=CARTESIAN_POINT('Ctrl Pts',(1.16540949069431,-3.45770043113048,18.8243690332114));
#33743=CARTESIAN_POINT('Ctrl Pts',(1.22554046200446,-3.46574819271174,18.4161908869355));
#33744=CARTESIAN_POINT('Ctrl Pts',(-30.6001603149859,-2.2653457359543,43.2190559709685));
#33745=CARTESIAN_POINT('Ctrl Pts',(-30.1962920925288,-2.26761569662348,
43.2414546676051));
#33746=CARTESIAN_POINT('Ctrl Pts',(-29.790483177066,-2.26951335386862,43.2561496325629));
#33747=CARTESIAN_POINT('Ctrl Pts',(-28.056332027324,-2.27586002752392,43.2853222550732));
#33748=CARTESIAN_POINT('Ctrl Pts',(-25.4351951428781,-2.27671432942662,
43.1627196453144));
#33749=CARTESIAN_POINT('Ctrl Pts',(-21.6341437305441,-2.25814179129592,
42.5038126448418));
#33750=CARTESIAN_POINT('Ctrl Pts',(-17.3923960901783,-2.2214798205824,41.2122877014012));
#33751=CARTESIAN_POINT('Ctrl Pts',(-13.4420746485557,-2.17652897108851,
39.3066630970881));
#33752=CARTESIAN_POINT('Ctrl Pts',(-9.85852300070146,-2.13845241575724,
36.8465264101127));
#33753=CARTESIAN_POINT('Ctrl Pts',(-6.60839102281067,-2.11316923258448,
33.9747989860199));
#33754=CARTESIAN_POINT('Ctrl Pts',(-3.82493207095045,-2.11235831802136,
30.6287183522426));
#33755=CARTESIAN_POINT('Ctrl Pts',(-1.58262415787283,-2.14581153060268,
26.8687460420206));
#33756=CARTESIAN_POINT('Ctrl Pts',(-0.0656103164190895,-2.20085463389179,
23.3897875019218));
#33757=CARTESIAN_POINT('Ctrl Pts',(0.653217774137632,-2.25628908058851,
20.9181693846315));
#33758=CARTESIAN_POINT('Ctrl Pts',(1.02296935998166,-2.29898278275007,19.2460320909997));
#33759=CARTESIAN_POINT('Ctrl Pts',(1.10343093441437,-2.30966173471912,18.842915305665));
#33760=CARTESIAN_POINT('Ctrl Pts',(1.17537432901808,-2.32072459453129,18.4397418535062));
#33761=CARTESIAN_POINT('Ctrl Pts',(-31.8292095903569,0.42091842584111,41.6423330468386));
#33762=CARTESIAN_POINT('Ctrl Pts',(-31.426588380617,0.412015546281074,41.6791686699069));
#33763=CARTESIAN_POINT('Ctrl Pts',(-31.0217428525285,0.403442573942463,
41.7084816508355));
#33764=CARTESIAN_POINT('Ctrl Pts',(-29.2904348792228,0.368526239150617,
41.8006000821719));
#33765=CARTESIAN_POINT('Ctrl Pts',(-26.6677579163665,0.324281374370589,
41.7754850488311));
#33766=CARTESIAN_POINT('Ctrl Pts',(-22.8465337117467,0.279215865745994,
41.2649689473965));
#33767=CARTESIAN_POINT('Ctrl Pts',(-18.5602087327645,0.243759038204317,
40.147435296854));
#33768=CARTESIAN_POINT('Ctrl Pts',(-14.5387725951337,0.21967725703067,38.4148047775327));
#33769=CARTESIAN_POINT('Ctrl Pts',(-10.8572617892506,0.192114722189047,
36.1235067085039));
#33770=CARTESIAN_POINT('Ctrl Pts',(-7.48755331988048,0.154437491851918,
33.4155983170629));
#33771=CARTESIAN_POINT('Ctrl Pts',(-4.55732909655327,0.0954817696064694,
30.2249414587457));
#33772=CARTESIAN_POINT('Ctrl Pts',(-2.14084655383702,0.0048363712043943,
26.6088223096227));
#33773=CARTESIAN_POINT('Ctrl Pts',(-0.455654318055976,-0.0979118428630517,
23.2437893603337));
#33774=CARTESIAN_POINT('Ctrl Pts',(0.387941255052986,-0.184631554593919,
20.8409136479811));
#33775=CARTESIAN_POINT('Ctrl Pts',(0.844059787599826,-0.247909792323189,
19.2113700902569));
#33776=CARTESIAN_POINT('Ctrl Pts',(0.945576151375779,-0.263520166061751,
18.8179166382569));
#33777=CARTESIAN_POINT('Ctrl Pts',(1.03880163967271,-0.279478515480188,
18.423810774743));
#33778=CARTESIAN_POINT('Ctrl Pts',(-33.7395940988688,3.93922736422659,39.1963288075476));
#33779=CARTESIAN_POINT('Ctrl Pts',(-33.338359123107,3.92273017306588,39.2538975757074));
#33780=CARTESIAN_POINT('Ctrl Pts',(-32.9345110720053,3.90651491483579,39.3041976635156));
#33781=CARTESIAN_POINT('Ctrl Pts',(-31.2057260147983,3.83888692720806,39.4866672841393));
#33782=CARTESIAN_POINT('Ctrl Pts',(-28.5787152339974,3.74496038387833,39.6013457126449));
#33783=CARTESIAN_POINT('Ctrl Pts',(-24.7261416632,3.6271896762232,39.3032423032837));
#33784=CARTESIAN_POINT('Ctrl Pts',(-20.3739691877485,3.50969140214063,38.4343783563741));
#33785=CARTESIAN_POINT('Ctrl Pts',(-16.2497646181535,3.40771510315772,36.9485603352936));
#33786=CARTESIAN_POINT('Ctrl Pts',(-12.4281284545972,3.30695483103527,34.8977873111395));
#33787=CARTESIAN_POINT('Ctrl Pts',(-8.88820541265663,3.1998573133211,32.4229990482932));
#33788=CARTESIAN_POINT('Ctrl Pts',(-5.74991377138373,3.07607789704229,29.4532363326592));
#33789=CARTESIAN_POINT('Ctrl Pts',(-3.08718802358192,2.92448144596071,26.0413441207066));
#33790=CARTESIAN_POINT('Ctrl Pts',(-1.16461755079814,2.77158317941627,22.8379182506629));
#33791=CARTESIAN_POINT('Ctrl Pts',(-0.145141170452875,2.65236568914073,
20.5324826814612));
#33792=CARTESIAN_POINT('Ctrl Pts',(0.432661725556691,2.56779645721963,18.9632953151811));
#33793=CARTESIAN_POINT('Ctrl Pts',(0.563887154443276,2.54707902977605,18.5835837371794));
#33794=CARTESIAN_POINT('Ctrl Pts',(0.687186542465773,2.52604544176493,18.2024213506929));
#33795=CARTESIAN_POINT('Ctrl Pts',(-36.1213273778177,7.64857049485316,36.1506600847068));
#33796=CARTESIAN_POINT('Ctrl Pts',(-35.7213655257733,7.62538079009264,36.2323665893927));
#33797=CARTESIAN_POINT('Ctrl Pts',(-35.318370358813,7.6024320797305,36.3070907747722));
#33798=CARTESIAN_POINT('Ctrl Pts',(-33.5913541783468,7.50598047950645,36.594676968361));
#33799=CARTESIAN_POINT('Ctrl Pts',(-30.9577397928421,7.36825978906471,36.8718667276266));
#33800=CARTESIAN_POINT('Ctrl Pts',(-27.0670307767398,7.18657585481396,36.8203372030951));
#33801=CARTESIAN_POINT('Ctrl Pts',(-22.6371118575503,6.99739878870591,36.2397466988013));
#33802=CARTESIAN_POINT('Ctrl Pts',(-18.3932178061842,6.82819742189185,35.0395940680358));
#33803=CARTESIAN_POINT('Ctrl Pts',(-14.4094498834431,6.66543158101024,33.2667925298684));
#33804=CARTESIAN_POINT('Ctrl Pts',(-10.6732059289801,6.50060855796851,31.0610971404567));
#33805=CARTESIAN_POINT('Ctrl Pts',(-7.29557708527982,6.32441606849526,28.3459245289215));
#33806=CARTESIAN_POINT('Ctrl Pts',(-4.35011979267042,6.12505774886043,25.1690331245211));
#33807=CARTESIAN_POINT('Ctrl Pts',(-2.1552924018102,5.93384517916791,22.1512975283732));
#33808=CARTESIAN_POINT('Ctrl Pts',(-0.934264384510294,5.79035915091665,
19.9576366206874));
#33809=CARTESIAN_POINT('Ctrl Pts',(-0.217066032849526,5.69001969995687,
18.4576188984149));
#33810=CARTESIAN_POINT('Ctrl Pts',(-0.0517570763689102,5.66551509710643,
18.0937381573601));
#33811=CARTESIAN_POINT('Ctrl Pts',(0.106095228629841,5.64071489355821,17.7275698974483));
#33812=CARTESIAN_POINT('Ctrl Pts',(-38.3661892429674,10.6050661536892,33.2823591784344));
#33813=CARTESIAN_POINT('Ctrl Pts',(-37.9671384846144,10.5777689837161,33.3854884036947));
#33814=CARTESIAN_POINT('Ctrl Pts',(-37.5647102405911,10.5506896266998,33.4818781105384));
#33815=CARTESIAN_POINT('Ctrl Pts',(-35.838584594256,10.4365567481294,33.8626670870572));
#33816=CARTESIAN_POINT('Ctrl Pts',(-33.1982305732567,10.2719415070743,34.2838556108487));
#33817=CARTESIAN_POINT('Ctrl Pts',(-29.2728489305625,10.0511774947007,34.4505393124499));
#33818=CARTESIAN_POINT('Ctrl Pts',(-24.7735462962233,9.81863871620139,34.1247592769514));
#33819=CARTESIAN_POINT('Ctrl Pts',(-20.423779822698,9.60967367489776,33.1767389206439));
#33820=CARTESIAN_POINT('Ctrl Pts',(-16.2972164409564,9.41153176383594,31.6489144657926));
#33821=CARTESIAN_POINT('Ctrl Pts',(-12.3884323729163,9.21500541081661,29.6800767690944));
#33822=CARTESIAN_POINT('Ctrl Pts',(-8.80083669338724,9.01175979868378,27.1886192523672));
#33823=CARTESIAN_POINT('Ctrl Pts',(-5.6076513402522,8.78956564702969,24.2178312637806));
#33824=CARTESIAN_POINT('Ctrl Pts',(-3.17445016977068,8.58124477590158,21.3626542097078));
#33825=CARTESIAN_POINT('Ctrl Pts',(-1.77705695674595,8.42762540105217,19.2666254426567));
#33826=CARTESIAN_POINT('Ctrl Pts',(-0.937912040084691,8.32086564673385,
17.8269442237021));
#33827=CARTESIAN_POINT('Ctrl Pts',(-0.74276181745419,8.29482075310626,17.476953167516));
#33828=CARTESIAN_POINT('Ctrl Pts',(-0.554631609392133,8.26849188852043,
17.1240221481785));
#33829=CARTESIAN_POINT('Ctrl Pts',(-41.0932888255619,13.6252616883324,29.7990058126645));
#33830=CARTESIAN_POINT('Ctrl Pts',(-40.6951709804398,13.5952855444977,29.926812980099));
#33831=CARTESIAN_POINT('Ctrl Pts',(-40.2933116112545,13.5655149131873,30.0481434512788));
#33832=CARTESIAN_POINT('Ctrl Pts',(-38.5680000299751,13.4398628522405,30.5361601005493));
#33833=CARTESIAN_POINT('Ctrl Pts',(-35.919675614011,13.2576618204372,31.122937703186));
#33834=CARTESIAN_POINT('Ctrl Pts',(-31.9544063765669,13.0115743729063,31.5403078753727));
#33835=CARTESIAN_POINT('Ctrl Pts',(-27.3756745048881,12.751644575675,31.5069624080352));
#33836=CARTESIAN_POINT('Ctrl Pts',(-22.9050004035097,12.5189796899122,30.8479170967634));
#33837=CARTESIAN_POINT('Ctrl Pts',(-18.6155631238519,12.301865256328,29.6004493920025));
#33838=CARTESIAN_POINT('Ctrl Pts',(-14.5100993266258,12.0904144587841,27.9023158041159));
#33839=CARTESIAN_POINT('Ctrl Pts',(-10.6832885815738,11.8774764455751,25.6660504730613));
#33840=CARTESIAN_POINT('Ctrl Pts',(-7.20797317660949,11.6504923923572,22.9297998250813));
#33841=CARTESIAN_POINT('Ctrl Pts',(-4.5033571253319,11.4410171343385,20.2591620206668));
#33842=CARTESIAN_POINT('Ctrl Pts',(-2.90518917804047,11.2882220371981,18.273624202455));
#33843=CARTESIAN_POINT('Ctrl Pts',(-1.92723052845132,11.1823584691134,16.9020932343301));
#33844=CARTESIAN_POINT('Ctrl Pts',(-1.69811217151328,11.1565388193505,16.5678840962628));
#33845=CARTESIAN_POINT('Ctrl Pts',(-1.47551448673721,11.1304479812224,16.2300888450915));
#33846=CARTESIAN_POINT('Ctrl Pts',(-43.607077734618,15.9398275064074,26.5881648420301));
#33847=CARTESIAN_POINT('Ctrl Pts',(-43.2097562832355,15.9092719019138,26.7376510428101));
#33848=CARTESIAN_POINT('Ctrl Pts',(-42.8083994921326,15.8789225535602,26.8808736318176));
#33849=CARTESIAN_POINT('Ctrl Pts',(-41.0839333013364,15.7507918597713,27.4629402111696));
#33850=CARTESIAN_POINT('Ctrl Pts',(-38.4288723650909,15.5646999212503,28.1949050547109));
#33851=CARTESIAN_POINT('Ctrl Pts',(-34.4291690696808,15.3133344724918,28.8319001558766));
#33852=CARTESIAN_POINT('Ctrl Pts',(-29.7816206639597,15.0487502016962,29.054528697458));
#33853=CARTESIAN_POINT('Ctrl Pts',(-25.2060188107135,14.8142492774957,28.648116309137));
#33854=CARTESIAN_POINT('Ctrl Pts',(-20.7751262600391,14.5991383033468,27.6453833399041));
#33855=CARTESIAN_POINT('Ctrl Pts',(-16.4987857843687,14.3930646018661,26.183231029547));
#33856=CARTESIAN_POINT('Ctrl Pts',(-12.4640832639393,14.1899609567462,24.168963069841));
#33857=CARTESIAN_POINT('Ctrl Pts',(-8.74353496671818,13.977122935371,21.6361869570784));
#33858=CARTESIAN_POINT('Ctrl Pts',(-5.80297495936802,13.7824369346935,19.1251989416204));
#33859=CARTESIAN_POINT('Ctrl Pts',(-4.03025747473542,13.6409944051188,17.2348975933744));
#33860=CARTESIAN_POINT('Ctrl Pts',(-2.9316130946012,13.5429643472183,15.9219687959923));
#33861=CARTESIAN_POINT('Ctrl Pts',(-2.67298639300328,13.5190447294408,15.6014060795513));
#33862=CARTESIAN_POINT('Ctrl Pts',(-2.42046701738913,13.4948677704672,15.2767757095819));
#33863=CARTESIAN_POINT('Ctrl Pts',(-46.600622033322,18.188947172369,22.7630606377021));
#33864=CARTESIAN_POINT('Ctrl Pts',(-46.2043140287326,18.1597316481657,22.9372716024946));
#33865=CARTESIAN_POINT('Ctrl Pts',(-45.8036618532788,18.1307342364494,23.1054387932091));
#33866=CARTESIAN_POINT('Ctrl Pts',(-44.0808392894361,18.0083786966032,23.794574813762));
#33867=CARTESIAN_POINT('Ctrl Pts',(-41.4191469418867,17.830846834045,24.6917945378714));
#33868=CARTESIAN_POINT('Ctrl Pts',(-37.3817973723991,17.5925027676131,25.5786367906797));
#33869=CARTESIAN_POINT('Ctrl Pts',(-32.6577288281998,17.3443426911773,26.0922604044553));
#33870=CARTESIAN_POINT('Ctrl Pts',(-27.9645205180292,17.1289494695207,25.9727307503254));
#33871=CARTESIAN_POINT('Ctrl Pts',(-23.3744766463726,16.9369213116231,25.2475009189749));
#33872=CARTESIAN_POINT('Ctrl Pts',(-18.9055289559508,16.7575317657622,24.0525348461015));
#33873=CARTESIAN_POINT('Ctrl Pts',(-14.6361364276617,16.5859876106103,22.2890423286866));
#33874=CARTESIAN_POINT('Ctrl Pts',(-10.6384560691178,16.4095763329362,19.9853865921915));
#33875=CARTESIAN_POINT('Ctrl Pts',(-7.43109834396335,16.2491906636996,17.6535628588228));
#33876=CARTESIAN_POINT('Ctrl Pts',(-5.46091214715191,16.1323920433636,15.8696510460116));
#33877=CARTESIAN_POINT('Ctrl Pts',(-4.22570859084968,16.0510402241362,14.6219906158099));
#33878=CARTESIAN_POINT('Ctrl Pts',(-3.93374351400571,16.0311583490605,14.3166984129188));
#33879=CARTESIAN_POINT('Ctrl Pts',(-3.64746550911542,16.01103806515,14.006873262723));
#33880=CARTESIAN_POINT('Ctrl Pts',(-49.3109039376438,19.7983627848149,19.2977258249977));
#33881=CARTESIAN_POINT('Ctrl Pts',(-48.9156505478665,19.7720645135703,19.4934389062555));
#33882=CARTESIAN_POINT('Ctrl Pts',(-48.5158032965208,19.7460021313493,19.6832775632098));
#33883=CARTESIAN_POINT('Ctrl Pts',(-46.795314972639,19.6361820466171,20.465343757841));
#33884=CARTESIAN_POINT('Ctrl Pts',(-44.1292133031455,19.4774394485581,21.5059848500062));
#33885=CARTESIAN_POINT('Ctrl Pts',(-40.0610920842694,19.2670183310104,22.6095856728884));
#33886=CARTESIAN_POINT('Ctrl Pts',(-35.2727034384221,19.0520629838802,23.3755210446417));
#33887=CARTESIAN_POINT('Ctrl Pts',(-30.4793692627444,18.8717166252608,23.5044879484745));
#33888=CARTESIAN_POINT('Ctrl Pts',(-25.7530104929066,18.7178122962125,23.0192735306984));
#33889=CARTESIAN_POINT('Ctrl Pts',(-21.1186127047416,18.5794411422907,22.0550466235913));
#33890=CARTESIAN_POINT('Ctrl Pts',(-16.6471314095342,18.4529446490623,20.5075853478614));
#33891=CARTESIAN_POINT('Ctrl Pts',(-12.4104243963383,18.3257380682571,18.4006076730228));
#33892=CARTESIAN_POINT('Ctrl Pts',(-8.97273113596811,18.2102139945187,16.2219895556944));
#33893=CARTESIAN_POINT('Ctrl Pts',(-6.83193517130343,18.1249152482566,14.5285728120039));
#33894=CARTESIAN_POINT('Ctrl Pts',(-5.47870989582417,18.064727637235,13.3362339645435));
#33895=CARTESIAN_POINT('Ctrl Pts',(-5.15799058549254,18.0499634327475,13.0439317858091));
#33896=CARTESIAN_POINT('Ctrl Pts',(-4.84265063443571,18.0349776243875,12.746749095832));
#33897=CARTESIAN_POINT('Ctrl Pts',(-51.2947920922114,20.6836496418694,16.758668506747));
#33898=CARTESIAN_POINT('Ctrl Pts',(-50.90049041867,20.6606519170286,16.9695486618146));
#33899=CARTESIAN_POINT('Ctrl Pts',(-50.5014277827748,20.6379063239872,17.1746607300667));
#33900=CARTESIAN_POINT('Ctrl Pts',(-48.7835507278465,20.5422448076096,18.0221667953519));
#33901=CARTESIAN_POINT('Ctrl Pts',(-46.1157541596014,20.4047755971079,19.1638130647008));
#33902=CARTESIAN_POINT('Ctrl Pts',(-42.0278763659724,20.225761668211,20.420052715765));
#33903=CARTESIAN_POINT('Ctrl Pts',(-37.1961968561338,20.0475517349526,21.3635952152001));
#33904=CARTESIAN_POINT('Ctrl Pts',(-32.3340808857814,19.9048724048602,21.6673350763271));
#33905=CARTESIAN_POINT('Ctrl Pts',(-27.5131912254386,19.790507905872,21.3506809605032));
#33906=CARTESIAN_POINT('Ctrl Pts',(-22.7635395442217,19.6935273080542,20.5482405652461));
#33907=CARTESIAN_POINT('Ctrl Pts',(-18.1507531781766,19.6110850660289,19.1518448697928));
#33908=CARTESIAN_POINT('Ctrl Pts',(-13.746490413364,19.530779076001,17.18184705429));
#33909=CARTESIAN_POINT('Ctrl Pts',(-10.1470937090947,19.4573327991495,15.1094559205455));
#33910=CARTESIAN_POINT('Ctrl Pts',(-7.88638509780635,19.4012238336331,13.4783919538666));
#33911=CARTESIAN_POINT('Ctrl Pts',(-6.45016872863384,19.3605693891818,12.3240081054347));
#33912=CARTESIAN_POINT('Ctrl Pts',(-6.10927013923073,19.3505226070412,12.0406358031095));
#33913=CARTESIAN_POINT('Ctrl Pts',(-5.77357313580776,19.3402634731691,11.7521626271329));
#33914=CARTESIAN_POINT('Ctrl Pts',(-52.4105767042207,21.117312799858,15.3299514418919));
#33915=CARTESIAN_POINT('Ctrl Pts',(-52.016860569711,21.0964267127388,15.5492448456817));
#33916=CARTESIAN_POINT('Ctrl Pts',(-51.6182931914354,21.0758020890032,15.7628245248212));
#33917=CARTESIAN_POINT('Ctrl Pts',(-49.9021313977145,20.9891913310095,16.6465912195786));
#33918=CARTESIAN_POINT('Ctrl Pts',(-47.2337840991246,20.8653273744228,17.8442101454984));
#33919=CARTESIAN_POINT('Ctrl Pts',(-43.1354771375862,20.7063681300896,19.1850388218609));
#33920=CARTESIAN_POINT('Ctrl Pts',(-38.280340820171,20.5515335415639,20.2269975195059));
#33921=CARTESIAN_POINT('Ctrl Pts',(-33.3805535763787,20.4326519806542,20.6275542276719));
#33922=CARTESIAN_POINT('Ctrl Pts',(-28.5076379384233,20.3430531321453,20.4042206960657));
#33923=CARTESIAN_POINT('Ctrl Pts',(-23.6944093857262,20.2718184169426,19.6912911988527));
#33924=CARTESIAN_POINT('Ctrl Pts',(-19.0035276350953,20.2165549432469,18.3783788785326));
#33925=CARTESIAN_POINT('Ctrl Pts',(-14.5065432410363,20.164982094833,16.4839472490078));
#33926=CARTESIAN_POINT('Ctrl Pts',(-10.8175964077287,20.117197691553,14.4700412096342));
#33927=CARTESIAN_POINT('Ctrl Pts',(-8.49044235789128,20.0788282397779,12.8732097710812));
#33928=CARTESIAN_POINT('Ctrl Pts',(-7.00822822710744,20.0500302875854,11.739623233971));
#33929=CARTESIAN_POINT('Ctrl Pts',(-6.65615891828568,20.0428451797642,11.4611482226922));
#33930=CARTESIAN_POINT('Ctrl Pts',(-6.30920577514685,20.0354515632684,11.1774559872003));
#33931=CARTESIAN_POINT('Ctrl Pts',(-52.7278698567105,21.2334813897109,14.9235928820212));
#33932=CARTESIAN_POINT('Ctrl Pts',(-52.3343225101278,21.2132228077857,15.1452703485296));
#33933=CARTESIAN_POINT('Ctrl Pts',(-51.9358984377363,21.1932283095702,15.36124888794));
#33934=CARTESIAN_POINT('Ctrl Pts',(-50.2202359374443,21.1093059289188,16.2552855690169));
#33935=CARTESIAN_POINT('Ctrl Pts',(-47.5517532779547,20.9894835119608,17.4687550424721));
#33936=CARTESIAN_POINT('Ctrl Pts',(-43.4505266608392,20.8364792943525,18.8335283196105));
#33937=CARTESIAN_POINT('Ctrl Pts',(-38.5887936562049,20.6885792302246,19.9033309706188));
#33938=CARTESIAN_POINT('Ctrl Pts',(-33.6783987418936,20.5767478260626,20.3312569091985));
#33939=CARTESIAN_POINT('Ctrl Pts',(-28.7908305503325,20.4944756050622,20.1342769298014));
#33940=CARTESIAN_POINT('Ctrl Pts',(-23.9597012807767,20.4308554028779,19.4465967898802));
#33941=CARTESIAN_POINT('Ctrl Pts',(-19.2468366897852,20.3836340081555,18.1571940901283));
#33942=CARTESIAN_POINT('Ctrl Pts',(-14.7237552627977,20.340580727313,16.2839937133523));
#33943=CARTESIAN_POINT('Ctrl Pts',(-11.0096023037979,20.3004356869138,14.2864756931423));
#33944=CARTESIAN_POINT('Ctrl Pts',(-8.66373522866924,20.2673681898868,12.6992039590105));
#33945=CARTESIAN_POINT('Ctrl Pts',(-7.16856047765098,20.2421246596599,11.5714116141598));
#33946=CARTESIAN_POINT('Ctrl Pts',(-6.81334606473223,20.2357981340653,11.2943015263024));
#33947=CARTESIAN_POINT('Ctrl Pts',(-6.46322607776776,20.2292648564311,11.0119422811286));
#33948=CARTESIAN_POINT('Ctrl Pts',(-53.0460482247937,21.3428689572265,14.5160304606263));
#33949=CARTESIAN_POINT('Ctrl Pts',(-52.6526722617868,21.323266505305,14.7400892699525));
#33950=CARTESIAN_POINT('Ctrl Pts',(-52.2543941113152,21.303930781031,14.9584636434814));
#33951=CARTESIAN_POINT('Ctrl Pts',(-50.5392422512964,21.2228186866547,15.862756102697));
#33952=CARTESIAN_POINT('Ctrl Pts',(-47.870642759627,21.1072213437662,17.0920520597779));
#33953=CARTESIAN_POINT('Ctrl Pts',(-43.7665309694762,20.9604400919523,18.4807247967744));
#33954=CARTESIAN_POINT('Ctrl Pts',(-38.8982526035527,20.819779963638,19.5783050883969));
#33955=CARTESIAN_POINT('Ctrl Pts',(-33.9773212172862,20.7152993064879,20.0335139845838));
#33956=CARTESIAN_POINT('Ctrl Pts',(-29.075197419158,20.6406553883908,19.8627783242788));
#33957=CARTESIAN_POINT('Ctrl Pts',(-24.226291838715,20.5849601975755,19.2002153983462));
#33958=CARTESIAN_POINT('Ctrl Pts',(-19.4916041416705,20.5461109852346,17.9341609933042));
#33959=CARTESIAN_POINT('Ctrl Pts',(-14.9426199184388,20.5119420676311,16.0819985993253));
#33960=CARTESIAN_POINT('Ctrl Pts',(-11.2034485633272,20.4797911688045,14.1006759877594));
#33961=CARTESIAN_POINT('Ctrl Pts',(-8.83899898851629,20.4522911786996,12.5228195121512));
#33962=CARTESIAN_POINT('Ctrl Pts',(-7.33094843090817,20.4307901345004,11.4007202313913));
#33963=CARTESIAN_POINT('Ctrl Pts',(-6.97261113714822,20.4253683033402,11.1249514482168));
#33964=CARTESIAN_POINT('Ctrl Pts',(-6.61934824302656,20.4197421663948,10.8439022877958));
#33965=CARTESIAN_POINT('',(-42.6061719181885,20.5529756002067,19.5442896711374));
#33966=CARTESIAN_POINT('Ctrl Pts',(-19.7766131277702,-3.27137127985417,
42.4988381903824));
#33967=CARTESIAN_POINT('Ctrl Pts',(-23.5152967093788,1.76302065360711,40.7590604194676));
#33968=CARTESIAN_POINT('Ctrl Pts',(-28.0269925336501,6.26298702224561,38.031741717945));
#33969=CARTESIAN_POINT('Ctrl Pts',(-34.3755322884386,12.51884027248,31.997404897986));
#33970=CARTESIAN_POINT('Ctrl Pts',(-36.3604480222897,14.4577038717082,29.7410619772352));
#33971=CARTESIAN_POINT('Ctrl Pts',(-39.8066816790496,17.8486390891638,24.9184712381644));
#33972=CARTESIAN_POINT('Ctrl Pts',(-41.3278638860567,19.3555621054309,22.33097742788));
#33973=CARTESIAN_POINT('Ctrl Pts',(-42.6061719181886,20.5529756002057,19.544289671137));
#33974=CARTESIAN_POINT('Ctrl Pts',(-13.0430026535592,19.9464420456703,15.9970821676198));
#33975=CARTESIAN_POINT('Ctrl Pts',(-17.5281049508455,20.0189549105364,18.3838569009211));
#33976=CARTESIAN_POINT('Ctrl Pts',(-22.4637387366771,20.0954766247834,19.8995121675166));
#33977=CARTESIAN_POINT('Ctrl Pts',(-32.54594053874,20.2752040736289,21.1067813092147));
#33978=CARTESIAN_POINT('Ctrl Pts',(-37.6925271019862,20.3824974081049,20.8003325400241));
#33979=CARTESIAN_POINT('Ctrl Pts',(-42.6061719181885,20.5529756002056,19.5442896711373));
#33980=CARTESIAN_POINT('Ctrl Pts',(-51.3108334676861,20.9435908393615,16.1511536729868));
#33981=CARTESIAN_POINT('Ctrl Pts',(-51.1733425720729,20.9358615047579,16.2234493647249));
#33982=CARTESIAN_POINT('Ctrl Pts',(-51.0358516764597,20.9281321701544,16.295745056463));
#33983=CARTESIAN_POINT('Ctrl Pts',(-50.8983607808465,20.9204028355509,16.3680407482011));
#33984=CARTESIAN_POINT('Ctrl Pts',(-37.1492712195272,20.1474693751975,23.5976099220123));
#33985=CARTESIAN_POINT('Ctrl Pts',(-19.3601378042676,20.0812550388979,21.8299835873915));
#33986=CARTESIAN_POINT('Ctrl Pts',(-7.20423930084636,19.8399463130827,12.1777561381709));
#33987=CARTESIAN_POINT('Ctrl Pts',(-51.3107798237275,20.9469886892296,16.1512322048296));
#33988=CARTESIAN_POINT('Ctrl Pts',(-51.1732906434227,20.9392720585054,16.2235357813434));
#33989=CARTESIAN_POINT('Ctrl Pts',(-51.0358014631179,20.9315554277811,16.2958393578572));
#33990=CARTESIAN_POINT('Ctrl Pts',(-50.8983122828131,20.9238387970569,16.368142934371));
#33991=CARTESIAN_POINT('Ctrl Pts',(-37.149394252333,20.1521757246323,23.5985005857523));
#33992=CARTESIAN_POINT('Ctrl Pts',(-19.3601421168584,20.0873688943554,21.8304317652129));
#33993=CARTESIAN_POINT('Ctrl Pts',(-7.20415446045915,19.8474084919615,12.1784397513226));
#33994=CARTESIAN_POINT('Ctrl Pts',(-51.310726179769,20.9503865390978,16.1513107366724));
#33995=CARTESIAN_POINT('Ctrl Pts',(-51.1732387147725,20.9426826122528,16.2236221979619));
#33996=CARTESIAN_POINT('Ctrl Pts',(-51.0357512497761,20.9349786854078,16.2959336592514));
#33997=CARTESIAN_POINT('Ctrl Pts',(-50.8982637847797,20.9272747585629,16.3682451205409));
#33998=CARTESIAN_POINT('Ctrl Pts',(-37.1495172851389,20.1568820740671,23.5993912494923));
#33999=CARTESIAN_POINT('Ctrl Pts',(-19.3601464294492,20.093482749813,21.8308799430342));
#34000=CARTESIAN_POINT('Ctrl Pts',(-7.20406962007193,19.8548706708402,12.1791233644742));
#34001=CARTESIAN_POINT('Ctrl Pts',(-51.3106725358104,20.9537843889659,16.1513892685152));
#34002=CARTESIAN_POINT('Ctrl Pts',(-51.1731867861224,20.9460931660003,16.2237086145804));
#34003=CARTESIAN_POINT('Ctrl Pts',(-51.0357010364343,20.9384019430346,16.2960279606456));
#34004=CARTESIAN_POINT('Ctrl Pts',(-50.8982152867463,20.9307107200689,16.3683473067109));
#34005=CARTESIAN_POINT('Ctrl Pts',(-37.1496403179447,20.1615884235019,23.6002819132323));
#34006=CARTESIAN_POINT('Ctrl Pts',(-19.36015074204,20.0995966052706,21.8313281208555));
#34007=CARTESIAN_POINT('Ctrl Pts',(-7.20398477968471,19.862332849719,12.1798069776258));
#34008=CARTESIAN_POINT('Ctrl Pts',(-51.3105096332532,20.9641027630587,16.1516277490143));
#34009=CARTESIAN_POINT('Ctrl Pts',(-51.1730290925045,20.9564501184246,16.2239710390642));
#34010=CARTESIAN_POINT('Ctrl Pts',(-51.0355485517558,20.9487974737906,16.2963143291142));
#34011=CARTESIAN_POINT('Ctrl Pts',(-50.898068011007,20.9411448291565,16.3686576191641));
#34012=CARTESIAN_POINT('Ctrl Pts',(-37.1500139361344,20.1758803657488,23.6029866241575));
#34013=CARTESIAN_POINT('Ctrl Pts',(-19.360163838241,20.1181627721728,21.8326891187219));
#34014=CARTESIAN_POINT('Ctrl Pts',(-7.20372714179975,19.8849935193208,12.1818829305098));
#34015=CARTESIAN_POINT('Ctrl Pts',(-51.3101838278559,20.9847395112521,16.1521047099983));
#34016=CARTESIAN_POINT('Ctrl Pts',(-51.1727137050801,20.9771640232786,16.2244958880224));
#34017=CARTESIAN_POINT('Ctrl Pts',(-51.0352435823044,20.9695885353052,16.2968870660465));
#34018=CARTESIAN_POINT('Ctrl Pts',(-50.8977734595286,20.9620130473318,16.3692782440705));
#34019=CARTESIAN_POINT('Ctrl Pts',(-37.1507611819551,20.2044642499886,23.6083960464791));
#34020=CARTESIAN_POINT('Ctrl Pts',(-19.3601900256785,20.1552951062578,21.8354111160267));
#34021=CARTESIAN_POINT('Ctrl Pts',(-7.20321186602976,19.9303148585245,12.1860348362777));
#34022=CARTESIAN_POINT('Ctrl Pts',(-51.3096951007816,21.0156946339229,16.1528201510927));
#34023=CARTESIAN_POINT('Ctrl Pts',(-51.1722406112913,21.0082348808134,16.2252831612052));
#34024=CARTESIAN_POINT('Ctrl Pts',(-51.034786121801,21.000775127704,16.2977461713177));
#34025=CARTESIAN_POINT('Ctrl Pts',(-50.8973316323108,20.9933153745945,16.3702091814302));
#34026=CARTESIAN_POINT('Ctrl Pts',(-37.151882683285,20.2473400636495,23.616510192681));
#34027=CARTESIAN_POINT('Ctrl Pts',(-19.3602290009807,20.2109936225946,21.8394942155879));
#34028=CARTESIAN_POINT('Ctrl Pts',(-7.20243895237484,19.9982968673298,12.1922626949296));
#34029=CARTESIAN_POINT('Ctrl Pts',(-51.3092063487451,21.0466497571015,16.1535355916576));
#34030=CARTESIAN_POINT('Ctrl Pts',(-51.1717675008611,21.0393057386868,16.226070434035));
#34031=CARTESIAN_POINT('Ctrl Pts',(-51.0343286529771,21.0319617202721,16.2986052764125));
#34032=CARTESIAN_POINT('Ctrl Pts',(-50.8968898050931,21.0246177018574,16.3711401187899));
#34033=CARTESIAN_POINT('Ctrl Pts',(-37.1530050166935,20.2902158603888,23.6246243565344));
#34034=CARTESIAN_POINT('Ctrl Pts',(-19.3602675711725,20.2666921589687,21.8435774500921));
#34035=CARTESIAN_POINT('Ctrl Pts',(-7.20166603871989,20.0662788761352,12.1984905535815));
#34036=CARTESIAN_POINT('Ctrl Pts',(-51.3088805014622,21.0672865061488,16.1540125517431));
#34037=CARTESIAN_POINT('Ctrl Pts',(-51.171452085513,21.0600196441101,16.2265952823942));
#34038=CARTESIAN_POINT('Ctrl Pts',(-51.0340236695638,21.0527527820714,16.2991780130453));
#34039=CARTESIAN_POINT('Ctrl Pts',(-50.8965952536146,21.0454859200326,16.3717607436964));
#34040=CARTESIAN_POINT('Ctrl Pts',(-37.1537536586921,20.3187997161584,23.6300338088058));
#34041=CARTESIAN_POINT('Ctrl Pts',(-19.3602930783192,20.3038245267329,21.8462996737943));
#34042=CARTESIAN_POINT('Ctrl Pts',(-7.20115076294994,20.1116002153389,12.2026424593494));
#34043=CARTESIAN_POINT('Ctrl Pts',(-51.3087175776821,21.0776048806767,16.154251031777));
#34044=CARTESIAN_POINT('Ctrl Pts',(-51.1712943777465,21.0703765968246,16.2268577065679));
#34045=CARTESIAN_POINT('Ctrl Pts',(-51.0338711778109,21.0631483129724,16.2994643813587));
#34046=CARTESIAN_POINT('Ctrl Pts',(-50.8964479778753,21.0559200291202,16.3720710561496));
#34047=CARTESIAN_POINT('Ctrl Pts',(-37.1541279843181,20.3330916439037,23.6327385352381));
#34048=CARTESIAN_POINT('Ctrl Pts',(-19.3603058292958,20.3223907107576,21.847660786348));
#34049=CARTESIAN_POINT('Ctrl Pts',(-7.20089312506496,20.1342608849406,12.2047184122334));
#34050=CARTESIAN_POINT('Ctrl Pts',(-51.3087018783124,21.0785991614118,16.1542740117631));
#34051=CARTESIAN_POINT('Ctrl Pts',(-51.171279180993,21.0713745949617,16.2268829938163));
#34052=CARTESIAN_POINT('Ctrl Pts',(-51.0338564836736,21.0641500285117,16.2994919758695));
#34053=CARTESIAN_POINT('Ctrl Pts',(-50.8964337863542,21.0569254620617,16.3721009579227));
#34054=CARTESIAN_POINT('Ctrl Pts',(-37.154164054414,20.3344688170607,23.6329991632448));
#34055=CARTESIAN_POINT('Ctrl Pts',(-19.3603070579826,20.3241797521467,21.8477919434393));
#34056=CARTESIAN_POINT('Ctrl Pts',(-7.20086829902429,20.1364444718193,12.204918451489));
#34057=CARTESIAN_POINT('Ctrl Pts',(-51.3086861789428,21.0795934421468,16.1542969917492));
#34058=CARTESIAN_POINT('Ctrl Pts',(-51.1712639842395,21.0723725930989,16.2269082810647));
#34059=CARTESIAN_POINT('Ctrl Pts',(-51.0338417895363,21.0651517440511,16.2995195703803));
#34060=CARTESIAN_POINT('Ctrl Pts',(-50.8964195948331,21.0579308950032,16.3721308596959));
#34061=CARTESIAN_POINT('Ctrl Pts',(-37.1542001245098,20.3358459902176,23.6332597912515));
#34062=CARTESIAN_POINT('Ctrl Pts',(-19.3603082866694,20.3259687935359,21.8479231005306));
#34063=CARTESIAN_POINT('Ctrl Pts',(-7.20084347298362,20.1386280586979,12.2051184907446));
#34064=CARTESIAN_POINT('Ctrl Pts',(-51.3086704795731,21.0805877228818,16.1543199717353));
#34065=CARTESIAN_POINT('Ctrl Pts',(-51.171248787486,21.0733705912361,16.2269335683132));
#34066=CARTESIAN_POINT('Ctrl Pts',(-51.033827095399,21.0661534595904,16.2995471648911));
#34067=CARTESIAN_POINT('Ctrl Pts',(-50.8964054033119,21.0589363279447,16.372160761469));
#34068=CARTESIAN_POINT('Ctrl Pts',(-37.1542361946057,20.3372231633746,23.6335204192581));
#34069=CARTESIAN_POINT('Ctrl Pts',(-19.3603095153562,20.327757834925,21.848054257622));
#34070=CARTESIAN_POINT('Ctrl Pts',(-7.20081864694295,20.1408116455766,12.2053185300001));
#34071=CARTESIAN_POINT('',(-42.6061719181885,20.5529756002067,19.5442896711374));
#34072=CARTESIAN_POINT('Ctrl Pts',(-44.4073194910718,21.2883239772394,-32.4663123587466));
#34073=CARTESIAN_POINT('Ctrl Pts',(-44.3383146796219,21.2711623310641,-32.0212557620871));
#34074=CARTESIAN_POINT('Ctrl Pts',(-44.261863066907,21.2542807820542,-31.5759157513107));
#34075=CARTESIAN_POINT('Ctrl Pts',(-43.9035132676456,21.1834525291307,-29.6749230164548));
#34076=CARTESIAN_POINT('Ctrl Pts',(-43.2061630172825,21.0834264338425,-26.8247770659076));
#34077=CARTESIAN_POINT('Ctrl Pts',(-41.7401377983077,20.9598507183575,-22.7530174393195));
#34078=CARTESIAN_POINT('Ctrl Pts',(-39.5700058445959,20.8461335954997,-18.2644080598691));
#34079=CARTESIAN_POINT('Ctrl Pts',(-36.8630486192783,20.7684839093916,-14.133595467843));
#34080=CARTESIAN_POINT('Ctrl Pts',(-33.6763829202324,20.7206230093664,-10.4064236844732));
#34081=CARTESIAN_POINT('Ctrl Pts',(-30.1365835892634,20.6916936542703,-7.02655419472538));
#34082=CARTESIAN_POINT('Ctrl Pts',(-26.1937522215189,20.6796111419738,-4.11120263465573));
#34083=CARTESIAN_POINT('Ctrl Pts',(-21.9057871986473,20.6722203558656,-1.70562443471912));
#34084=CARTESIAN_POINT('Ctrl Pts',(-18.0203164619706,20.6630225594897,-0.0137786889588934));
#34085=CARTESIAN_POINT('Ctrl Pts',(-15.3077264292458,20.6508204531822,0.853827525762252));
#34086=CARTESIAN_POINT('Ctrl Pts',(-13.4888993727121,20.6394053700742,1.33453354362263));
#34087=CARTESIAN_POINT('Ctrl Pts',(-13.0513753202763,20.6364191357732,1.44265992605398));
#34088=CARTESIAN_POINT('Ctrl Pts',(-12.6129206067808,20.6332209087108,1.54359234992982));
#34089=CARTESIAN_POINT('Ctrl Pts',(-44.5317392944723,21.2398788304839,-31.9470607245409));
#34090=CARTESIAN_POINT('Ctrl Pts',(-44.4608008352633,21.2217224127637,-31.5033401695429));
#34091=CARTESIAN_POINT('Ctrl Pts',(-44.3824197147887,21.2038412173392,-31.0593641751136));
#34092=CARTESIAN_POINT('Ctrl Pts',(-44.0158544499838,21.1287309618461,-29.1643130978913));
#34093=CARTESIAN_POINT('Ctrl Pts',(-43.3063638359009,21.0222253289507,-26.3240464492741));
#34094=CARTESIAN_POINT('Ctrl Pts',(-41.8236544645841,20.8890564489947,-22.2693004510702));
#34095=CARTESIAN_POINT('Ctrl Pts',(-39.6360777463142,20.7641817659416,-17.802927976306));
#34096=CARTESIAN_POINT('Ctrl Pts',(-36.9144982085081,20.6752847595175,-13.6971173002781));
#34097=CARTESIAN_POINT('Ctrl Pts',(-33.7164751020028,20.6159219251614,-9.99738737870817));
#34098=CARTESIAN_POINT('Ctrl Pts',(-30.1681646940186,20.5752144761384,-6.64672745320853));
#34099=CARTESIAN_POINT('Ctrl Pts',(-26.2206730087597,20.5509334123338,-3.76258061545188));
#34100=CARTESIAN_POINT('Ctrl Pts',(-21.9323370596648,20.5308579865904,-1.38988250425128));
#34101=CARTESIAN_POINT('Ctrl Pts',(-18.0496957203779,20.510426256151,0.272782902906163));
#34102=CARTESIAN_POINT('Ctrl Pts',(-15.3412263850242,20.4905046142392,1.12035027642913));
#34103=CARTESIAN_POINT('Ctrl Pts',(-13.5258914774281,20.4739374093561,1.58770978327916));
#34104=CARTESIAN_POINT('Ctrl Pts',(-13.0892415042887,20.469713411733,1.69263748736944));
#34105=CARTESIAN_POINT('Ctrl Pts',(-12.6516971675958,20.4652767483487,1.79037613603859));
#34106=CARTESIAN_POINT('Ctrl Pts',(-44.6561524410473,21.1822016013635,-31.4275844698422));
#34107=CARTESIAN_POINT('Ctrl Pts',(-44.5832693071228,21.1630886105529,-30.9852161369667));
#34108=CARTESIAN_POINT('Ctrl Pts',(-44.5029476284026,21.1442460408093,-30.5426209641973));
#34109=CARTESIAN_POINT('Ctrl Pts',(-44.1281197536622,21.0650173413637,-28.6535860555276));
#34110=CARTESIAN_POINT('Ctrl Pts',(-43.4064198561525,20.9522796229575,-25.8233136742122));
#34111=CARTESIAN_POINT('Ctrl Pts',(-41.9069320566516,20.8098799445818,-21.7857609610574));
#34112=CARTESIAN_POINT('Ctrl Pts',(-39.701810753245,20.6742608619688,-17.3418485850746));
#34113=CARTESIAN_POINT('Ctrl Pts',(-36.9655218819498,20.5745198093833,-13.2612876234125));
#34114=CARTESIAN_POINT('Ctrl Pts',(-33.7560682522845,20.5040526001987,-9.58928002469061));
#34115=CARTESIAN_POINT('Ctrl Pts',(-30.1991853983857,20.4519664047462,-6.26814546563906));
#34116=CARTESIAN_POINT('Ctrl Pts',(-26.2469871598986,20.4158956934967,-3.4155667301831));
#34117=CARTESIAN_POINT('Ctrl Pts',(-21.9582479010102,20.3835681705302,-1.07616408222921));
#34118=CARTESIAN_POINT('Ctrl Pts',(-18.0784131832276,20.3523071857454,0.55692401639258));
#34119=CARTESIAN_POINT('Ctrl Pts',(-15.3740496198733,20.3249607749065,1.38416737993585));
#34120=CARTESIAN_POINT('Ctrl Pts',(-13.5621950244834,20.3034475984546,1.83798684151568));
#34121=CARTESIAN_POINT('Ctrl Pts',(-13.126418050243,20.2980359714688,1.93966838129505));
#34122=CARTESIAN_POINT('Ctrl Pts',(-12.6897847127264,20.29241155197,2.03416478777318));
#34123=CARTESIAN_POINT('Ctrl Pts',(-45.1007065738908,20.942701117012,-29.5703976932599));
#34124=CARTESIAN_POINT('Ctrl Pts',(-45.0208376113571,20.9203083949833,-29.1329175650445));
#34125=CARTESIAN_POINT('Ctrl Pts',(-44.9335441184161,20.898168919688,-28.6953160815928));
#34126=CARTESIAN_POINT('Ctrl Pts',(-44.5290285228739,20.8048139743737,-26.8280477231251));
#34127=CARTESIAN_POINT('Ctrl Pts',(-43.7634624578871,20.6706999592586,-24.0339034229851));
#34128=CARTESIAN_POINT('Ctrl Pts',(-42.2036921823277,20.496623371127,-20.0584390264519));
#34129=CARTESIAN_POINT('Ctrl Pts',(-39.9355295569025,20.3241023157428,-15.6955948544318));
#34130=CARTESIAN_POINT('Ctrl Pts',(-37.1463732008804,20.1870685788371,-11.7061626846798));
#34131=CARTESIAN_POINT('Ctrl Pts',(-33.8958149948604,20.0783595881962,-8.13424084429036));
#34132=CARTESIAN_POINT('Ctrl Pts',(-30.3080800546265,19.9870599496472,-4.91976504399102));
#34133=CARTESIAN_POINT('Ctrl Pts',(-26.338894511269,19.9103458023656,-2.1813190929775));
#34134=CARTESIAN_POINT('Ctrl Pts',(-22.0485898350668,19.8358125374395,0.0375894018033821));
#34135=CARTESIAN_POINT('Ctrl Pts',(-18.1786911029417,19.767331746443,1.56354030718519));
#34136=CARTESIAN_POINT('Ctrl Pts',(-15.4889340993771,19.7145309927478,2.31712214152166));
#34137=CARTESIAN_POINT('Ctrl Pts',(-13.6894644921416,19.6760973304852,2.72185635616174));
#34138=CARTESIAN_POINT('Ctrl Pts',(-13.2568036731226,19.6666248028076,2.81176456048477));
#34139=CARTESIAN_POINT('Ctrl Pts',(-12.8234309753936,19.6569408091057,2.89449675536615));
#34140=CARTESIAN_POINT('Ctrl Pts',(-45.7331411798393,20.4780024533914,-26.9246386002418));
#34141=CARTESIAN_POINT('Ctrl Pts',(-45.643195587219,20.4514551579611,-26.4943263387457));
#34142=CARTESIAN_POINT('Ctrl Pts',(-45.545843383721,20.4251375618498,-26.0640525529226));
#34143=CARTESIAN_POINT('Ctrl Pts',(-45.0984865809081,20.3138746691076,-24.2287465356082));
#34144=CARTESIAN_POINT('Ctrl Pts',(-44.2696195687612,20.1526659052326,-21.4875728962292));
#34145=CARTESIAN_POINT('Ctrl Pts',(-42.6228530658995,19.938389785095,-17.602943244611));
#34146=CARTESIAN_POINT('Ctrl Pts',(-40.2636965799363,19.7189203495023,-13.3585242566371));
#34147=CARTESIAN_POINT('Ctrl Pts',(-37.3981974853228,19.5342279169114,-9.50204543905061));
#34148=CARTESIAN_POINT('Ctrl Pts',(-34.0882248338531,19.3763677050182,-6.07603571246518));
#34149=CARTESIAN_POINT('Ctrl Pts',(-30.4558249347077,19.2344308170631,-3.01699581468252));
#34150=CARTESIAN_POINT('Ctrl Pts',(-26.4619147472141,19.1049298841923,-0.444834180453594));
#34151=CARTESIAN_POINT('Ctrl Pts',(-22.1690568663997,18.9752993129734,1.5985252972521));
#34152=CARTESIAN_POINT('Ctrl Pts',(-18.313179789766,18.8580619466085,2.96837222878708));
#34153=CARTESIAN_POINT('Ctrl Pts',(-15.6442421074702,18.7718242877839,3.61460478820385));
#34154=CARTESIAN_POINT('Ctrl Pts',(-13.8624572105756,18.7111415689428,3.94779507422417));
#34155=CARTESIAN_POINT('Ctrl Pts',(-13.4342661174466,18.6963263828107,4.02053340451179));
#34156=CARTESIAN_POINT('Ctrl Pts',(-13.0055894034835,18.6812985797984,4.0861000036974));
#34157=CARTESIAN_POINT('Ctrl Pts',(-46.6541128225086,19.4355555088431,-23.0630467354439));
#34158=CARTESIAN_POINT('Ctrl Pts',(-46.5490340460232,19.4044605226273,-22.643764115916));
#34159=CARTESIAN_POINT('Ctrl Pts',(-46.4365715773658,19.3735658358572,-22.2247785892071));
#34160=CARTESIAN_POINT('Ctrl Pts',(-45.924844384654,19.2426748194849,-20.4387653247907));
#34161=CARTESIAN_POINT('Ctrl Pts',(-45.0008677782111,19.0517849995255,-17.7791175023364));
#34162=CARTESIAN_POINT('Ctrl Pts',(-43.2233772399451,18.7933185397158,-14.0338870045424));
#34163=CARTESIAN_POINT('Ctrl Pts',(-40.7274520428515,18.5218580841843,-9.97086024600777));
#34164=CARTESIAN_POINT('Ctrl Pts',(-37.7471256337672,18.2836948825759,-6.3177091993364));
#34165=CARTESIAN_POINT('Ctrl Pts',(-34.3476493922282,18.0697821020849,-3.11466407912025));
#34166=CARTESIAN_POINT('Ctrl Pts',(-30.6477975764489,17.8693333343866,-0.293061415310591));
#34167=CARTESIAN_POINT('Ctrl Pts',(-26.6162332687096,17.6778661310593,2.02512214074259));
#34168=CARTESIAN_POINT('Ctrl Pts',(-22.318832751704,17.4826662284719,3.80028746637419));
#34169=CARTESIAN_POINT('Ctrl Pts',(-18.4832621351138,17.3068805329357,4.93156172800206));
#34170=CARTESIAN_POINT('Ctrl Pts',(-15.844982677665,17.1802068447994,5.4136492325017));
#34171=CARTESIAN_POINT('Ctrl Pts',(-14.0893175584168,17.0925519552341,5.63740721935216));
#34172=CARTESIAN_POINT('Ctrl Pts',(-13.6677806909122,17.0712544126695,5.68386420748927));
#34173=CARTESIAN_POINT('Ctrl Pts',(-13.2461444261988,17.0497370990139,5.72313897790732));
#34174=CARTESIAN_POINT('Ctrl Pts',(-47.6918456308501,17.8320672383652,-18.704111982361));
#34175=CARTESIAN_POINT('Ctrl Pts',(-47.5691196189588,17.7976045693245,-18.29788404473));
#34176=CARTESIAN_POINT('Ctrl Pts',(-47.4390324745029,17.7633163796081,-17.8922819113841));
#34177=CARTESIAN_POINT('Ctrl Pts',(-46.8522106122062,17.6178640028275,-16.1648079219532));
#34178=CARTESIAN_POINT('Ctrl Pts',(-45.817282089803,17.4049846203341,-13.6018689231232));
#34179=CARTESIAN_POINT('Ctrl Pts',(-43.887284691588,17.1135517229592,-10.0217467329179));
#34180=CARTESIAN_POINT('Ctrl Pts',(-41.231769853489,16.8027253827761,-6.17336527532705));
#34181=CARTESIAN_POINT('Ctrl Pts',(-38.1173880411078,16.523022337621,-2.76065836727235));
#34182=CARTESIAN_POINT('Ctrl Pts',(-34.6133006485321,16.2641978724915,0.178767788703479));
#34183=CARTESIAN_POINT('Ctrl Pts',(-30.8344657346569,16.0157341831644,2.71962576869524));
#34184=CARTESIAN_POINT('Ctrl Pts',(-26.7585353322669,15.7719994721116,4.73743033545191));
#34185=CARTESIAN_POINT('Ctrl Pts',(-22.4552167350297,15.5202180684676,6.19524316069885));
#34186=CARTESIAN_POINT('Ctrl Pts',(-18.6426662536523,15.2931736272884,7.04407111501189));
#34187=CARTESIAN_POINT('Ctrl Pts',(-16.0396032563085,15.130708702949,7.33170692760031));
#34188=CARTESIAN_POINT('Ctrl Pts',(-14.3140107263472,15.0190926843839,7.42578042231738));
#34189=CARTESIAN_POINT('Ctrl Pts',(-13.9002119764642,14.9920326361705,7.44107757524737));
#34190=CARTESIAN_POINT('Ctrl Pts',(-13.4868340937886,14.9647422323135,7.44916755087306));
#34191=CARTESIAN_POINT('Ctrl Pts',(-48.6780895578841,15.7638142683891,-14.5547709237334));
#34192=CARTESIAN_POINT('Ctrl Pts',(-48.5377569832782,15.7283726072843,-14.1616824700076));
#34193=CARTESIAN_POINT('Ctrl Pts',(-48.3900841939855,15.6930928161318,-13.7695776325575));
#34194=CARTESIAN_POINT('Ctrl Pts',(-47.7283337492943,15.543379415412,-12.1012573581504));
#34195=CARTESIAN_POINT('Ctrl Pts',(-46.5827035062241,15.3241289383934,-9.63600324480673));
#34196=CARTESIAN_POINT('Ctrl Pts',(-44.5005407430779,15.0227233638938,-6.22259713508827));
#34197=CARTESIAN_POINT('Ctrl Pts',(-41.6857715265693,14.6988957424381,-2.59094464376435));
#34198=CARTESIAN_POINT('Ctrl Pts',(-38.4375620143823,14.4035050799014,0.578927699610593));
#34199=CARTESIAN_POINT('Ctrl Pts',(-34.8289423387839,14.1252237593235,3.25197397062977));
#34200=CARTESIAN_POINT('Ctrl Pts',(-30.9710627511194,13.8539516979883,5.50899869421461));
#34201=CARTESIAN_POINT('Ctrl Pts',(-26.8505025711077,13.5829362127958,7.22288800531011));
#34202=CARTESIAN_POINT('Ctrl Pts',(-22.5407609566498,13.2994842764397,8.35930998893307));
#34203=CARTESIAN_POINT('Ctrl Pts',(-18.7506147783617,13.0425486753816,8.92186191214317));
#34204=CARTESIAN_POINT('Ctrl Pts',(-16.1822241576763,12.8585920936854,9.01223170778387));
#34205=CARTESIAN_POINT('Ctrl Pts',(-14.4862987055291,12.7324540777387,8.97467844460437));
#34206=CARTESIAN_POINT('Ctrl Pts',(-14.0802223991229,12.7018988467546,8.95834926449915));
#34207=CARTESIAN_POINT('Ctrl Pts',(-13.6751669748553,12.6711030837425,8.93478984019534));
#34208=CARTESIAN_POINT('Ctrl Pts',(-49.6043543370422,13.2592937677246,-10.6555406574459));
#34209=CARTESIAN_POINT('Ctrl Pts',(-49.4465065543946,13.2252177231213,-10.2754480399043));
#34210=CARTESIAN_POINT('Ctrl Pts',(-49.281340174109,13.191306123502,-9.89672252517936));
#34211=CARTESIAN_POINT('Ctrl Pts',(-48.5450641799685,13.0474600457288,-8.2871658783874));
#34212=CARTESIAN_POINT('Ctrl Pts',(-47.2893340185595,12.8372075593629,-5.91905480535809));
#34213=CARTESIAN_POINT('Ctrl Pts',(-45.0558433901964,12.5484949329477,-2.6717513794037));
#34214=CARTESIAN_POINT('Ctrl Pts',(-42.0826999038725,12.2377054846042,0.7436212820901));
#34215=CARTESIAN_POINT('Ctrl Pts',(-38.7013965992381,11.9522310106351,3.67073641417757));
#34216=CARTESIAN_POINT('Ctrl Pts',(-34.9887969057865,11.6797819251771,6.0770574947467));
#34217=CARTESIAN_POINT('Ctrl Pts',(-31.0522615890383,11.4108111467242,8.04954156774515));
#34218=CARTESIAN_POINT('Ctrl Pts',(-26.887234235299,11.1374939458242,9.45832687893132));
#34219=CARTESIAN_POINT('Ctrl Pts',(-22.5709739096369,10.8473681096278,10.2716488305119));
#34220=CARTESIAN_POINT('Ctrl Pts',(-18.8029589072629,10.5820480444149,10.5460864286058));
#34221=CARTESIAN_POINT('Ctrl Pts',(-16.2689222255049,10.3910369789073,10.4377055494679));
#34222=CARTESIAN_POINT('Ctrl Pts',(-14.6024067670471,10.2599216927486,10.267460566929));
#34223=CARTESIAN_POINT('Ctrl Pts',(-14.2040678125169,10.2281653805015,10.2192687273159));
#34224=CARTESIAN_POINT('Ctrl Pts',(-13.8074239840703,10.1961599190035,10.1638445143716));
#34225=CARTESIAN_POINT('Ctrl Pts',(-50.4780231898425,10.420684636249,-6.97825636524223));
#34226=CARTESIAN_POINT('Ctrl Pts',(-50.3027554822726,10.3898269637342,-6.61091292266229));
#34227=CARTESIAN_POINT('Ctrl Pts',(-50.1201946638507,10.3591499865554,-6.24534398850934));
#34228=CARTESIAN_POINT('Ctrl Pts',(-49.3098403704687,10.2291883131935,-4.69370522484957));
#34229=CARTESIAN_POINT('Ctrl Pts',(-47.9446771541553,10.0401067219452,-2.42149658251557));
#34230=CARTESIAN_POINT('Ctrl Pts',(-45.5607908677836,9.78206378055234,0.661378115659448));
#34231=CARTESIAN_POINT('Ctrl Pts',(-42.4302660676023,9.50499638561923,3.86218206511734));
#34232=CARTESIAN_POINT('Ctrl Pts',(-38.9167256658903,9.24981780003299,6.5479222446764));
#34233=CARTESIAN_POINT('Ctrl Pts',(-35.1008412689809,9.00337535985762,8.68853775633541));
#34234=CARTESIAN_POINT('Ctrl Pts',(-31.0862039090992,8.75677479408939,10.3771954877894));
#34235=CARTESIAN_POINT('Ctrl Pts',(-26.8770707252232,8.50116890088297,11.4811916028238));
#34236=CARTESIAN_POINT('Ctrl Pts',(-22.5544391822955,8.22444592813344,11.9713059613016));
#34237=CARTESIAN_POINT('Ctrl Pts',(-18.8085260012426,7.96804930448713,11.95723852036));
#34238=CARTESIAN_POINT('Ctrl Pts',(-16.3087141317035,7.78162503245108,11.6496422404835));
#34239=CARTESIAN_POINT('Ctrl Pts',(-14.6714860069479,7.65323614745839,11.3463312647337));
#34240=CARTESIAN_POINT('Ctrl Pts',(-14.2809216999101,7.62212996336316,11.266226142876));
#34241=CARTESIAN_POINT('Ctrl Pts',(-13.8927906386079,7.59076668565169,11.1789266563201));
#34242=CARTESIAN_POINT('Ctrl Pts',(-51.2801101945885,7.18298363715391,-3.6058167721169));
#34243=CARTESIAN_POINT('Ctrl Pts',(-51.0875784709456,7.15763661423686,-3.25078129070187));
#34244=CARTESIAN_POINT('Ctrl Pts',(-50.887783992036,7.13250342173354,-2.89794609704175));
#34245=CARTESIAN_POINT('Ctrl Pts',(-50.0040661154971,7.02634360727853,-1.40250116902478));
#34246=CARTESIAN_POINT('Ctrl Pts',(-48.5305347456743,6.87350147707393,0.776364733400529));
#34247=CARTESIAN_POINT('Ctrl Pts',(-45.9977455159499,6.66841421880391,3.69838327624897));
#34248=CARTESIAN_POINT('Ctrl Pts',(-42.7114417935179,6.45075222930465,6.68844966589508));
#34249=CARTESIAN_POINT('Ctrl Pts',(-39.067072850966,6.25122984378583,9.13619723204205));
#34250=CARTESIAN_POINT('Ctrl Pts',(-35.1490911808322,6.05595707526583,11.0140071785515));
#34251=CARTESIAN_POINT('Ctrl Pts',(-31.0573490533695,5.8568061689083,12.4213387062058));
#34252=CARTESIAN_POINT('Ctrl Pts',(-26.8048536119047,5.64398234710963,13.2225300798875));
#34253=CARTESIAN_POINT('Ctrl Pts',(-22.476319035136,5.40587468584602,13.3908877176693));
#34254=CARTESIAN_POINT('Ctrl Pts',(-18.7527113449239,5.18017895256177,13.0891872008594));
#34255=CARTESIAN_POINT('Ctrl Pts',(-16.2871230511152,5.01301666232781,12.582706320691));
#34256=CARTESIAN_POINT('Ctrl Pts',(-14.6791349520876,4.89707445701614,12.1464642141551));
#34257=CARTESIAN_POINT('Ctrl Pts',(-14.2963869521683,4.86894780999335,12.0345319415383));
#34258=CARTESIAN_POINT('Ctrl Pts',(-13.9168603612279,4.84055053954568,11.9154972073634));
#34259=CARTESIAN_POINT('Ctrl Pts',(-52.0016295564212,3.57357815210241,-0.579903291299028));
#34260=CARTESIAN_POINT('Ctrl Pts',(-51.7920457954104,3.55599962931061,-0.236514691928469));
#34261=CARTESIAN_POINT('Ctrl Pts',(-51.5752339262503,3.53868515668548,0.104236780555091));
#34262=CARTESIAN_POINT('Ctrl Pts',(-50.6191007286354,3.46609807861293,1.54621396039117));
#34263=CARTESIAN_POINT('Ctrl Pts',(-49.0386135652145,3.36435917107101,3.63581403638429));
#34264=CARTESIAN_POINT('Ctrl Pts',(-46.3589071813945,3.23426720235262,6.40277838991865));
#34265=CARTESIAN_POINT('Ctrl Pts',(-42.9189723935365,3.10147907156715,9.1884915299686));
#34266=CARTESIAN_POINT('Ctrl Pts',(-39.1456956308945,2.98285053627008,11.4041304698817));
#34267=CARTESIAN_POINT('Ctrl Pts',(-35.1272894147124,2.86388130857434,13.024498250666));
#34268=CARTESIAN_POINT('Ctrl Pts',(-30.9599073841823,2.73730530568202,14.1554442054127));
#34269=CARTESIAN_POINT('Ctrl Pts',(-26.665243652355,2.59247375589619,14.6582371615255));
#34270=CARTESIAN_POINT('Ctrl Pts',(-22.3317156909432,2.41842603756845,14.5087087925182));
#34271=CARTESIAN_POINT('Ctrl Pts',(-18.6309936354684,2.24547053120763,13.9223283048296));
#34272=CARTESIAN_POINT('Ctrl Pts',(-16.1998803664798,2.11246131963295,13.2186916617235));
#34273=CARTESIAN_POINT('Ctrl Pts',(-14.6212528479762,2.01884144332686,12.6505786045591));
#34274=CARTESIAN_POINT('Ctrl Pts',(-14.2463818515635,1.99605339732081,12.5071362986838));
#34275=CARTESIAN_POINT('Ctrl Pts',(-13.8755492926242,1.9729679754383,12.3567453325002));
#34276=CARTESIAN_POINT('Ctrl Pts',(-52.5606120871006,0.237308438758995,
1.7568092319314));
#34277=CARTESIAN_POINT('Ctrl Pts',(-52.3365811493543,0.227921876287717,
2.09077303370513));
#34278=CARTESIAN_POINT('Ctrl Pts',(-52.1053556035498,0.218854274805993,
2.42171900485068));
#34279=CARTESIAN_POINT('Ctrl Pts',(-51.0879099056863,0.181679983795775,
3.82019619056501));
#34280=CARTESIAN_POINT('Ctrl Pts',(-49.4168749753258,0.133848323063104,
5.83677555706815));
#34281=CARTESIAN_POINT('Ctrl Pts',(-46.6128290745602,0.0830496793456984,
8.47584076816339));
#34282=CARTESIAN_POINT('Ctrl Pts',(-43.042935990631,0.0403924264632703,
11.0919484184786));
#34283=CARTESIAN_POINT('Ctrl Pts',(-39.1607220282688,0.00837005963384143,
13.1138268621901));
#34284=CARTESIAN_POINT('Ctrl Pts',(-35.057611354433,-0.0279539839125438,
14.5183472740695));
#34285=CARTESIAN_POINT('Ctrl Pts',(-30.8266189755247,-0.0750512999789021,
15.4169100192373));
#34286=CARTESIAN_POINT('Ctrl Pts',(-26.4968422963745,-0.14423024726241,
15.6680790196882));
#34287=CARTESIAN_POINT('Ctrl Pts',(-22.1598678274238,-0.245792879606331,
15.2498574169528));
#34288=CARTESIAN_POINT('Ctrl Pts',(-18.479339761014,-0.358291148292244,
14.4224610081486));
#34289=CARTESIAN_POINT('Ctrl Pts',(-16.0780703993592,-0.451704594358635,
13.551672433831));
#34290=CARTESIAN_POINT('Ctrl Pts',(-14.5247726836695,-0.519340602547392,
12.8716869099791));
#34291=CARTESIAN_POINT('Ctrl Pts',(-14.1567035816969,-0.535923052101836,
12.7015674050379));
#34292=CARTESIAN_POINT('Ctrl Pts',(-13.7933819214922,-0.552841667182328,
12.5246829031289));
#34293=CARTESIAN_POINT('Ctrl Pts',(-52.890754328659,-2.14030259993981,3.13037102927048));
#34294=CARTESIAN_POINT('Ctrl Pts',(-52.657228107773,-2.14321532053782,3.45848437102345));
#34295=CARTESIAN_POINT('Ctrl Pts',(-52.4165290093469,-2.14576465810466,
3.78332769304311));
#34296=CARTESIAN_POINT('Ctrl Pts',(-51.3587858092243,-2.15494826818845,
5.15466604875529));
#34297=CARTESIAN_POINT('Ctrl Pts',(-49.6282458760827,-2.16016260296573,
7.12536059420484));
#34298=CARTESIAN_POINT('Ctrl Pts',(-46.7425200714405,-2.1481556077715,9.68318376842775));
#34299=CARTESIAN_POINT('Ctrl Pts',(-43.0873089005232,-2.11918777525101,
12.1907133889699));
#34300=CARTESIAN_POINT('Ctrl Pts',(-39.1336679603413,-2.08197924289826,
14.0876535838583));
#34301=CARTESIAN_POINT('Ctrl Pts',(-34.9751571205844,-2.05170003121316,
15.3522532943094));
#34302=CARTESIAN_POINT('Ctrl Pts',(-30.7027227640134,-2.03426137368081,
16.0996671248213));
#34303=CARTESIAN_POINT('Ctrl Pts',(-26.3503698404099,-2.04135770257883,
16.1866083095668));
#34304=CARTESIAN_POINT('Ctrl Pts',(-22.0117968234591,-2.08278583441843,
15.5925376255057));
#34305=CARTESIAN_POINT('Ctrl Pts',(-18.345239938277,-2.14471303148954,14.6071159445911));
#34306=CARTESIAN_POINT('Ctrl Pts',(-15.9641459641279,-2.20477046252904,
13.6265599022038));
#34307=CARTESIAN_POINT('Ctrl Pts',(-14.4278995707152,-2.25046208753918,
12.8730584763167));
#34308=CARTESIAN_POINT('Ctrl Pts',(-14.0644019743396,-2.26180965939547,
12.6854345106128));
#34309=CARTESIAN_POINT('Ctrl Pts',(-13.7061209153785,-2.27353152926925,
12.4911916848406));
#34310=CARTESIAN_POINT('Ctrl Pts',(-53.1032912039355,-3.83428286431684,
4.01176084911006));
#34311=CARTESIAN_POINT('Ctrl Pts',(-52.8632528626129,-3.83237339034492,
4.33600459105002));
#34312=CARTESIAN_POINT('Ctrl Pts',(-52.6160567145443,-3.83006698099443,
4.65680426763478));
#34313=CARTESIAN_POINT('Ctrl Pts',(-51.530678565802,-3.81839846831683,6.01013065392125));
#34314=CARTESIAN_POINT('Ctrl Pts',(-49.759334630619,-3.79185933798401,7.95023150514814));
#34315=CARTESIAN_POINT('Ctrl Pts',(-46.8176122011927,-3.73301479320489,
10.4535182943327));
#34316=CARTESIAN_POINT('Ctrl Pts',(-43.1039324419476,-3.65055513724086,
12.8878101932113));
#34317=CARTESIAN_POINT('Ctrl Pts',(-39.1013809514705,-3.56151400652134,
14.7001087066328));
#34318=CARTESIAN_POINT('Ctrl Pts',(-34.9049930164177,-3.48120332570528,
15.8696164243301));
#34319=CARTESIAN_POINT('Ctrl Pts',(-30.6042940209659,-3.41513875248544,
16.5141034371326));
#34320=CARTESIAN_POINT('Ctrl Pts',(-26.2366723205577,-3.37526128513496,
16.4889878616773));
#34321=CARTESIAN_POINT('Ctrl Pts',(-21.8972872475658,-3.37099617994084,
15.7747435778838));
#34322=CARTESIAN_POINT('Ctrl Pts',(-18.2406096187147,-3.39437469848804,
14.6812175248876));
#34323=CARTESIAN_POINT('Ctrl Pts',(-15.8735908020004,-3.42893690611626,
13.6255049859516));
#34324=CARTESIAN_POINT('Ctrl Pts',(-14.3492100804318,-3.45783930783476,
12.8216495280743));
#34325=CARTESIAN_POINT('Ctrl Pts',(-13.9888888382134,-3.46518513130081,
12.622048154141));
#34326=CARTESIAN_POINT('Ctrl Pts',(-13.6341053234284,-3.47293757911652,
12.4159397012604));
#34327=CARTESIAN_POINT('Ctrl Pts',(-53.1601903434721,-4.30636894546118,
4.2473972842643));
#34328=CARTESIAN_POINT('Ctrl Pts',(-52.9183653507488,-4.3031084050989,4.57059999598952));
#34329=CARTESIAN_POINT('Ctrl Pts',(-52.6693862245725,-4.29944065268701,
4.89031068574757));
#34330=CARTESIAN_POINT('Ctrl Pts',(-51.5764222971609,-4.28192251284736,
6.23878159611758));
#34331=CARTESIAN_POINT('Ctrl Pts',(-49.7938739335711,-4.24645759656194,
8.1706048791254));
#34332=CARTESIAN_POINT('Ctrl Pts',(-46.8367693381174,-4.17439213330946,
10.6590570403307));
#34333=CARTESIAN_POINT('Ctrl Pts',(-43.1070263635738,-4.07676875425951,
13.0733547091991));
#34334=CARTESIAN_POINT('Ctrl Pts',(-39.0910430470873,-3.97294922980807,
14.8624751290696));
#34335=CARTESIAN_POINT('Ctrl Pts',(-34.8842670257438,-3.87828739688684,
16.0058968704492));
#34336=CARTESIAN_POINT('Ctrl Pts',(-30.5758354149997,-3.79820251809058,
16.6221317740867));
#34337=CARTESIAN_POINT('Ctrl Pts',(-26.2040674843958,-3.74469501429227,
16.5662546574962));
#34338=CARTESIAN_POINT('Ctrl Pts',(-21.8645183078476,-3.72710099262819,
15.8190437354006));
#34339=CARTESIAN_POINT('Ctrl Pts',(-18.210605270362,-3.7392015362719,14.6958994891422));
#34340=CARTESIAN_POINT('Ctrl Pts',(-15.8474815123186,-3.76629674044718,
13.6196193253719));
#34341=CARTESIAN_POINT('Ctrl Pts',(-14.3263754116638,-3.79028538091932,
12.8019944646511));
#34342=CARTESIAN_POINT('Ctrl Pts',(-13.9669291566427,-3.79646095010219,
12.5991202663822));
#34343=CARTESIAN_POINT('Ctrl Pts',(-13.6131076449932,-3.80305340259771,
12.3897718290191));
#34344=CARTESIAN_POINT('Ctrl Pts',(-53.215160241902,-4.78145508078572,4.47472655383311));
#34345=CARTESIAN_POINT('Ctrl Pts',(-52.9715659541889,-4.77682808742727,
4.79691749644181));
#34346=CARTESIAN_POINT('Ctrl Pts',(-52.7208204637783,-4.7717826224726,5.11556900438931));
#34347=CARTESIAN_POINT('Ctrl Pts',(-51.62033837218,-4.74834091216943,6.45931390625469));
#34348=CARTESIAN_POINT('Ctrl Pts',(-49.826681616631,-4.70381966688121,8.38304978791861));
#34349=CARTESIAN_POINT('Ctrl Pts',(-46.8543205172875,-4.61828583278682,
10.8569290710769));
#34350=CARTESIAN_POINT('Ctrl Pts',(-43.1086432890248,-4.50515190400754,
13.2515130774504));
#34351=CARTESIAN_POINT('Ctrl Pts',(-39.0793411611953,-4.38613315046716,
15.0177107421923));
#34352=CARTESIAN_POINT('Ctrl Pts',(-34.8622778213812,-4.27662792828432,
16.1352883928939));
#34353=CARTESIAN_POINT('Ctrl Pts',(-30.5462074145363,-4.18197237106197,
16.7235169409871));
#34354=CARTESIAN_POINT('Ctrl Pts',(-26.1703739293047,-4.11421750462538,
16.6371432586749));
#34355=CARTESIAN_POINT('Ctrl Pts',(-21.8307192732995,-4.08262421860679,
15.8572735488346));
#34356=CARTESIAN_POINT('Ctrl Pts',(-18.179597184834,-4.0828488851085,14.7048258212658));
#34357=CARTESIAN_POINT('Ctrl Pts',(-15.8203637738754,-4.10207414795096,
13.6082204427389));
#34358=CARTESIAN_POINT('Ctrl Pts',(-14.3025195588351,-4.12088738197538,
12.776999220031));
#34359=CARTESIAN_POINT('Ctrl Pts',(-13.9439433330175,-4.12583098108427,
12.5708945965306));
#34360=CARTESIAN_POINT('Ctrl Pts',(-13.5910770012361,-4.13120272145022,
12.3583493234692));
#34361=CARTESIAN_POINT('',(-41.8541565650246,20.7105311502984,-21.1067383182144));
#34362=CARTESIAN_POINT('Ctrl Pts',(-41.8541606617387,20.7105314630301,-21.1067474351839));
#34363=CARTESIAN_POINT('Ctrl Pts',(-39.7295427826956,20.5483441672165,-16.3785508491963));
#34364=CARTESIAN_POINT('Ctrl Pts',(-36.6735238440582,20.4520245495079,-12.0795659696835));
#34365=CARTESIAN_POINT('Ctrl Pts',(-29.2347502694402,20.3052748660675,-4.861962389441));
#34366=CARTESIAN_POINT('Ctrl Pts',(-24.8528638925488,20.248474007324,-1.94033620546688));
#34367=CARTESIAN_POINT('Ctrl Pts',(-20.067365612881,20.1925493450898,0.0414315931501192));
#34368=CARTESIAN_POINT('',(-45.5574401880941,-3.27137091447505,11.0356095483923));
#34369=CARTESIAN_POINT('Ctrl Pts',(-41.8541565650195,20.7105311502992,-21.1067383182116));
#34370=CARTESIAN_POINT('Ctrl Pts',(-43.2784775859439,19.9641948262067,-18.2823438856532));
#34371=CARTESIAN_POINT('Ctrl Pts',(-44.3685065694085,18.7336174322537,-15.3991351590888));
#34372=CARTESIAN_POINT('Ctrl Pts',(-46.0288074700108,15.6437709263416,-9.45081981765083));
#34373=CARTESIAN_POINT('Ctrl Pts',(-46.544980861968,13.6706054953477,-6.29727873979032));
#34374=CARTESIAN_POINT('Ctrl Pts',(-46.9598955651361,9.45712578015162,-0.478364493721878));
#34375=CARTESIAN_POINT('Ctrl Pts',(-46.8862235035279,7.18268855808127,2.2621291923848));
#34376=CARTESIAN_POINT('Ctrl Pts',(-46.3912855803782,2.26699026933625,7.13843410632294));
#34377=CARTESIAN_POINT('Ctrl Pts',(-45.9810130440977,-0.365223992195544,
9.28700597763431));
#34378=CARTESIAN_POINT('Ctrl Pts',(-45.5574400014258,-3.27137053313469,
11.0356101369551));
#34379=CARTESIAN_POINT('Ctrl Pts',(-45.5574399163743,-3.27137100135121,
11.0356091539468));
#34380=CARTESIAN_POINT('Ctrl Pts',(-44.9166357013057,-3.25992112204952,
11.4745151676869));
#34381=CARTESIAN_POINT('Ctrl Pts',(-44.261681176221,-3.24789096533568,11.8872675855542));
#34382=CARTESIAN_POINT('Ctrl Pts',(-43.5942284150339,-3.23555894384663,
12.2734886145391));
#34383=CARTESIAN_POINT('Ctrl Pts',(-41.9596126991115,-3.2053573815679,13.2193577464244));
#34384=CARTESIAN_POINT('Ctrl Pts',(-40.2500354155345,-3.17334534347451,
14.0060973871022));
#34385=CARTESIAN_POINT('Ctrl Pts',(-38.4898291965579,-3.14345008158506,
14.6282917586553));
#34386=CARTESIAN_POINT('Ctrl Pts',(-37.3163583243798,-3.12351990598108,
15.0430880273988));
#34387=CARTESIAN_POINT('Ctrl Pts',(-36.1203857008334,-3.10453051989493,
15.3847530580121));
#34388=CARTESIAN_POINT('Ctrl Pts',(-34.9091314157924,-3.08752071373525,
15.6517249226301));
#34389=CARTESIAN_POINT('Ctrl Pts',(-33.6978771313855,-3.07051090758448,
15.9186967871083));
#34390=CARTESIAN_POINT('Ctrl Pts',(-32.4713411854945,-3.0554806813514,16.110975485675));
#34391=CARTESIAN_POINT('Ctrl Pts',(-31.2367458399556,-3.04339100491456,
16.2270169755245));
#34392=CARTESIAN_POINT('Ctrl Pts',(-29.3848528239486,-3.02525649028182,
16.4010792100824));
#34393=CARTESIAN_POINT('Ctrl Pts',(-27.5148261587893,-3.01373821257335,
16.4036077255193));
#34394=CARTESIAN_POINT('Ctrl Pts',(-25.6510314119391,-3.01128625574909,
16.2295094149015));
#34395=CARTESIAN_POINT('Ctrl Pts',(-24.4085015836232,-3.00965161787009,
16.1134438747622));
#34396=CARTESIAN_POINT('Ctrl Pts',(-23.1687414966973,-3.01204645592803,
15.918877523405));
#34397=CARTESIAN_POINT('Ctrl Pts',(-21.9389594448249,-3.01891855380822,
15.6443269212343));
#34398=CARTESIAN_POINT('Ctrl Pts',(-20.70917754041,-3.02579065086441,15.3697763519838));
#34399=CARTESIAN_POINT('Ctrl Pts',(-19.4893736686176,-3.03714000665748,
15.0152415511123));
#34400=CARTESIAN_POINT('Ctrl Pts',(-18.2867431495384,-3.05321938564873,
14.5792465784353));
#34401=CARTESIAN_POINT('Ctrl Pts',(-17.7911796469897,-3.05984515577954,
14.3995877452977));
#34402=CARTESIAN_POINT('Ctrl Pts',(-17.2985321692438,-3.06727406915266,
14.2060970869875));
#34403=CARTESIAN_POINT('Ctrl Pts',(-16.809302921024,-3.07550335254719,13.9986721479021));
#34404=CARTESIAN_POINT('Ctrl Pts',(-53.2550241076282,-4.68328060676847,
4.62744272080562));
#34405=CARTESIAN_POINT('Ctrl Pts',(-53.0102407077981,-4.67927906663786,
4.9503893548096));
#34406=CARTESIAN_POINT('Ctrl Pts',(-52.7582576936744,-4.67486342687383,
5.26975370936434));
#34407=CARTESIAN_POINT('Ctrl Pts',(-51.655544643172,-4.65418501649615,6.6123848263081));
#34408=CARTESIAN_POINT('Ctrl Pts',(-49.8600436026871,-4.61395560865182,
8.53249843791617));
#34409=CARTESIAN_POINT('Ctrl Pts',(-46.8850762930286,-4.53496565777432,
11.0007825140162));
#34410=CARTESIAN_POINT('Ctrl Pts',(-43.1365657964198,-4.42959393838223,
13.3886632292394));
#34411=CARTESIAN_POINT('Ctrl Pts',(-39.1047177769365,-4.31850354734918,
15.1479551320865));
#34412=CARTESIAN_POINT('Ctrl Pts',(-34.8854383833948,-4.2170896233612,16.2584454359381));
#34413=CARTESIAN_POINT('Ctrl Pts',(-30.5674377343485,-4.13063759391767,
16.8394400005655));
#34414=CARTESIAN_POINT('Ctrl Pts',(-26.1900645771467,-4.07121155600733,
16.7456659202151));
#34415=CARTESIAN_POINT('Ctrl Pts',(-21.8493056943788,-4.04803120464602,
15.9582493147047));
#34416=CARTESIAN_POINT('Ctrl Pts',(-18.1975571114897,-4.055480889925,14.7992430763966));
#34417=CARTESIAN_POINT('Ctrl Pts',(-15.8381298955582,-4.07952578289679,
13.698223661129));
#34418=CARTESIAN_POINT('Ctrl Pts',(-14.3182865449456,-4.10152925776619,
12.8630191402326));
#34419=CARTESIAN_POINT('Ctrl Pts',(-13.9578284677764,-4.1072571624472,12.6550855609606));
#34420=CARTESIAN_POINT('Ctrl Pts',(-13.6031599189745,-4.11341014061892,
12.4406557045438));
#34421=CARTESIAN_POINT('Ctrl Pts',(-53.1870621995371,-4.24009445412503,
4.34532464343756));
#34422=CARTESIAN_POINT('Ctrl Pts',(-52.9441663261533,-4.23725223817857,
4.66946739029586));
#34423=CARTESIAN_POINT('Ctrl Pts',(-52.6940654070999,-4.23400446880359,
4.99008143969754));
#34424=CARTESIAN_POINT('Ctrl Pts',(-51.5993293700175,-4.21832863439708,
6.33826150780282));
#34425=CARTESIAN_POINT('Ctrl Pts',(-49.8156106685733,-4.18572164472913,
8.26773769630283));
#34426=CARTESIAN_POINT('Ctrl Pts',(-46.8568510448354,-4.11799618192084,
10.7525697593713));
#34427=CARTESIAN_POINT('Ctrl Pts',(-43.1253084596183,-4.02550335874969,
13.1625385894897));
#34428=CARTESIAN_POINT('Ctrl Pts',(-39.1077078270931,-3.92690475481451,
14.9472114885605));
#34429=CARTESIAN_POINT('Ctrl Pts',(-34.8995234161583,-3.83755718932749,
16.0860839457906));
#34430=CARTESIAN_POINT('Ctrl Pts',(-30.589864068293,-3.76285616468038,16.6976922413632));
#34431=CARTESIAN_POINT('Ctrl Pts',(-26.2171128932958,-3.71481495977278,
16.6371028524245));
#34432=CARTESIAN_POINT('Ctrl Pts',(-21.8768503613734,-3.70275434803773,
15.8851071811083));
#34433=CARTESIAN_POINT('Ctrl Pts',(-18.2225224734843,-3.71962751323487,
14.7578178297532));
#34434=CARTESIAN_POINT('Ctrl Pts',(-15.8592594973308,-3.74992063397164,
13.6787524066036));
#34435=CARTESIAN_POINT('Ctrl Pts',(-14.3361562667453,-3.77604797989279,
12.8582381071574));
#34436=CARTESIAN_POINT('Ctrl Pts',(-13.974817866806,-3.78276245762616,12.6538069497816));
#34437=CARTESIAN_POINT('Ctrl Pts',(-13.6191764391839,-3.78989370687861,
12.4428410361005));
#34438=CARTESIAN_POINT('Ctrl Pts',(-53.1177874295843,-3.80075287541765,
4.05749922158663));
#34439=CARTESIAN_POINT('Ctrl Pts',(-52.8767867368435,-3.79905339336963,
4.38285827146066));
#34440=CARTESIAN_POINT('Ctrl Pts',(-52.6285750022794,-3.79695621683146,
4.7047423894142));
#34441=CARTESIAN_POINT('Ctrl Pts',(-51.541843702939,-3.78620663871065,6.05855883565579));
#34442=CARTESIAN_POINT('Ctrl Pts',(-49.7699443207133,-3.76109400159902,
7.99752044121646));
#34443=CARTESIAN_POINT('Ctrl Pts',(-46.8274357987597,-3.70440674399875,
10.4990527223183));
#34444=CARTESIAN_POINT('Ctrl Pts',(-43.1129011207827,-3.62448835210827,
12.9312507195699));
#34445=CARTESIAN_POINT('Ctrl Pts',(-39.1095812653897,-3.53802316526296,
14.7414040548252));
#34446=CARTESIAN_POINT('Ctrl Pts',(-34.9125240042515,-3.46032715355504,
15.9087253564222));
#34447=CARTESIAN_POINT('Ctrl Pts',(-30.6112411258892,-3.39690914788247,
16.5509976263655));
#34448=CARTESIAN_POINT('Ctrl Pts',(-26.2431498662277,-3.35971861494906,
16.5236373449463));
#34449=CARTESIAN_POINT('Ctrl Pts',(-21.9034199271629,-3.35817927654809,
15.8071251099738));
#34450=CARTESIAN_POINT('Ctrl Pts',(-18.2465365368635,-3.38391914529348,
14.7116415712368));
#34451=CARTESIAN_POINT('Ctrl Pts',(-15.879443166288,-3.42007079724739,13.6546163643265));
#34452=CARTESIAN_POINT('Ctrl Pts',(-14.3530780248134,-3.45006162272336,
12.8488621843749));
#34453=CARTESIAN_POINT('Ctrl Pts',(-13.990857400756,-3.45770043113048,12.6479516105235));
#34454=CARTESIAN_POINT('Ctrl Pts',(-13.6342398281543,-3.46574819271174,
12.4404689854205));
#34455=CARTESIAN_POINT('Ctrl Pts',(-52.8689004777194,-2.2653457359543,3.02246760313475));
#34456=CARTESIAN_POINT('Ctrl Pts',(-52.6346047659193,-2.26761569662348,
3.35218985314796));
#34457=CARTESIAN_POINT('Ctrl Pts',(-52.3930760318627,-2.26951335386862,
3.67862619991285));
#34458=CARTESIAN_POINT('Ctrl Pts',(-51.3346585498217,-2.27586002752392,
5.05262899676798));
#34459=CARTESIAN_POINT('Ctrl Pts',(-49.6045518529517,-2.27671432942662,
7.02547485602001));
#34460=CARTESIAN_POINT('Ctrl Pts',(-46.7194808240327,-2.25814179129592,
9.58643472149431));
#34461=CARTESIAN_POINT('Ctrl Pts',(-43.0650395670317,-2.2214798205824,12.0975139363354));
#34462=CARTESIAN_POINT('Ctrl Pts',(-39.1121771246984,-2.17652897108851,
13.9978620983042));
#34463=CARTESIAN_POINT('Ctrl Pts',(-34.9544569047753,-2.13845241575724,
15.2657254601391));
#34464=CARTESIAN_POINT('Ctrl Pts',(-30.6828258526428,-2.11316923258448,
16.0162881999903));
#34465=CARTESIAN_POINT('Ctrl Pts',(-26.3312963999019,-2.11235831802136,
16.1062368873549));
#34466=CARTESIAN_POINT('Ctrl Pts',(-21.9935755581312,-2.14581153060268,
15.5150394164916));
#34467=CARTESIAN_POINT('Ctrl Pts',(-18.327773585856,-2.20085463389179,14.5319934262389));
#34468=CARTESIAN_POINT('Ctrl Pts',(-15.9472027453685,-2.25628908058851,
13.5529671676988));
#34469=CARTESIAN_POINT('Ctrl Pts',(-14.4093368232033,-2.29898278275007,
12.799490048317));
#34470=CARTESIAN_POINT('Ctrl Pts',(-14.0440004582171,-2.30966173471912,
12.6110582357232));
#34471=CARTESIAN_POINT('Ctrl Pts',(-13.6839307875775,-2.32072459453129,
12.4159313107788));
#34472=CARTESIAN_POINT('Ctrl Pts',(-52.4024685456813,0.42091842584111,1.07848752259329));
#34473=CARTESIAN_POINT('Ctrl Pts',(-52.1802375771876,0.412015546281074,
1.41623609520554));
#34474=CARTESIAN_POINT('Ctrl Pts',(-51.9507383304312,0.403442573942463,
1.75103341927263));
#34475=CARTESIAN_POINT('Ctrl Pts',(-50.9433065549328,0.368526239150617,
3.16205940115231));
#34476=CARTESIAN_POINT('Ctrl Pts',(-49.288458491273,0.324281374370589,5.1968918518957));
#34477=CARTESIAN_POINT('Ctrl Pts',(-46.5068266086684,0.279215865745994,
7.86614365370726));
#34478=CARTESIAN_POINT('Ctrl Pts',(-42.9606237061091,0.243759038204317,
10.5205566320174));
#34479=CARTESIAN_POINT('Ctrl Pts',(-39.0986741979798,0.21967725703067,12.5843645499658));
#34480=CARTESIAN_POINT('Ctrl Pts',(-35.011880788994,0.192114722189047,14.0340846219934));
#34481=CARTESIAN_POINT('Ctrl Pts',(-30.7937738910368,0.154437491851918,
14.980275523655));
#34482=CARTESIAN_POINT('Ctrl Pts',(-26.4722529890479,0.0954817696064694,
15.2818750597512));
#34483=CARTESIAN_POINT('Ctrl Pts',(-22.1384049721548,0.0048363712043943,
14.9165437766969));
#34484=CARTESIAN_POINT('Ctrl Pts',(-18.4568160996774,-0.0979118428630517,
14.1360163938409));
#34485=CARTESIAN_POINT('Ctrl Pts',(-16.0521989825758,-0.184631554593919,
13.2973974695823));
#34486=CARTESIAN_POINT('Ctrl Pts',(-14.4937852736123,-0.247909792323189,
12.6380015081389));
#34487=CARTESIAN_POINT('Ctrl Pts',(-14.1228765604169,-0.263520166061751,
12.4720559824965));
#34488=CARTESIAN_POINT('Ctrl Pts',(-13.75662704767,-0.279478515480188,12.2992216174618));
#34489=CARTESIAN_POINT('Ctrl Pts',(-51.6812106838394,3.93922736422659,-1.9401699282817));
#34490=CARTESIAN_POINT('Ctrl Pts',(-51.4760538436571,3.92273017306588,-1.59057825251053));
#34491=CARTESIAN_POINT('Ctrl Pts',(-51.263584894514,3.90651491483579,-1.24347554024485));
#34492=CARTESIAN_POINT('Ctrl Pts',(-50.3283655357373,3.83888692720806,0.221910991507739));
#34493=CARTESIAN_POINT('Ctrl Pts',(-48.7801103103006,3.74496038387833,2.34729155538723));
#34494=CARTESIAN_POINT('Ctrl Pts',(-46.1450033475284,3.6271896762232,5.17349042592491));
#34495=CARTESIAN_POINT('Ctrl Pts',(-42.7521630054787,3.50969140214063,8.03442807426281));
#34496=CARTESIAN_POINT('Ctrl Pts',(-39.0191042094579,3.40771510315772,10.3324686633491));
#34497=CARTESIAN_POINT('Ctrl Pts',(-35.0329941213862,3.30695483103527,12.0417080640687));
#34498=CARTESIAN_POINT('Ctrl Pts',(-30.891020829036,3.1998573133211,13.2663261001275));
#34499=CARTESIAN_POINT('Ctrl Pts',(-26.6124740089013,3.07607789704229,13.8683245393028));
#34500=CARTESIAN_POINT('Ctrl Pts',(-22.2847669139082,2.92448144596071,13.8228473589188));
#34501=CARTESIAN_POINT('Ctrl Pts',(-18.5815246338201,2.77158317941627,13.3286701208219));
#34502=CARTESIAN_POINT('Ctrl Pts',(-16.1434293986355,2.65236568914073,12.6883132843688));
#34503=CARTESIAN_POINT('Ctrl Pts',(-14.5563351006402,2.56779645721963,12.1616854590491));
#34504=CARTESIAN_POINT('Ctrl Pts',(-14.1776469180455,2.54707902977605,12.0275353341212));
#34505=CARTESIAN_POINT('Ctrl Pts',(-13.8027662533503,2.52604544176493,11.8862838166198));
#34506=CARTESIAN_POINT('Ctrl Pts',(-50.7849974013264,7.64857049485316,-5.70122737713707));
#34507=CARTESIAN_POINT('Ctrl Pts',(-50.5995059831301,7.62538079009264,-5.33758143700541));
#34508=CARTESIAN_POINT('Ctrl Pts',(-50.4066643269634,7.6024320797305,-4.97591736065702));
#34509=CARTESIAN_POINT('Ctrl Pts',(-49.5547312908686,7.50598047950645,-3.44637468117887));
#34510=CARTESIAN_POINT('Ctrl Pts',(-48.1294152598895,7.36825978906471,-1.21450705382876));
#34511=CARTESIAN_POINT('Ctrl Pts',(-45.6633104617947,7.18657585481396,1.79524361104216));
#34512=CARTESIAN_POINT('Ctrl Pts',(-42.4473772579401,6.99739878870591,4.89670142836206));
#34513=CARTESIAN_POINT('Ctrl Pts',(-38.8630354862451,6.82819742189185,7.46642848002267));
#34514=CARTESIAN_POINT('Ctrl Pts',(-34.993164758737,6.66543158101024,9.47573998110103));
#34515=CARTESIAN_POINT('Ctrl Pts',(-30.9391726596963,6.50060855796851,11.0216245495761));
#34516=CARTESIAN_POINT('Ctrl Pts',(-26.7104480931522,6.32441606849526,11.9694786820947));
#34517=CARTESIAN_POINT('Ctrl Pts',(-22.3901917930574,6.12505774886043,12.2915705314655));
#34518=CARTESIAN_POINT('Ctrl Pts',(-18.662378603183,5.93384517916791,12.1260283153189));
#34519=CARTESIAN_POINT('Ctrl Pts',(-16.1860069271246,5.79035915091665,11.7129412555412));
#34520=CARTESIAN_POINT('Ctrl Pts',(-14.5660799894216,5.69001969995687,11.3384237535995));
#34521=CARTESIAN_POINT('Ctrl Pts',(-14.1785181216796,5.66551509710643,11.2407915689695));
#34522=CARTESIAN_POINT('Ctrl Pts',(-13.7938169458334,5.64071489355821,11.1359032947783));
#34523=CARTESIAN_POINT('Ctrl Pts',(-49.9421179311135,10.6050661536892,-9.24468742082597));
#34524=CARTESIAN_POINT('Ctrl Pts',(-49.7739435279274,10.5777689837161,-8.86839695461952));
#34525=CARTESIAN_POINT('Ctrl Pts',(-49.5983941291953,10.5506896266998,-8.49366788478655));
#34526=CARTESIAN_POINT('Ctrl Pts',(-48.8198852019977,10.4365567481294,-6.90671046826663));
#34527=CARTESIAN_POINT('Ctrl Pts',(-47.5029498445623,10.2719415070743,-4.57979182054436));
#34528=CARTESIAN_POINT('Ctrl Pts',(-45.1858329874651,10.0511774947007,-1.40687928349953));
#34529=CARTESIAN_POINT('Ctrl Pts',(-42.1258585913662,9.81863871620139,1.90769663539571));
#34530=CARTESIAN_POINT('Ctrl Pts',(-38.6726313940744,9.60967367489776,4.71739998166952));
#34531=CARTESIAN_POINT('Ctrl Pts',(-34.9052599503476,9.41153176383594,6.99109418128465));
#34532=CARTESIAN_POINT('Ctrl Pts',(-30.9288736511082,9.21500541081661,8.81955439844158));
#34533=CARTESIAN_POINT('Ctrl Pts',(-26.7441444079205,9.01175979868378,10.07105129362));
#34534=CARTESIAN_POINT('Ctrl Pts',(-22.4305703275812,8.78956564702969,10.7153281176886));
#34535=CARTESIAN_POINT('Ctrl Pts',(-18.6812269030208,8.58124477590158,10.8375076202336));
#34536=CARTESIAN_POINT('Ctrl Pts',(-16.1712252072741,8.42762540105217,10.6231810669046));
#34537=CARTESIAN_POINT('Ctrl Pts',(-14.5224388077575,8.32086564673385,10.3816244231577));
#34538=CARTESIAN_POINT('Ctrl Pts',(-14.1271306078084,8.29482075310626,10.3159831567471));
#34539=CARTESIAN_POINT('Ctrl Pts',(-13.7339007596026,8.26849188852043,10.2430203848967));
#34540=CARTESIAN_POINT('Ctrl Pts',(-48.9190413835945,13.6252616883324,-13.5486550301516));
#34541=CARTESIAN_POINT('Ctrl Pts',(-48.7707426344082,13.5952855444977,-13.157707499603));
#34542=CARTESIAN_POINT('Ctrl Pts',(-48.6150473980909,13.5655149131873,-12.7678728818138));
#34543=CARTESIAN_POINT('Ctrl Pts',(-47.9208800025026,13.4398628522405,-11.1146965665455));
#34544=CARTESIAN_POINT('Ctrl Pts',(-46.728437940084,13.2576618204372,-8.67830331115292));
#34545=CARTESIAN_POINT('Ctrl Pts',(-44.5824461493721,13.0115743729063,-5.31790493889871));
#34546=CARTESIAN_POINT('Ctrl Pts',(-41.7015829857729,12.751644575675,-1.75889877066355));
#34547=CARTESIAN_POINT('Ctrl Pts',(-38.3989009034041,12.5189796899122,1.32550695910777));
#34548=CARTESIAN_POINT('Ctrl Pts',(-34.7491709788807,12.301865256328,3.90134067434971));
#34549=CARTESIAN_POINT('Ctrl Pts',(-30.8618018689639,12.0904144587841,6.05235254691278));
#34550=CARTESIAN_POINT('Ctrl Pts',(-26.7274417568102,11.8774764455751,7.64998503667857));
#34551=CARTESIAN_POINT('Ctrl Pts',(-22.4213311430581,11.6504923923572,8.66107165744092));
#34552=CARTESIAN_POINT('Ctrl Pts',(-18.6470419033825,11.4410171343385,9.1105101988073));
#34553=CARTESIAN_POINT('Ctrl Pts',(-16.09824451068,11.2882220371981,9.12204563341117));
#34554=CARTESIAN_POINT('Ctrl Pts',(-14.4161911759617,11.1823584691134,9.03150892265254));
#34555=CARTESIAN_POINT('Ctrl Pts',(-14.0120429911226,11.1565388193505,9.00226487804507));
#34556=CARTESIAN_POINT('Ctrl Pts',(-13.6091566427535,11.1304479812224,8.96568686170588));
#34557=CARTESIAN_POINT('Ctrl Pts',(-47.9760265763764,15.9398275064074,-17.5159409401114));
#34558=CARTESIAN_POINT('Ctrl Pts',(-47.845173721344,15.9092719019138,-17.1120993990557));
#34559=CARTESIAN_POINT('Ctrl Pts',(-47.7069077842713,15.8789225535602,-16.7090082004271));
#34560=CARTESIAN_POINT('Ctrl Pts',(-47.0867986772895,15.7507918597713,-14.9978536657822));
#34561=CARTESIAN_POINT('Ctrl Pts',(-46.0036684189674,15.5646999212503,-12.4656708226873));
#34562=CARTESIAN_POINT('Ctrl Pts',(-44.0079170280876,15.3133344724918,-8.94141691639378));
#34563=CARTESIAN_POINT('Ctrl Pts',(-41.28427599618,15.0487502016962,-5.16901063122818));
#34564=CARTESIAN_POINT('Ctrl Pts',(-38.1136889032606,14.8142492774957,-1.84505503058845));
#34565=CARTESIAN_POINT('Ctrl Pts',(-34.5671043809285,14.5991383033468,0.993962480657613));
#34566=CARTESIAN_POINT('Ctrl Pts',(-30.7576929966717,14.3930646018661,3.42570304001716));
#34567=CARTESIAN_POINT('Ctrl Pts',(-26.6672790166255,14.1899609567462,5.32428496179455));
#34568=CARTESIAN_POINT('Ctrl Pts',(-22.3673509929844,13.977122935371,6.65396667590596));
#34569=CARTESIAN_POINT('Ctrl Pts',(-18.5707723340629,13.7824369346935,7.38741364551115));
#34570=CARTESIAN_POINT('Ctrl Pts',(-15.9876039554074,13.6409944051188,7.5947963714473));
#34571=CARTESIAN_POINT('Ctrl Pts',(-14.276121320492,13.5429643472183,7.63515342013838));
#34572=CARTESIAN_POINT('Ctrl Pts',(-13.8642441857383,13.5190447294408,7.63748833309744));
#34573=CARTESIAN_POINT('Ctrl Pts',(-13.4529946868638,13.4948677704672,7.63251220583618));
#34574=CARTESIAN_POINT('Ctrl Pts',(-46.8518840273662,18.188947172369,-22.2413015794463));
#34575=CARTESIAN_POINT('Ctrl Pts',(-46.7409936449756,18.1597316481657,-21.8228367447842));
#34576=CARTESIAN_POINT('Ctrl Pts',(-46.6226695035064,18.1307342364494,-21.4047437320774));
#34577=CARTESIAN_POINT('Ctrl Pts',(-46.0872954411095,18.0083786966032,-19.6281175320506));
#34578=CARTESIAN_POINT('Ctrl Pts',(-45.129232033727,17.830846834045,-16.9877153100835));
#34579=CARTESIAN_POINT('Ctrl Pts',(-43.3053469438411,17.5925027676131,-13.2782512104459));
#34580=CARTESIAN_POINT('Ctrl Pts',(-40.7615054946399,17.3443426911773,-9.26458661207112));
#34581=CARTESIAN_POINT('Ctrl Pts',(-37.7418859285627,17.1289494695207,-5.66981412176888));
#34582=CARTESIAN_POINT('Ctrl Pts',(-34.3130328703258,16.9369213116231,-2.53334672084906));
#34583=CARTESIAN_POINT('Ctrl Pts',(-30.5924274640541,16.7575317657622,0.215568117021719));
#34584=CARTESIAN_POINT('Ctrl Pts',(-26.5517507933222,16.5859876106103,2.45399400638956));
#34585=CARTESIAN_POINT('Ctrl Pts',(-22.2581672791192,16.4095763329362,4.14320050884528));
#34586=CARTESIAN_POINT('Ctrl Pts',(-18.4353192402588,16.2491906636996,5.19694543642052));
#34587=CARTESIAN_POINT('Ctrl Pts',(-15.8122098215815,16.1323920433636,5.62504820870853));
#34588=CARTESIAN_POINT('Ctrl Pts',(-14.0666127972462,16.0510402241362,5.81286568186864));
#34589=CARTESIAN_POINT('Ctrl Pts',(-13.6458884937628,16.0311583490605,5.85078659563688));
#34590=CARTESIAN_POINT('Ctrl Pts',(-13.2251660207337,16.01103806515,5.8814349310918));
#34591=CARTESIAN_POINT('Ctrl Pts',(-45.8324093010083,19.7983627848149,-26.5208862143558));
#34592=CARTESIAN_POINT('Ctrl Pts',(-45.7389874917903,19.7720645135703,-26.0898395604211));
#34593=CARTESIAN_POINT('Ctrl Pts',(-45.6381086468713,19.7460021313493,-25.6588639245312));
#34594=CARTESIAN_POINT('Ctrl Pts',(-45.1768456950506,19.6361820466171,-23.8261216909706));
#34595=CARTESIAN_POINT('Ctrl Pts',(-44.3281644612076,19.4774394485581,-21.0928503619399));
#34596=CARTESIAN_POINT('Ctrl Pts',(-42.6545622359201,19.2670183310104,-17.2241812601364));
#34597=CARTESIAN_POINT('Ctrl Pts',(-40.2678831350707,19.0520629838802,-13.0029153733495));
#34598=CARTESIAN_POINT('Ctrl Pts',(-37.3801185452477,18.8717166252608,-9.17492625949768));
#34599=CARTESIAN_POINT('Ctrl Pts',(-34.0539261447635,18.7178122962125,-5.78223641699785));
#34600=CARTESIAN_POINT('Ctrl Pts',(-30.4105634338668,18.5794411422907,-2.76010396718932));
#34601=CARTESIAN_POINT('Ctrl Pts',(-26.4127865038372,18.4529446490623,-0.228985441518097));
#34602=CARTESIAN_POINT('Ctrl Pts',(-22.1239414086001,18.3257380682571,1.76972639038569));
#34603=CARTESIAN_POINT('Ctrl Pts',(-18.2772624864382,18.2102139945187,3.09907703011229));
#34604=CARTESIAN_POINT('Ctrl Pts',(-15.6185315114537,18.1249152482566,3.71699064283981));
#34605=CARTESIAN_POINT('Ctrl Pts',(-13.8426013038607,18.064727637235,4.03157365432944));
#34606=CARTESIAN_POINT('Ctrl Pts',(-13.4141050388812,18.0499634327475,4.10007468068017));
#34607=CARTESIAN_POINT('Ctrl Pts',(-12.98514701221,18.0349776243875,4.16132700560662));
#34608=CARTESIAN_POINT('Ctrl Pts',(-45.0842283862103,20.6836496418694,-29.6550287755562));
#34609=CARTESIAN_POINT('Ctrl Pts',(-45.003258058161,20.6606519170286,-29.2152696874927));
#34610=CARTESIAN_POINT('Ctrl Pts',(-44.9148096467711,20.6379063239872,-28.7753846724798));
#34611=CARTESIAN_POINT('Ctrl Pts',(-44.5063377455988,20.5422448076096,-26.9038829192087));
#34612=CARTESIAN_POINT('Ctrl Pts',(-43.7355687870834,20.4047755971079,-24.1063107670654));
#34613=CARTESIAN_POINT('Ctrl Pts',(-42.1689863802376,20.225761668211,-20.1270266003951));
#34614=CARTESIAN_POINT('Ctrl Pts',(-39.8941747111083,20.0475517349526,-15.7611783203895));
#34615=CARTESIAN_POINT('Ctrl Pts',(-37.1001683740488,19.9048724048602,-11.7704442775268));
#34616=CARTESIAN_POINT('Ctrl Pts',(-33.8468226781346,19.790507905872,-8.19875157949892));
#34617=CARTESIAN_POINT('Ctrl Pts',(-30.2580901286986,19.6935273080542,-4.98563776740868));
#34618=CARTESIAN_POINT('Ctrl Pts',(-26.2903187546283,19.6110850660289,-2.24985464000988));
#34619=CARTESIAN_POINT('Ctrl Pts',(-22.004099523508,19.530779076001,-0.0347369010676612));
#34620=CARTESIAN_POINT('Ctrl Pts',(-18.1396517532032,19.4573327991495,1.48727002286964));
#34621=CARTESIAN_POINT('Ctrl Pts',(-15.4549058300219,19.4012238336331,2.23781143845789));
#34622=CARTESIAN_POINT('Ctrl Pts',(-13.6569059350236,19.3605693891818,2.64094405458518));
#34623=CARTESIAN_POINT('Ctrl Pts',(-13.2228097538454,19.3505226070412,2.73078956348044));
#34624=CARTESIAN_POINT('Ctrl Pts',(-12.7879686848707,19.3402634731691,2.81338796599552));
#34625=CARTESIAN_POINT('Ctrl Pts',(-44.662892732026,21.117312799858,-31.4181748325572));
#34626=CARTESIAN_POINT('Ctrl Pts',(-44.5888652243124,21.0964267127388,-30.9736279625641));
#34627=CARTESIAN_POINT('Ctrl Pts',(-44.5073458457706,21.0758020890032,-30.5288506865157));
#34628=CARTESIAN_POINT('Ctrl Pts',(-44.1282930941642,20.9891913310095,-28.6360818457722));
#34629=CARTESIAN_POINT('Ctrl Pts',(-43.4009419459597,20.8653273744228,-25.8031807347521));
#34630=CARTESIAN_POINT('Ctrl Pts',(-41.89399142233,20.7063681300896,-21.7630023216518));
#34631=CARTESIAN_POINT('Ctrl Pts',(-39.6814995550379,20.5515335415639,-17.3174532750829));
#34632=CARTESIAN_POINT('Ctrl Pts',(-36.9397000222138,20.4326519806542,-13.2369023278833));
#34633=CARTESIAN_POINT('Ctrl Pts',(-33.7268776305302,20.3430531321453,-9.56634965008858));
#34634=CARTESIAN_POINT('Ctrl Pts',(-30.1684879882071,20.2718184169426,-6.2477203062325));
#34635=CARTESIAN_POINT('Ctrl Pts',(-26.2172948692171,20.2165549432469,-3.39882871550882));
#34636=CARTESIAN_POINT('Ctrl Pts',(-21.9323446710577,20.164982094833,-1.06410354139334));
#34637=CARTESIAN_POINT('Ctrl Pts',(-18.0577887965766,20.117197691553,0.564381352586137));
#34638=CARTESIAN_POINT('Ctrl Pts',(-15.3583788882933,20.0788282397779,1.3882155360768));
#34639=CARTESIAN_POINT('Ctrl Pts',(-13.5479598507639,20.0500302875854,1.84027756187001));
#34640=CARTESIAN_POINT('Ctrl Pts',(-13.1107276962677,20.0428451797642,1.9419101019128));
#34641=CARTESIAN_POINT('Ctrl Pts',(-12.6726064287586,20.0354515632684,2.03628977646432));
#34642=CARTESIAN_POINT('Ctrl Pts',(-44.5430178615257,21.2334813897109,-31.9196050263226));
#34643=CARTESIAN_POINT('Ctrl Pts',(-44.4709595266528,21.2132228077857,-31.4737036812526));
#34644=CARTESIAN_POINT('Ctrl Pts',(-44.3914050023503,21.1932283095702,-31.0275427813411));
#34645=CARTESIAN_POINT('Ctrl Pts',(-44.0206929537339,21.1093059289188,-29.1287610721839));
#34646=CARTESIAN_POINT('Ctrl Pts',(-43.3056498664664,20.9894835119608,-26.2858714770087));
#34647=CARTESIAN_POINT('Ctrl Pts',(-41.8155996100812,20.8364792943525,-22.2284811708669));
#34648=CARTESIAN_POINT('Ctrl Pts',(-39.6207640549177,20.6885792302246,-17.7604142055847));
#34649=CARTESIAN_POINT('Ctrl Pts',(-36.893748873692,20.5767478260626,-13.65450541157));
#34650=CARTESIAN_POINT('Ctrl Pts',(-33.6923948010559,20.4944756050622,-9.95606573502258));
#34651=CARTESIAN_POINT('Ctrl Pts',(-30.1425849867683,20.4308554028779,-6.60769833039274));
#34652=CARTESIAN_POINT('Ctrl Pts',(-26.1960663524986,20.3836340081555,-3.72696185433125));
#34653=CARTESIAN_POINT('Ctrl Pts',(-21.9114441822608,20.340580727313,-1.35859572870376));
#34654=CARTESIAN_POINT('Ctrl Pts',(-18.0339852147836,20.3004356869138,0.29981387071413));
#34655=CARTESIAN_POINT('Ctrl Pts',(-15.3303820039488,20.2673681898868,1.1442388647251));
#34656=CARTESIAN_POINT('Ctrl Pts',(-13.5164122338016,20.2421246596599,1.61004653123375));
#34657=CARTESIAN_POINT('Ctrl Pts',(-13.0782862790771,20.2357981340653,1.71498902850875));
#34658=CARTESIAN_POINT('Ctrl Pts',(-12.6392326905351,20.2292648564311,1.81267574713249));
#34659=CARTESIAN_POINT('Ctrl Pts',(-44.4227536970802,21.3428689572265,-32.4224779048909));
#34660=CARTESIAN_POINT('Ctrl Pts',(-44.3526640269045,21.323266505305,-31.9752258099344));
#34661=CARTESIAN_POINT('Ctrl Pts',(-44.2750736219715,21.303930781031,-31.527685218234));
#34662=CARTESIAN_POINT('Ctrl Pts',(-43.9126982425839,21.2228186866547,-29.622908370639));
#34663=CARTESIAN_POINT('Ctrl Pts',(-43.2099559547992,21.1072213437662,-26.7700597812476));
#34664=CARTESIAN_POINT('Ctrl Pts',(-41.7367921725809,20.9604400919523,-22.695512686503));
#34665=CARTESIAN_POINT('Ctrl Pts',(-39.559593085345,20.819779963638,-18.2050092760581));
#34666=CARTESIAN_POINT('Ctrl Pts',(-36.8473391964997,20.7152993064879,-14.0738520907221));
#34667=CARTESIAN_POINT('Ctrl Pts',(-33.6574284865114,20.6406553883908,-10.3476693174035));
#34668=CARTESIAN_POINT('Ctrl Pts',(-30.116172752319,20.5849601975755,-6.9697435065069));
#34669=CARTESIAN_POINT('Ctrl Pts',(-26.1743020658466,20.5461109852346,-4.05738761544544));
#34670=CARTESIAN_POINT('Ctrl Pts',(-21.8899779235893,20.5119420676311,-1.65565290050457));
#34671=CARTESIAN_POINT('Ctrl Pts',(-18.0095823216269,20.4797911688045,0.0324145407608299));
#34672=CARTESIAN_POINT('Ctrl Pts',(-15.3017542572766,20.4522911786996,0.897238235717693));
#34673=CARTESIAN_POINT('Ctrl Pts',(-13.4842075697677,20.4307901345004,1.37666218058237));
#34674=CARTESIAN_POINT('Ctrl Pts',(-13.045183204915,20.4253683033402,1.48488253420603));
#34675=CARTESIAN_POINT('Ctrl Pts',(-12.6051943113167,20.4197421663948,1.58584330107463));
#34676=CARTESIAN_POINT('',(-41.8448486400327,20.5529756002067,-21.125185596459));
#34677=CARTESIAN_POINT('Ctrl Pts',(-45.5574402514582,-3.27137127985419,
11.0356091047656));
#34678=CARTESIAN_POINT('Ctrl Pts',(-46.5282583031688,1.76302065360852,7.02785488001061));
#34679=CARTESIAN_POINT('Ctrl Pts',(-47.208951015116,6.26298702224666,1.80001364845749));
#34680=CARTESIAN_POINT('Ctrl Pts',(-46.4493663072616,12.5188402724798,-6.92582206775948));
#34681=CARTESIAN_POINT('Ctrl Pts',(-45.9228610941799,14.4577038717082,-9.88449847911477));
#34682=CARTESIAN_POINT('Ctrl Pts',(-44.3011001623703,17.848637426394,-15.5857057966297));
#34683=CARTESIAN_POINT('Ctrl Pts',(-43.226555471649,19.3555632898771,-18.3882954426068));
#34684=CARTESIAN_POINT('Ctrl Pts',(-41.8448486400325,20.5529756002057,-21.1251855964593));
#34685=CARTESIAN_POINT('Ctrl Pts',(-20.6391955918159,19.9464420456703,-0.223416847360507));
#34686=CARTESIAN_POINT('Ctrl Pts',(-25.3016667625211,20.0189549105364,-2.24188131992115));
#34687=CARTESIAN_POINT('Ctrl Pts',(-29.5639710976893,20.0954766247834,-5.1557195977613));
#34688=CARTESIAN_POINT('Ctrl Pts',(-36.794002124349,20.2752040736289,-12.2855823812624));
#34689=CARTESIAN_POINT('Ctrl Pts',(-39.7632550653996,20.3824974081049,-16.5004134660379));
#34690=CARTESIAN_POINT('Ctrl Pts',(-41.8448486400326,20.5529756002056,-21.1251855964591));
#34691=CARTESIAN_POINT('Ctrl Pts',(-44.6192557971265,20.9435908393615,-30.0463497312518));
#34692=CARTESIAN_POINT('Ctrl Pts',(-44.5900546737109,20.9358615047579,-29.8937793939917));
#34693=CARTESIAN_POINT('Ctrl Pts',(-44.5608535502954,20.9281321701544,-29.7412090567315));
#34694=CARTESIAN_POINT('Ctrl Pts',(-44.5316524268797,20.9204028355509,-29.5886387194714));
#34695=CARTESIAN_POINT('Ctrl Pts',(-41.6115400853208,20.1474693751975,-14.3316049934558));
#34696=CARTESIAN_POINT('Ctrl Pts',(-29.138210899356,20.0812550388979,-1.52559743671482));
#34697=CARTESIAN_POINT('Ctrl Pts',(-14.0127168543002,19.8399463130827,1.960201331136));
#34698=CARTESIAN_POINT('Ctrl Pts',(-44.6192837493325,20.9469886892296,-30.0462588269131));
#34699=CARTESIAN_POINT('Ctrl Pts',(-44.5900898599601,20.9392720585054,-29.8936849146578));
#34700=CARTESIAN_POINT('Ctrl Pts',(-44.5608959705877,20.9315554277811,-29.7411110024025));
#34701=CARTESIAN_POINT('Ctrl Pts',(-44.5317020812152,20.9238387970569,-29.5885370901472));
#34702=CARTESIAN_POINT('Ctrl Pts',(-41.6123131439728,20.1521757246323,-14.331145864618));
#34703=CARTESIAN_POINT('Ctrl Pts',(-29.1385639877428,20.0873688943554,-1.52532137413304));
#34704=CARTESIAN_POINT('Ctrl Pts',(-14.0131984274678,19.8474084919615,1.96069388785016));
#34705=CARTESIAN_POINT('Ctrl Pts',(-44.6193117015385,20.9503865390978,-30.0461679225743));
#34706=CARTESIAN_POINT('Ctrl Pts',(-44.5901250462092,20.9426826122528,-29.8935904353239));
#34707=CARTESIAN_POINT('Ctrl Pts',(-44.56093839088,20.9349786854078,-29.7410129480734));
#34708=CARTESIAN_POINT('Ctrl Pts',(-44.5317517355507,20.9272747585629,-29.588435460823));
#34709=CARTESIAN_POINT('Ctrl Pts',(-41.6130862026247,20.1568820740671,-14.3306867357802));
#34710=CARTESIAN_POINT('Ctrl Pts',(-29.1389170761296,20.093482749813,-1.52504531155125));
#34711=CARTESIAN_POINT('Ctrl Pts',(-14.0136800006353,19.8548706708402,1.96118644456431));
#34712=CARTESIAN_POINT('Ctrl Pts',(-44.6193396537445,20.9537843889659,-30.0460770182355));
#34713=CARTESIAN_POINT('Ctrl Pts',(-44.5901602324584,20.9460931660003,-29.8934959559899));
#34714=CARTESIAN_POINT('Ctrl Pts',(-44.5609808111723,20.9384019430346,-29.7409148937444));
#34715=CARTESIAN_POINT('Ctrl Pts',(-44.5318013898862,20.9307107200689,-29.5883338314988));
#34716=CARTESIAN_POINT('Ctrl Pts',(-41.6138592612767,20.1615884235019,-14.3302276069424));
#34717=CARTESIAN_POINT('Ctrl Pts',(-29.1392701645165,20.0995966052706,-1.52476924896946));
#34718=CARTESIAN_POINT('Ctrl Pts',(-14.0141615738029,19.862332849719,1.96167900127847));
#34719=CARTESIAN_POINT('Ctrl Pts',(-44.6194245372235,20.9641027630587,-30.0458009657286));
#34720=CARTESIAN_POINT('Ctrl Pts',(-44.590267083819,20.9564501184246,-29.8932090471655));
#34721=CARTESIAN_POINT('Ctrl Pts',(-44.5611096304145,20.9487974737906,-29.7406171286024));
#34722=CARTESIAN_POINT('Ctrl Pts',(-44.53195217701,20.9411448291565,-29.5880252100392));
#34723=CARTESIAN_POINT('Ctrl Pts',(-41.61620683656,20.1758803657488,-14.3288333537267));
#34724=CARTESIAN_POINT('Ctrl Pts',(-29.1403424008437,20.1181627721728,-1.52393091970171));
#34725=CARTESIAN_POINT('Ctrl Pts',(-14.0156239845298,19.8849935193208,1.96317476614031));
#34726=CARTESIAN_POINT('Ctrl Pts',(-44.6195943039941,20.9847395112521,-30.0452488605024));
#34727=CARTESIAN_POINT('Ctrl Pts',(-44.5904807864153,20.9771640232786,-29.892635229375));
#34728=CARTESIAN_POINT('Ctrl Pts',(-44.5613672688365,20.9695885353052,-29.7400215982477));
#34729=CARTESIAN_POINT('Ctrl Pts',(-44.5322537512578,20.9620130473318,-29.5874079671203));
#34730=CARTESIAN_POINT('Ctrl Pts',(-41.6209019933817,20.2044642499886,-14.326044854383));
#34731=CARTESIAN_POINT('Ctrl Pts',(-29.142486871632,20.1552951062578,-1.52225425630454));
#34732=CARTESIAN_POINT('Ctrl Pts',(-14.0185488059837,19.9303148585245,1.96616629586402));
#34733=CARTESIAN_POINT('Ctrl Pts',(-44.6198489420188,21.0156946339229,-30.0444206880632));
#34734=CARTESIAN_POINT('Ctrl Pts',(-44.5908013322223,21.0082348808134,-29.891774492956));
#34735=CARTESIAN_POINT('Ctrl Pts',(-44.5617537224258,21.000775127704,-29.7391282978488));
#34736=CARTESIAN_POINT('Ctrl Pts',(-44.5327061126293,20.9933153745945,-29.5864821027416));
#34737=CARTESIAN_POINT('Ctrl Pts',(-41.6279451329777,20.2473400636495,-14.3218625920227));
#34738=CARTESIAN_POINT('Ctrl Pts',(-29.1457034681185,20.2109936225946,-1.51973895748648));
#34739=CARTESIAN_POINT('Ctrl Pts',(-14.0229360381646,19.9982968673298,1.97065359044955));
#34740=CARTESIAN_POINT('Ctrl Pts',(-44.6201035640659,21.0466497571015,-30.0435924964379));
#34741=CARTESIAN_POINT('Ctrl Pts',(-44.5911218673776,21.0393057386868,-29.8909137437463));
#34742=CARTESIAN_POINT('Ctrl Pts',(-44.5621401706893,21.0319617202721,-29.7382349910547));
#34743=CARTESIAN_POINT('Ctrl Pts',(-44.5331584740009,21.0246177018574,-29.5855562383631));
#34744=CARTESIAN_POINT('Ctrl Pts',(-41.6349888051667,20.2902158603888,-14.317680969202));
#34745=CARTESIAN_POINT('Ctrl Pts',(-29.1489199175254,20.2666921589687,-1.51722325780471));
#34746=CARTESIAN_POINT('Ctrl Pts',(-14.0273232703454,20.0662788761352,1.97514088503509));
#34747=CARTESIAN_POINT('Ctrl Pts',(-44.6202733040188,21.0672865061488,-30.0430403590245));
#34748=CARTESIAN_POINT('Ctrl Pts',(-44.5913355520954,21.0600196441101,-29.8903399044977));
#34749=CARTESIAN_POINT('Ctrl Pts',(-44.562397800172,21.0527527820714,-29.7376394499708));
#34750=CARTESIAN_POINT('Ctrl Pts',(-44.5334600482486,21.0454859200326,-29.584938995444));
#34751=CARTESIAN_POINT('Ctrl Pts',(-41.6396848559067,20.3187997161584,-14.3148935427609));
#34752=CARTESIAN_POINT('Ctrl Pts',(-29.151064141164,20.3038245267329,-1.5155459213784));
#34753=CARTESIAN_POINT('Ctrl Pts',(-14.0302480917993,20.1116002153389,1.97813241475879));
#34754=CARTESIAN_POINT('Ctrl Pts',(-44.6203581739018,21.0776048806767,-30.0427642902148));
#34755=CARTESIAN_POINT('Ctrl Pts',(-44.591442394392,21.0703765968246,-29.8900529848047));
#34756=CARTESIAN_POINT('Ctrl Pts',(-44.5625266148822,21.0631483129724,-29.7373416793946));
#34757=CARTESIAN_POINT('Ctrl Pts',(-44.5336108353724,21.0559200291202,-29.5846303739845));
#34758=CARTESIAN_POINT('Ctrl Pts',(-41.6420328843933,20.3330916439037,-14.3134998329725));
#34759=CARTESIAN_POINT('Ctrl Pts',(-29.1521362519135,20.3223907107576,-1.51470725069692));
#34760=CARTESIAN_POINT('Ctrl Pts',(-14.0317105025263,20.1342608849406,1.97962817962064));
#34761=CARTESIAN_POINT('Ctrl Pts',(-44.6203663519816,21.0785991614118,-30.0427376881664));
#34762=CARTESIAN_POINT('Ctrl Pts',(-44.5914526897381,21.0713745949617,-29.8900253371629));
#34763=CARTESIAN_POINT('Ctrl Pts',(-44.5625390274948,21.0641500285117,-29.7373129861594));
#34764=CARTESIAN_POINT('Ctrl Pts',(-44.5336253652514,21.0569254620617,-29.5846006351559));
#34765=CARTESIAN_POINT('Ctrl Pts',(-41.6422591409111,20.3344688170607,-14.3133655348048));
#34766=CARTESIAN_POINT('Ctrl Pts',(-29.1522395607303,20.3241797521467,-1.51462643621404));
#34767=CARTESIAN_POINT('Ctrl Pts',(-14.0318514207308,20.1364444718193,1.97977231183664));
#34768=CARTESIAN_POINT('Ctrl Pts',(-44.6203745300613,21.0795934421468,-30.042711086118));
#34769=CARTESIAN_POINT('Ctrl Pts',(-44.5914629850843,21.0723725930989,-29.8899976895211));
#34770=CARTESIAN_POINT('Ctrl Pts',(-44.5625514401073,21.0651517440511,-29.7372842929242));
#34771=CARTESIAN_POINT('Ctrl Pts',(-44.5336398951302,21.0579308950032,-29.5845708963273));
#34772=CARTESIAN_POINT('Ctrl Pts',(-41.6424853974288,20.3358459902176,-14.3132312366371));
#34773=CARTESIAN_POINT('Ctrl Pts',(-29.1523428695472,20.3259687935359,-1.51454562173116));
#34774=CARTESIAN_POINT('Ctrl Pts',(-14.0319923389354,20.1386280586979,1.97991644405265));
#34775=CARTESIAN_POINT('Ctrl Pts',(-44.620382708141,21.0805877228818,-30.0426844840695));
#34776=CARTESIAN_POINT('Ctrl Pts',(-44.5914732804304,21.0733705912361,-29.8899700418792));
#34777=CARTESIAN_POINT('Ctrl Pts',(-44.5625638527198,21.0661534595904,-29.7372555996889));
#34778=CARTESIAN_POINT('Ctrl Pts',(-44.5336544250092,21.0589363279447,-29.5845411574986));
#34779=CARTESIAN_POINT('Ctrl Pts',(-41.6427116539466,20.3372231633746,-14.3130969384694));
#34780=CARTESIAN_POINT('Ctrl Pts',(-29.152446178364,20.327757834925,-1.51446480724828));
#34781=CARTESIAN_POINT('Ctrl Pts',(-14.03213325714,20.1408116455766,1.98006057626865));
#34782=CARTESIAN_POINT('',(-41.8448486400327,20.5529756002067,-21.125185596459));
#34783=CARTESIAN_POINT('Ctrl Pts',(-2.30431969428901,21.2883239772394,-54.9614594276758));
#34784=CARTESIAN_POINT('Ctrl Pts',(-2.60925515681931,21.2711623310641,-54.6300210443754));
#34785=CARTESIAN_POINT('Ctrl Pts',(-2.90976919678355,21.2542807820542,-54.2925838115906));
#34786=CARTESIAN_POINT('Ctrl Pts',(-4.17259771949928,21.1834525291307,-52.8271650732017));
#34787=CARTESIAN_POINT('Ctrl Pts',(-5.96614078384086,21.0834264338425,-50.5049177591858));
#34788=CARTESIAN_POINT('Ctrl Pts',(-8.23551887565116,20.9598507183575,-46.8200324861014));
#34789=CARTESIAN_POINT('Ctrl Pts',(-10.3917998591798,20.8461335954997,-42.3247528309648));
#34790=CARTESIAN_POINT('Ctrl Pts',(-11.9336389677477,20.7684839093916,-37.6328489259993));
#34791=CARTESIAN_POINT('Ctrl Pts',(-12.8608056432646,20.7206230093664,-32.8175597616776));
#34792=CARTESIAN_POINT('Ctrl Pts',(-13.2962652334972,20.6916936542703,-27.9427190446355));
#34793=CARTESIAN_POINT('Ctrl Pts',(-13.1172637173845,20.6796111419738,-23.042397384734));
#34794=CARTESIAN_POINT('Ctrl Pts',(-12.3245180251463,20.6722203558656,-18.190077858897));
#34795=CARTESIAN_POINT('Ctrl Pts',(-11.2247049129228,20.6630225594897,-14.0974459439554));
#34796=CARTESIAN_POINT('Ctrl Pts',(-10.2117545439491,20.6508204531822,-11.4357140304342));
#34797=CARTESIAN_POINT('Ctrl Pts',(-9.45356552143072,20.6394053700742,-9.71398247664349));
#34798=CARTESIAN_POINT('Ctrl Pts',(-9.2653103465393,20.6364191357732,-9.30449670135436));
#34799=CARTESIAN_POINT('Ctrl Pts',(-9.0708504506859,20.6332209087108,-8.89876866574359));
#34800=CARTESIAN_POINT('Ctrl Pts',(-2.78786144780353,21.2398788304839,-54.734986648491));
#34801=CARTESIAN_POINT('Ctrl Pts',(-3.09054674124275,21.2217224127637,-54.4028694868473));
#34802=CARTESIAN_POINT('Ctrl Pts',(-3.38879132187344,21.2038412173392,-54.0647741544324));
#34803=CARTESIAN_POINT('Ctrl Pts',(-4.64185221060926,21.1287309618461,-52.5966368693792));
#34804=CARTESIAN_POINT('Ctrl Pts',(-6.42010193270706,21.0222253289507,-50.2710574808013));
#34805=CARTESIAN_POINT('Ctrl Pts',(-8.6657758353777,20.8890564489947,-46.5837358359478));
#34806=CARTESIAN_POINT('Ctrl Pts',(-10.7937946739521,20.7641817659416,-42.0886817979723));
#34807=CARTESIAN_POINT('Ctrl Pts',(-12.3069696347546,20.6752847595175,-37.4009341484086));
#34808=CARTESIAN_POINT('Ctrl Pts',(-13.2056001710523,20.6159219251614,-32.593875126352));
#34809=CARTESIAN_POINT('Ctrl Pts',(-13.6129162346445,20.5752144761384,-27.7305920467752));
#34810=CARTESIAN_POINT('Ctrl Pts',(-13.4066122237822,20.5509334123338,-22.8460826300547));
#34811=CARTESIAN_POINT('Ctrl Pts',(-12.5879285743064,20.5308579865904,-18.0139735024298));
#34812=CARTESIAN_POINT('Ctrl Pts',(-11.4670654551122,20.510426256151,-13.9417473429775));
#34813=CARTESIAN_POINT('Ctrl Pts',(-10.441017302005,20.4905046142392,-11.2957311335189));
#34814=CARTESIAN_POINT('Ctrl Pts',(-9.67457087624675,20.4739374093561,-9.58505126521439));
#34815=CARTESIAN_POINT('Ctrl Pts',(-9.48435985345334,20.469713411733,-9.17824321596247));
#34816=CARTESIAN_POINT('Ctrl Pts',(-9.2879705742477,20.4652767483487,-8.7752182278677));
#34817=CARTESIAN_POINT('Ctrl Pts',(-3.27157466622819,21.1822016013635,-54.5083686162039));
#34818=CARTESIAN_POINT('Ctrl Pts',(-3.57199026498769,21.1630886105529,-54.1755741433477));
#34819=CARTESIAN_POINT('Ctrl Pts',(-3.867945357497,21.1442460408093,-53.8368225496259));
#34820=CARTESIAN_POINT('Ctrl Pts',(-5.11115096322305,21.0650173413637,-52.3659763157366));
#34821=CARTESIAN_POINT('Ctrl Pts',(-6.87397448879546,20.9522796229575,-50.0370826487369));
#34822=CARTESIAN_POINT('Ctrl Pts',(-9.09574496106366,20.8098799445818,-46.3473629383914));
#34823=CARTESIAN_POINT('Ctrl Pts',(-11.1952649174008,20.6742608619688,-41.8525956339481));
#34824=CARTESIAN_POINT('Ctrl Pts',(-12.6795277371662,20.5745198093833,-37.1690907037834));
#34825=CARTESIAN_POINT('Ctrl Pts',(-13.549357274074,20.5040526001987,-32.3703795244388));
#34826=CARTESIAN_POINT('Ctrl Pts',(-13.928244644041,20.4519664047462,-27.5188030016408));
#34827=CARTESIAN_POINT('Ctrl Pts',(-13.6943252090186,20.4158956934967,-22.6502962432811));
#34828=CARTESIAN_POINT('Ctrl Pts',(-12.84935865861,20.3835681705302,-17.8386311771449));
#34829=CARTESIAN_POINT('Ctrl Pts',(-11.7071209683214,20.3523071857454,-13.7870404729825));
#34830=CARTESIAN_POINT('Ctrl Pts',(-10.6677427713326,20.3249607749065,-11.1569060982881));
#34831=CARTESIAN_POINT('Ctrl Pts',(-9.89288025107589,20.3034475984546,-9.45738932777788));
#34832=CARTESIAN_POINT('Ctrl Pts',(-9.70067558073745,20.2980359714688,-9.05328776689231));
#34833=CARTESIAN_POINT('Ctrl Pts',(-9.502319413209,20.29241155197,-8.65299653157533));
#34834=CARTESIAN_POINT('Ctrl Pts',(-5.00075672518562,20.942701117012,-53.6979980175762));
#34835=CARTESIAN_POINT('Ctrl Pts',(-5.29299497875376,20.9203083949833,-53.3627895497372));
#34836=CARTESIAN_POINT('Ctrl Pts',(-5.58069899267371,20.898168919688,-53.0217006865309));
#34837=CARTESIAN_POINT('Ctrl Pts',(-6.78837683302675,20.8048139743737,-51.5412148799487));
#34838=CARTESIAN_POINT('Ctrl Pts',(-8.49560417926637,20.6706999592586,-49.2005507523738));
#34839=CARTESIAN_POINT('Ctrl Pts',(-10.6312465418532,20.496623371127,-45.5024117366326));
#34840=CARTESIAN_POINT('Ctrl Pts',(-12.6280792027309,20.3241023157428,-41.0089019403645));
#34841=CARTESIAN_POINT('Ctrl Pts',(-14.0081323264445,20.1870685788371,-36.3408814186532));
#34842=CARTESIAN_POINT('Ctrl Pts',(-14.7740833823745,20.0783595881962,-31.5724358370727));
#34843=CARTESIAN_POINT('Ctrl Pts',(-15.050345615672,19.9870599496472,-26.7632388302389));
#34844=CARTESIAN_POINT('Ctrl Pts',(-14.716602165243,19.9103458023656,-21.9526114892868));
#34845=CARTESIAN_POINT('Ctrl Pts',(-13.7764534706996,19.8358125374395,-17.2148494062985));
#34846=CARTESIAN_POINT('Ctrl Pts',(-12.5566475355216,19.767331746443,-13.2378259159173));
#34847=CARTESIAN_POINT('Ctrl Pts',(-11.4687854770212,19.7145309927478,-10.6650386217668));
#34848=CARTESIAN_POINT('Ctrl Pts',(-10.6632684791928,19.6760973304852,-9.00580897579432));
#34849=CARTESIAN_POINT('Ctrl Pts',(-10.4638019355425,19.6666248028076,-8.61148427775603));
#34850=CARTESIAN_POINT('Ctrl Pts',(-10.2582811126764,19.6569408091057,-8.22107717923549));
#34851=CARTESIAN_POINT('Ctrl Pts',(-7.46361100628468,20.4780024533914,-52.5428514904373));
#34852=CARTESIAN_POINT('Ctrl Pts',(-7.74396251989346,20.4514551579611,-52.2042338877599));
#34853=CARTESIAN_POINT('Ctrl Pts',(-8.01966600566118,20.4251375618498,-51.8598495527096));
#34854=CARTESIAN_POINT('Ctrl Pts',(-9.17564362561465,20.3138746691076,-50.3657973352887));
#34855=CARTESIAN_POINT('Ctrl Pts',(-10.8019893466219,20.1526659052326,-48.0086692011363));
#34856=CARTESIAN_POINT('Ctrl Pts',(-12.8123729854089,19.938389785095,-44.2991483331433));
#34857=CARTESIAN_POINT('Ctrl Pts',(-14.6598833650052,19.7189203495023,-39.8083335665313));
#34858=CARTESIAN_POINT('Ctrl Pts',(-15.8883904533384,19.5342279169114,-35.1635209475294));
#34859=CARTESIAN_POINT('Ctrl Pts',(-16.5032185242019,19.3763677050182,-30.4395979969074));
#34860=CARTESIAN_POINT('Ctrl Pts',(-16.6301079290243,19.2344308170631,-25.6923932190953));
#34861=CARTESIAN_POINT('Ctrl Pts',(-16.150942601219,19.1049298841923,-20.9661119486891));
#34862=CARTESIAN_POINT('Ctrl Pts',(-15.071952261372,18.9752993129734,-16.3358067118265));
#34863=CARTESIAN_POINT('Ctrl Pts',(-13.7388416841064,18.8580619466085,-12.4670750288679));
#34864=CARTESIAN_POINT('Ctrl Pts',(-12.5800312173463,18.7718242877839,-9.97749611367835));
#34865=CARTESIAN_POINT('Ctrl Pts',(-11.7296051602899,18.7111415689428,-8.37669984088804));
#34866=CARTESIAN_POINT('Ctrl Pts',(-11.5195014970783,18.6963263828107,-7.99657495662887));
#34867=CARTESIAN_POINT('Ctrl Pts',(-11.3034879690696,18.6812985797984,-7.62054189991676));
#34868=CARTESIAN_POINT('Ctrl Pts',(-11.0569415256315,19.4355555088431,-50.8552329684943));
#34869=CARTESIAN_POINT('Ctrl Pts',(-11.3192343320996,19.4044605226273,-50.5116606355265));
#34870=CARTESIAN_POINT('Ctrl Pts',(-11.5766912052793,19.3735658358572,-50.1625007339047));
#34871=CARTESIAN_POINT('Ctrl Pts',(-12.653995917516,19.2426748194849,-48.6488552478595));
#34872=CARTESIAN_POINT('Ctrl Pts',(-14.1573023261151,19.0517849995255,-46.2681979540424));
#34873=CARTESIAN_POINT('Ctrl Pts',(-15.9771942148807,18.7933185397158,-42.5433868704522));
#34874=CARTESIAN_POINT('Ctrl Pts',(-17.597612542223,18.5218580841843,-38.0587382248537));
#34875=CARTESIAN_POINT('Ctrl Pts',(-18.5955579184473,18.2836948825759,-33.4509227879516));
#34876=CARTESIAN_POINT('Ctrl Pts',(-18.9802606649373,18.0697821020849,-28.7960392710661));
#34877=CARTESIAN_POINT('Ctrl Pts',(-18.8794585829925,17.8693333343866,-24.1441381552406));
#34878=CARTESIAN_POINT('Ctrl Pts',(-18.1782482378414,17.6778661310593,-19.5467704498198));
#34879=CARTESIAN_POINT('Ctrl Pts',(-16.8867429791504,17.4826662284719,-15.0801299557059));
#34880=CARTESIAN_POINT('Ctrl Pts',(-15.3797696484439,17.3068805329357,-11.3760221291961));
#34881=CARTESIAN_POINT('Ctrl Pts',(-14.1117405005934,17.1802068447994,-9.0127555471549));
#34882=CARTESIAN_POINT('Ctrl Pts',(-13.1920422418364,17.0925519552341,-7.50061046136997));
#34883=CARTESIAN_POINT('Ctrl Pts',(-12.965539839746,17.0712544126695,-7.14207420900537));
#34884=CARTESIAN_POINT('Ctrl Pts',(-12.733360180583,17.0497370990139,-6.78793828427621));
#34885=CARTESIAN_POINT('Ctrl Pts',(-15.1119097686709,17.8320672383652,-48.9488137829308));
#34886=CARTESIAN_POINT('Ctrl Pts',(-15.3529931425318,17.7976045693245,-48.5995837467735));
#34887=CARTESIAN_POINT('Ctrl Pts',(-15.5889976518167,17.7633163796081,-48.2449887280201));
#34888=CARTESIAN_POINT('Ctrl Pts',(-16.5737137552487,17.6178640028275,-46.7091305060896));
#34889=CARTESIAN_POINT('Ctrl Pts',(-17.9322327728079,17.4049846203341,-44.3020244766142));
#34890=CARTESIAN_POINT('Ctrl Pts',(-19.5279513167919,17.1135517229592,-40.5609220746071));
#34891=CARTESIAN_POINT('Ctrl Pts',(-20.8810506766434,16.8027253827761,-36.0853303795502));
#34892=CARTESIAN_POINT('Ctrl Pts',(-21.6074270786827,16.523022337621,-31.5226206762998));
#34893=CARTESIAN_POINT('Ctrl Pts',(-21.7208002337218,16.2641978724915,-26.950312603897));
#34894=CARTESIAN_POINT('Ctrl Pts',(-21.3512579632507,16.0157341831644,-22.4117014626838));
#34895=CARTESIAN_POINT('Ctrl Pts',(-20.3875400600326,15.7719994721116,-17.9669301842299));
#34896=CARTESIAN_POINT('Ctrl Pts',(-18.8442287628299,15.5202180684676,-13.6935287962594));
#34897=CARTESIAN_POINT('Ctrl Pts',(-17.1307828365004,15.2931736272884,-10.1835212283731));
#34898=CARTESIAN_POINT('Ctrl Pts',(-15.7326823378276,15.130708702949,-7.96902663040391));
#34899=CARTESIAN_POINT('Ctrl Pts',(-14.7303426130687,15.0190926843839,-6.56125019998718));
#34900=CARTESIAN_POINT('Ctrl Pts',(-14.4843031082476,14.9920326361705,-6.22819169107344));
#34901=CARTESIAN_POINT('Ctrl Pts',(-14.232891211722,14.9647422323135,-5.8999558309418));
#34902=CARTESIAN_POINT('Ctrl Pts',(-18.970908270454,15.7638142683891,-47.1328184999909));
#34903=CARTESIAN_POINT('Ctrl Pts',(-19.1907412698361,15.7283726072843,-46.7780154330218));
#34904=CARTESIAN_POINT('Ctrl Pts',(-19.4052286980466,15.6930928161318,-46.4180868298392));
#34905=CARTESIAN_POINT('Ctrl Pts',(-20.2969793577773,15.543379415412,-44.8605288213155));
#34906=CARTESIAN_POINT('Ctrl Pts',(-21.510103862618,15.3241289383934,-42.4277782313556));
#34907=CARTESIAN_POINT('Ctrl Pts',(-22.8806049730129,15.0227233638938,-38.6716539324935));
#34908=CARTESIAN_POINT('Ctrl Pts',(-23.9649653230345,14.6988957424381,-34.2066804509099));
#34909=CARTESIAN_POINT('Ctrl Pts',(-24.4180458113406,14.4035050799014,-29.6907449133417));
#34910=CARTESIAN_POINT('Ctrl Pts',(-24.2579799735948,14.1252237593235,-25.2027953528283));
#34911=CARTESIAN_POINT('Ctrl Pts',(-23.6172443794943,13.8539516979883,-20.7793517379232));
#34912=CARTESIAN_POINT('Ctrl Pts',(-22.3880897501917,13.5829362127958,-16.4891755568032));
#34913=CARTESIAN_POINT('Ctrl Pts',(-20.5895002890963,13.2994842764397,-12.4111363639204));
#34914=CARTESIAN_POINT('Ctrl Pts',(-18.6662036034684,13.0425486753816,-9.09713537144141));
#34915=CARTESIAN_POINT('Ctrl Pts',(-17.1354921955775,12.8585920936854,-7.03274207893589));
#34916=CARTESIAN_POINT('Ctrl Pts',(-16.048739648028,12.7324540777387,-5.73022824514736));
#34917=CARTESIAN_POINT('Ctrl Pts',(-15.7827885451181,12.7018988467546,-5.42292608178293));
#34918=CARTESIAN_POINT('Ctrl Pts',(-15.5118211192701,12.6711030837425,-5.12093005973719));
#34919=CARTESIAN_POINT('Ctrl Pts',(-22.5969658936558,13.2592937677246,-45.4258711593088));
#34920=CARTESIAN_POINT('Ctrl Pts',(-22.7957177855766,13.2252177231213,-45.0654769225982));
#34921=CARTESIAN_POINT('Ctrl Pts',(-22.9888377624845,13.191306123502,-44.7002131505109));
#34922=CARTESIAN_POINT('Ctrl Pts',(-23.7881792480622,13.0474600457288,-43.1210272437177));
#34923=CARTESIAN_POINT('Ctrl Pts',(-24.8567080894127,12.8372075593629,-40.6627647663409));
#34924=CARTESIAN_POINT('Ctrl Pts',(-26.0029935116187,12.5484949329477,-36.8918909076659));
#34925=CARTESIAN_POINT('Ctrl Pts',(-26.8195147395495,12.2377054846042,-32.4379437041746));
#34926=CARTESIAN_POINT('Ctrl Pts',(-26.9998173751933,11.9522310106351,-27.9693078951154));
#34927=CARTESIAN_POINT('Ctrl Pts',(-26.5663869056578,11.6797819251771,-23.5663639192412));
#34928=CARTESIAN_POINT('Ctrl Pts',(-25.6541474279455,11.4108111467242,-19.2588329729169));
#34929=CARTESIAN_POINT('Ctrl Pts',(-24.1587280567503,11.1374939458242,-15.12412018789));
#34930=CARTESIAN_POINT('Ctrl Pts',(-22.1034644686606,10.8473681096278,-11.2424340363213));
#34931=CARTESIAN_POINT('Ctrl Pts',(-19.9687094955924,10.5820480444149,-8.12537223739529));
#34932=CARTESIAN_POINT('Ctrl Pts',(-18.3040278835727,10.3910369789073,-6.21175695472705));
#34933=CARTESIAN_POINT('Ctrl Pts',(-17.1318696035033,10.2599216927486,-5.01496871371572));
#34934=CARTESIAN_POINT('Ctrl Pts',(-16.845831430263,10.2281653805015,-4.73358189890223));
#34935=CARTESIAN_POINT('Ctrl Pts',(-16.5551956536855,10.1961599190035,-4.45802969804284));
#34936=CARTESIAN_POINT('Ctrl Pts',(-26.0167061432083,10.420684636249,-43.8161837189555));
#34937=CARTESIAN_POINT('Ctrl Pts',(-26.1946291832305,10.3898269637342,-43.4501190170891));
#34938=CARTESIAN_POINT('Ctrl Pts',(-26.3666176764586,10.3591499865554,-43.079458719461));
#34939=CARTESIAN_POINT('Ctrl Pts',(-27.0744900734894,10.2291883131935,-41.4784672756312));
#34940=CARTESIAN_POINT('Ctrl Pts',(-27.999808981558,10.0401067219452,-38.9944407782196));
#34941=CARTESIAN_POINT('Ctrl Pts',(-28.9237686887517,9.78206378055234,-35.20850249419));
#34942=CARTESIAN_POINT('Ctrl Pts',(-29.474407698267,9.50499638561923,-30.7652910285251));
#34943=CARTESIAN_POINT('Ctrl Pts',(-29.3835473154896,9.24981780003299,-26.343762915146));
#34944=CARTESIAN_POINT('Ctrl Pts',(-28.6779829078192,9.00337535985762,-22.0257324189637));
#34945=CARTESIAN_POINT('Ctrl Pts',(-27.4951432333356,8.75677479408939,-17.8341016659244));
#34946=CARTESIAN_POINT('Ctrl Pts',(-25.73393053778,8.50116890088297,-13.8549385098536));
#34947=CARTESIAN_POINT('Ctrl Pts',(-23.4220006890394,8.22444592813344,-10.1697877782279));
#34948=CARTESIAN_POINT('Ctrl Pts',(-21.0754636537987,7.96804930448713,-7.24988582865412));
#34949=CARTESIAN_POINT('Ctrl Pts',(-19.2763679910782,7.78162503245108,-5.48723735239392));
#34950=CARTESIAN_POINT('Ctrl Pts',(-18.0184348821575,7.65323614745839,-4.39631216064967));
#34951=CARTESIAN_POINT('Ctrl Pts',(-17.7122933135742,7.62212996336316,-4.14090141603417));
#34952=CARTESIAN_POINT('Ctrl Pts',(-17.4020440680749,7.59076668565169,-3.89187867255944));
#34953=CARTESIAN_POINT('Ctrl Pts',(-29.153478657498,7.18298363715391,-42.3405988972462));
#34954=CARTESIAN_POINT('Ctrl Pts',(-29.3110150080358,7.15763661423686,-41.968710532368));
#34955=CARTESIAN_POINT('Ctrl Pts',(-29.4623028504942,7.13250342173354,-41.5925157737493));
#34956=CARTESIAN_POINT('Ctrl Pts',(-30.0804996917727,7.02634360727853,-39.9692026543914));
#34957=CARTESIAN_POINT('Ctrl Pts',(-30.8652738685615,6.87350147707393,-37.4586487692798));
#34958=CARTESIAN_POINT('Ctrl Pts',(-31.570631702725,6.66841421880391,-33.6565856487172));
#34959=CARTESIAN_POINT('Ctrl Pts',(-31.8593828840731,6.45075222930465,-29.2229740367431));
#34960=CARTESIAN_POINT('Ctrl Pts',(-31.5008821225295,6.25122984378583,-24.8475460187101));
#34961=CARTESIAN_POINT('Ctrl Pts',(-30.5261914416043,6.05595707526583,-20.6135492497893));
#34962=CARTESIAN_POINT('Ctrl Pts',(-29.0753280478855,5.8568061689083,-16.5370395810716));
#34963=CARTESIAN_POINT('Ctrl Pts',(-27.0503371471076,5.64398234710963,-12.7127701150548));
#34964=CARTESIAN_POINT('Ctrl Pts',(-24.4831672830312,5.40587468584602,-9.22361623976366));
#34965=CARTESIAN_POINT('Ctrl Pts',(-21.9256568997423,5.18017895256177,-6.50048971464225));
#34966=CARTESIAN_POINT('Ctrl Pts',(-19.9924050455866,5.01301666232781,-4.88860082735946));
#34967=CARTESIAN_POINT('Ctrl Pts',(-18.6487730514648,4.89707445701614,-3.90341761267217));
#34968=CARTESIAN_POINT('Ctrl Pts',(-18.3226214021972,4.86894780999335,-3.6739618069591));
#34969=CARTESIAN_POINT('Ctrl Pts',(-17.9929253405265,4.84055053954568,-3.45145291255317));
#34970=CARTESIAN_POINT('Ctrl Pts',(-31.9690930439721,3.57357815210241,-41.0180792529404));
#34971=CARTESIAN_POINT('Ctrl Pts',(-32.1068917240552,3.55599962931061,-40.6401207805861));
#34972=CARTESIAN_POINT('Ctrl Pts',(-32.2381219635969,3.53868515668548,-40.2581553674421));
#34973=CARTESIAN_POINT('Ctrl Pts',(-32.7693658218617,3.46609807861293,-38.6115622659731));
#34974=CARTESIAN_POINT('Ctrl Pts',(-33.4176633186792,3.36435917107101,-36.0730433066292));
#34975=CARTESIAN_POINT('Ctrl Pts',(-33.9101935588516,3.23426720235262,-32.2527904354527));
#34976=CARTESIAN_POINT('Ctrl Pts',(-33.9433875335791,3.10147907156715,-27.8264773869434));
#34977=CARTESIAN_POINT('Ctrl Pts',(-33.3230442294874,2.98285053627008,-23.4949825382079));
#34978=CARTESIAN_POINT('Ctrl Pts',(-32.0844634781661,2.86388130857434,-19.342983262472));
#34979=CARTESIAN_POINT('Ctrl Pts',(-30.3703524340721,2.73730530568202,-15.3796595222941));
#34980=CARTESIAN_POINT('Ctrl Pts',(-28.0857727571174,2.59247375589619,-11.7084699295552));
#34981=CARTESIAN_POINT('Ctrl Pts',(-25.2669562806955,2.41842603756845,-8.41361075233248));
#34982=CARTESIAN_POINT('Ctrl Pts',(-22.5011430936133,2.24547053120763,-5.88587199558128));
#34983=CARTESIAN_POINT('Ctrl Pts',(-20.4352434834371,2.11246131963295,-4.423861375631));
#34984=CARTESIAN_POINT('Ctrl Pts',(-19.0068166510242,2.01884144332686,-3.54385338001933));
#34985=CARTESIAN_POINT('Ctrl Pts',(-18.6609406970972,1.99605339732081,-3.34020224802802));
#34986=CARTESIAN_POINT('Ctrl Pts',(-18.3121499863602,1.9729679754383,-3.14404091243222));
#34987=CARTESIAN_POINT('Ctrl Pts',(-34.1445283674067,0.237308438758995,
-39.9981929654655));
#34988=CARTESIAN_POINT('Ctrl Pts',(-34.2659507766525,0.227921876287717,
-39.6148155006927));
#34989=CARTESIAN_POINT('Ctrl Pts',(-34.3805279861517,0.218854274805993,
-39.2276946514564));
#34990=CARTESIAN_POINT('Ctrl Pts',(-34.8395344608935,0.181679983795775,
-37.5602873097401));
#34991=CARTESIAN_POINT('Ctrl Pts',(-35.3742864588916,0.133848323063104,
-34.996502923227));
#34992=CARTESIAN_POINT('Ctrl Pts',(-35.689296702141,0.0830496793456984,
-31.158781314165));
#34993=CARTESIAN_POINT('Ctrl Pts',(-35.508860093127,0.0403924264632703,
-26.7366100715681));
#34994=CARTESIAN_POINT('Ctrl Pts',(-34.6691074999777,0.00837005963384143,
-22.4407523838643));
#34995=CARTESIAN_POINT('Ctrl Pts',(-33.2089581147195,-0.0279539839125438,
-18.3571071296996));
#34996=CARTESIAN_POINT('Ctrl Pts',(-31.2735021578734,-0.0750512999789021,
-14.4889393778444));
#34997=CARTESIAN_POINT('Ctrl Pts',(-28.77030238607,-0.14423024726241,-10.9471823477048));
#34998=CARTESIAN_POINT('Ctrl Pts',(-25.7392642180907,-0.245792879606331,
-7.81715607344157));
#34999=CARTESIAN_POINT('Ctrl Pts',(-22.7976079423453,-0.358291148292244,
-5.45547658199914));
#35000=CARTESIAN_POINT('Ctrl Pts',(-20.6196310618627,-0.451704594358635,
-4.12101639283359));
#35001=CARTESIAN_POINT('Ctrl Pts',(-19.1195316867098,-0.519340602547392,
-3.33056337659497));
#35002=CARTESIAN_POINT('Ctrl Pts',(-18.7570395705057,-0.535923052101836,
-3.14886314137711));
#35003=CARTESIAN_POINT('Ctrl Pts',(-18.3922183482205,-0.552841667182328,
-2.97509251221366));
#35004=CARTESIAN_POINT('Ctrl Pts',(-35.4242625444563,-2.14030259993981,
-39.3999067907448));
#35005=CARTESIAN_POINT('Ctrl Pts',(-35.5351906676675,-2.14321532053782,
-39.0127533168375));
#35006=CARTESIAN_POINT('Ctrl Pts',(-35.6390899705067,-2.14576465810466,
-38.6220306854052));
#35007=CARTESIAN_POINT('Ctrl Pts',(-36.0517533718566,-2.15494826818845,
-36.9400382714986));
#35008=CARTESIAN_POINT('Ctrl Pts',(-36.513530409794,-2.16016260296573,-34.3583397184339));
#35009=CARTESIAN_POINT('Ctrl Pts',(-36.7140964838328,-2.1481556077715,-30.5074117705083));
#35010=CARTESIAN_POINT('Ctrl Pts',(-36.3955751956867,-2.11918777525101,
-26.0862334557496));
#35011=CARTESIAN_POINT('Ctrl Pts',(-35.4136079539949,-2.08197924289826,
-21.812429632092));
#35012=CARTESIAN_POINT('Ctrl Pts',(-33.8095227208381,-2.05170003121316,
-17.7727099144858));
#35013=CARTESIAN_POINT('Ctrl Pts',(-31.7300551335314,-2.03426137368081,
-13.9663813266482));
#35014=CARTESIAN_POINT('Ctrl Pts',(-29.0843808269317,-2.04135770257883,
-10.5093678461129));
#35015=CARTESIAN_POINT('Ctrl Pts',(-25.9148616326331,-2.08278583441843,
-7.48773188556975));
#35016=CARTESIAN_POINT('Ctrl Pts',(-22.8583671131416,-2.14471303148954,
-5.23550264905522));
#35017=CARTESIAN_POINT('Ctrl Pts',(-20.6071497187297,-2.20477046252904,
-3.98525510992991));
#35018=CARTESIAN_POINT('Ctrl Pts',(-19.0602046224515,-2.25046208753918,
-3.25396976945851));
#35019=CARTESIAN_POINT('Ctrl Pts',(-18.6868772548584,-2.26180965939547,
-3.08675753401129));
#35020=CARTESIAN_POINT('Ctrl Pts',(-18.3116275119647,-2.27353152926925,
-2.92775054349675));
#35021=CARTESIAN_POINT('Ctrl Pts',(-36.2458754281875,-3.83428286431684,
-39.0165372468892));
#35022=CARTESIAN_POINT('Ctrl Pts',(-36.3497179357597,-3.83237339034492,
-38.6267050482277));
#35023=CARTESIAN_POINT('Ctrl Pts',(-36.4464049450996,-3.83006698099443,
-38.2334239905326));
#35024=CARTESIAN_POINT('Ctrl Pts',(-36.827755913052,-3.81839846831683,-36.5410559830271));
#35025=CARTESIAN_POINT('Ctrl Pts',(-37.2401729585333,-3.79185933798401,
-33.9465304329049));
#35026=CARTESIAN_POINT('Ctrl Pts',(-37.3631874453177,-3.73301479320489,
-30.0858254407128));
#35027=CARTESIAN_POINT('Ctrl Pts',(-36.9509520321193,-3.65055513724086,
-25.6645975154325));
#35028=CARTESIAN_POINT('Ctrl Pts',(-35.8723140298153,-3.56151400652134,
-21.4053271089361));
#35029=CARTESIAN_POINT('Ctrl Pts',(-34.170266900352,-3.48120332570528,-17.3952827734835));
#35030=CARTESIAN_POINT('Ctrl Pts',(-31.9927051724745,-3.41513875248544,
-13.6310298223079));
#35031=CARTESIAN_POINT('Ctrl Pts',(-29.2499014363018,-3.37526128513496,
-10.2319449785824));
#35032=CARTESIAN_POINT('Ctrl Pts',(-25.9859204297108,-3.37099617994084,
-7.28460114094662));
#35033=CARTESIAN_POINT('Ctrl Pts',(-22.8510661243058,-3.39437469848804,
-5.10749779158423));
#35034=CARTESIAN_POINT('Ctrl Pts',(-20.5498647319002,-3.42893690611626,
-3.91511396280375));
#35035=CARTESIAN_POINT('Ctrl Pts',(-18.9709493935299,-3.45783930783476,
-3.22450080356909));
#35036=CARTESIAN_POINT('Ctrl Pts',(-18.5902381355287,-3.46518513130081,
-3.06723973368515));
#35037=CARTESIAN_POINT('Ctrl Pts',(-18.2078921549279,-3.47293757911652,
-2.91836533081347));
#35038=CARTESIAN_POINT('Ctrl Pts',(-36.4655794448433,-4.30636894546118,
-38.9141058712393));
#35039=CARTESIAN_POINT('Ctrl Pts',(-36.5674940832915,-4.3031084050989,-38.5235258839868));
#35040=CARTESIAN_POINT('Ctrl Pts',(-36.6622180197793,-4.29944065268701,
-38.1295298100554));
#35041=CARTESIAN_POINT('Ctrl Pts',(-37.0350431681583,-4.28192251284736,
-36.4342583416843));
#35042=CARTESIAN_POINT('Ctrl Pts',(-37.4340027033603,-4.24645759656194,
-33.8361337960593));
#35043=CARTESIAN_POINT('Ctrl Pts',(-37.5358283873113,-4.17439213330946,
-29.9726517814578));
#35044=CARTESIAN_POINT('Ctrl Pts',(-37.0979456046996,-4.07676875425951,
-25.5513313272549));
#35045=CARTESIAN_POINT('Ctrl Pts',(-35.9928116326167,-3.97294922980807,
-21.296010801273));
#35046=CARTESIAN_POINT('Ctrl Pts',(-34.2638927997542,-3.87828739688684,
-17.2941090731212));
#35047=CARTESIAN_POINT('Ctrl Pts',(-32.0594214767088,-3.79820251809058,
-13.5414254218137));
#35048=CARTESIAN_POINT('Ctrl Pts',(-29.2899822669843,-3.74469501429227,
-10.1582784319748));
#35049=CARTESIAN_POINT('Ctrl Pts',(-26.0001245878037,-3.72710099262819,
-7.23136065579539));
#35050=CARTESIAN_POINT('Ctrl Pts',(-22.843837540975,-3.7392015362719,-5.07488539244714));
#35051=CARTESIAN_POINT('Ctrl Pts',(-20.5289842613135,-3.76629674044718,
-3.89837054749424));
#35052=CARTESIAN_POINT('Ctrl Pts',(-18.9413452630501,-3.79028538091932,
-3.21890267223375));
#35053=CARTESIAN_POINT('Ctrl Pts',(-18.558620753541,-3.79646095010219,-3.06436626748395));
#35054=CARTESIAN_POINT('Ctrl Pts',(-18.1743414502133,-3.80305340259771,
-2.9182640862329));
#35055=CARTESIAN_POINT('Ctrl Pts',(-36.6775857957588,-4.78145508078572,
-38.8153455871797));
#35056=CARTESIAN_POINT('Ctrl Pts',(-36.7776062638762,-4.77682808742727,
-38.4240131371284));
#35057=CARTESIAN_POINT('Ctrl Pts',(-36.8704007885924,-4.7717826224726,-38.0292964530863));
#35058=CARTESIAN_POINT('Ctrl Pts',(-37.234843496037,-4.74834091216943,-36.3310936653698));
#35059=CARTESIAN_POINT('Ctrl Pts',(-37.6205540771554,-4.70381966688121,
-33.729326641453));
#35060=CARTESIAN_POINT('Ctrl Pts',(-37.7014739516717,-4.61828583278682,
-29.8630026526442));
#35061=CARTESIAN_POINT('Ctrl Pts',(-37.2382435623926,-4.50515190400754,
-25.4415155647569));
#35062=CARTESIAN_POINT('Ctrl Pts',(-36.10688371564,-4.38613315046716,-21.190074076811));
#35063=CARTESIAN_POINT('Ctrl Pts',(-34.3513451208948,-4.27662792828432,
-17.1962429261849));
#35064=CARTESIAN_POINT('Ctrl Pts',(-32.1202148359084,-4.18197237106197,
-13.4550487006667));
#35065=CARTESIAN_POINT('Ctrl Pts',(-29.3243976191462,-4.11421750462538,
-10.0877374299455));
#35066=CARTESIAN_POINT('Ctrl Pts',(-26.0089405061619,-4.08262421860679,
-7.18109960770556));
#35067=CARTESIAN_POINT('Ctrl Pts',(-22.8314832033504,-4.0828488851085,-5.04507681792322));
#35068=CARTESIAN_POINT('Ctrl Pts',(-20.5031646226372,-4.10207414795096,
-3.88427613292033));
#35069=CARTESIAN_POINT('Ctrl Pts',(-18.9069293129407,-4.12088738197538,
-3.2158356955667));
#35070=CARTESIAN_POINT('Ctrl Pts',(-18.5222216096196,-4.12583098108427,
-3.0639936442264));
#35071=CARTESIAN_POINT('Ctrl Pts',(-18.1360384644055,-4.13120272145022,
-2.92063144712372));
#35072=CARTESIAN_POINT('',(-9.59372125972938,20.7105311502984,-45.8827377044908));
#35073=CARTESIAN_POINT('Ctrl Pts',(-9.5937212597294,20.7105311502984,-45.8827377044908));
#35074=CARTESIAN_POINT('Ctrl Pts',(-11.9656966255223,20.5483438544848,-41.273662205894));
#35075=CARTESIAN_POINT('Ctrl Pts',(-13.4213771307776,20.4520245495079,-36.2040060452052));
#35076=CARTESIAN_POINT('Ctrl Pts',(-14.4263273756746,20.3052748660675,-25.8880364474773));
#35077=CARTESIAN_POINT('Ctrl Pts',(-13.978485237413,20.248474007324,-20.6405355948745));
#35078=CARTESIAN_POINT('Ctrl Pts',(-12.5441843191278,20.1925493450898,-15.6634703684439));
#35079=CARTESIAN_POINT('',(-37.032580314656,-3.27137091447505,-28.7376553268898));
#35080=CARTESIAN_POINT('Ctrl Pts',(-9.59372125972839,20.7105311502992,-45.8827377044852));
#35081=CARTESIAN_POINT('Ctrl Pts',(-12.689974521814,19.9641940681955,-45.2353349371288));
#35082=CARTESIAN_POINT('Ctrl Pts',(-15.6237739429307,18.7336189223951,-44.2899044956698));
#35083=CARTESIAN_POINT('Ctrl Pts',(-21.3095375661309,15.6437709263415,-41.8792648939248));
#35084=CARTESIAN_POINT('Ctrl Pts',(-24.0969041079348,13.6706054953475,-40.3166248003805));
#35085=CARTESIAN_POINT('Ctrl Pts',(-28.9050095453594,9.45712578015132,-37.0129844875419));
#35086=CARTESIAN_POINT('Ctrl Pts',(-31.0016800075678,7.182688558081,-35.2467154850527));
#35087=CARTESIAN_POINT('Ctrl Pts',(-34.5055399597611,2.26699026933606,-31.8194310502729));
#35088=CARTESIAN_POINT('Ctrl Pts',(-35.9295603487439,-0.36522399219569,
-30.1590544146936));
#35089=CARTESIAN_POINT('Ctrl Pts',(-37.0325806584272,-3.27137053313469,
-28.7376548139838));
#35090=CARTESIAN_POINT('Ctrl Pts',(-37.0325798368516,-3.27137100135122,
-28.7376553603834));
#35091=CARTESIAN_POINT('Ctrl Pts',(-36.9761954831548,-3.25992112204953,
-27.9630010274032));
#35092=CARTESIAN_POINT('Ctrl Pts',(-36.8905408508367,-3.24789096533568,
-27.1935900368743));
#35093=CARTESIAN_POINT('Ctrl Pts',(-36.7763506206657,-3.23555894384663,
-26.4309495822826));
#35094=CARTESIAN_POINT('Ctrl Pts',(-36.4966946574327,-3.20535738156791,
-24.5632157962139));
#35095=CARTESIAN_POINT('Ctrl Pts',(-36.0458884752206,-3.17334534347451,
-22.7360903115206));
#35096=CARTESIAN_POINT('Ctrl Pts',(-35.4348689964149,-3.14345008158506,
-20.9719738284514));
#35097=CARTESIAN_POINT('Ctrl Pts',(-35.0275226565476,-3.12351990598109,
-19.7958961134128));
#35098=CARTESIAN_POINT('Ctrl Pts',(-34.5489703998561,-3.10453051989494,
-18.6478224019152));
#35099=CARTESIAN_POINT('Ctrl Pts',(-34.0024927143669,-3.08752071373526,
-17.5343714336233));
#35100=CARTESIAN_POINT('Ctrl Pts',(-33.4560150291637,-3.07051090758448,
-16.4209204659143));
#35101=CARTESIAN_POINT('Ctrl Pts',(-32.8416119152349,-3.0554806813514,-15.342092241367));
#35102=CARTESIAN_POINT('Ctrl Pts',(-32.162579197906,-3.04339100491456,-14.3044960466025));
#35103=CARTESIAN_POINT('Ctrl Pts',(-31.1440301231784,-3.02525649028182,
-12.74810175639));
#35104=CARTESIAN_POINT('Ctrl Pts',(-29.9800644412201,-3.01373821257335,
-11.284479532925));
#35105=CARTESIAN_POINT('Ctrl Pts',(-28.6818918835157,-3.01128625574909,
-9.93585464417003));
#35106=CARTESIAN_POINT('Ctrl Pts',(-27.8164435137448,-3.00965161787008,
-9.03677138711117));
#35107=CARTESIAN_POINT('Ctrl Pts',(-26.891347643875,-3.01204645592803,-8.18879805630125));
#35108=CARTESIAN_POINT('Ctrl Pts',(-25.9099387717161,-3.01891855380822,
-7.39849523212083));
#35109=CARTESIAN_POINT('Ctrl Pts',(-24.9285300172334,-3.02579065086441,
-6.60819250270197));
#35110=CARTESIAN_POINT('Ctrl Pts',(-23.8908082739512,-3.03714000665748,
-5.87556026604573));
#35111=CARTESIAN_POINT('Ctrl Pts',(-22.8001058140645,-3.05321938564873,
-5.20714428357849));
#35112=CARTESIAN_POINT('Ctrl Pts',(-22.3506640922016,-3.05984515577954,
-4.93171258599896));
#35113=CARTESIAN_POINT('Ctrl Pts',(-21.8922263256852,-3.06727406915266,
-4.66718473035009));
#35114=CARTESIAN_POINT('Ctrl Pts',(-21.4250255310232,-3.07550335254719,
-4.41401723611861));
#35115=CARTESIAN_POINT('Ctrl Pts',(-36.8218388167228,-4.68328060676847,
-38.751295439731));
#35116=CARTESIAN_POINT('Ctrl Pts',(-36.9217087088858,-4.67927906663786,
-38.3585621385122));
#35117=CARTESIAN_POINT('Ctrl Pts',(-37.014288976107,-4.67486342687383,-37.962433466881));
#35118=CARTESIAN_POINT('Ctrl Pts',(-37.3764699113101,-4.65418501649615,
-36.2631808787972));
#35119=CARTESIAN_POINT('Ctrl Pts',(-37.7581985948115,-4.61395560865182,
-33.6622303832942));
#35120=CARTESIAN_POINT('Ctrl Pts',(-37.8331190147459,-4.53496565777432,
-29.7973573317513));
#35121=CARTESIAN_POINT('Ctrl Pts',(-37.3628812674897,-4.42959393838223,
-25.3778345391439));
#35122=CARTESIAN_POINT('Ctrl Pts',(-36.2245349411945,-4.31850354734918,
-21.1287082650676));
#35123=CARTESIAN_POINT('Ctrl Pts',(-34.4620735486552,-4.2170896233612,-17.1375634223537));
#35124=CARTESIAN_POINT('Ctrl Pts',(-32.224084021324,-4.13063759391767,-13.3993703876313));
#35125=CARTESIAN_POINT('Ctrl Pts',(-29.421520970621,-4.07121155600733,-10.0354694255977));
#35126=CARTESIAN_POINT('Ctrl Pts',(-26.0994749828814,-4.04803120464602,
-7.13267369659695));
#35127=CARTESIAN_POINT('Ctrl Pts',(-22.9164994170118,-4.055480889925,-5.00025025831193));
#35128=CARTESIAN_POINT('Ctrl Pts',(-20.5846089679859,-4.07952578289679,
-3.84205015737256));
#35129=CARTESIAN_POINT('Ctrl Pts',(-18.9840129497197,-4.10152925776619,
-3.17453027868918));
#35130=CARTESIAN_POINT('Ctrl Pts',(-18.5967019960699,-4.1072571624472,-3.02235727198848));
#35131=CARTESIAN_POINT('Ctrl Pts',(-18.2079217603241,-4.11341014061892,
-2.87876106338383));
#35132=CARTESIAN_POINT('Ctrl Pts',(-36.5588964654534,-4.24009445412503,
-38.8740584245357));
#35133=CARTESIAN_POINT('Ctrl Pts',(-36.6608783697925,-4.23725223817857,
-38.4820550867501));
#35134=CARTESIAN_POINT('Ctrl Pts',(-36.755609154871,-4.23400446880359,-38.0866187243054));
#35135=CARTESIAN_POINT('Ctrl Pts',(-37.1271020213035,-4.21832863439708,
-36.3901431019892));
#35136=CARTESIAN_POINT('Ctrl Pts',(-37.52349683041,-4.18572164472913,-33.7925669388741));
#35137=CARTESIAN_POINT('Ctrl Pts',(-37.6214603144111,-4.11799618192084,
-29.9300480653258));
#35138=CARTESIAN_POINT('Ctrl Pts',(-37.1790710704798,-4.02550335874969,
-25.5100196056566));
#35139=CARTESIAN_POINT('Ctrl Pts',(-36.0694515065602,-3.92690475481451,
-21.2562075949406));
#35140=CARTESIAN_POINT('Ctrl Pts',(-34.3360977835797,-3.83755718932749,
-17.2560411757399));
#35141=CARTESIAN_POINT('Ctrl Pts',(-32.1272437511178,-3.76285616468038,
-13.5052822838444));
#35142=CARTESIAN_POINT('Ctrl Pts',(-29.3535072956654,-3.71481495977278,
-10.1243046163367));
#35143=CARTESIAN_POINT('Ctrl Pts',(-26.0594639791076,-3.70275434803773,
-7.19981235881089));
#35144=CARTESIAN_POINT('Ctrl Pts',(-22.8996775036204,-3.71962751323487,
-5.04559718311213));
#35145=CARTESIAN_POINT('Ctrl Pts',(-20.5825598194173,-3.74992063397164,
-3.87071007387643));
#35146=CARTESIAN_POINT('Ctrl Pts',(-18.9914165768469,-3.77604797989279,
-3.19148231513987));
#35147=CARTESIAN_POINT('Ctrl Pts',(-18.606295054631,-3.78276245762616,-3.03643732004868));
#35148=CARTESIAN_POINT('Ctrl Pts',(-18.2196164583466,-3.78989370687861,
-2.88992075118384));
#35149=CARTESIAN_POINT('Ctrl Pts',(-36.290673376604,-3.80075287541765,-38.9993534436856));
#35150=CARTESIAN_POINT('Ctrl Pts',(-36.3947878507366,-3.79905339336963,
-38.6080734652654));
#35151=CARTESIAN_POINT('Ctrl Pts',(-36.4916895026568,-3.79695621683146,
-38.2133222519409));
#35152=CARTESIAN_POINT('Ctrl Pts',(-36.872579939312,-3.78620663871065,-36.5195907613128));
#35153=CARTESIAN_POINT('Ctrl Pts',(-37.2837599710986,-3.76109400159902,
-33.9253412532604));
#35154=CARTESIAN_POINT('Ctrl Pts',(-37.4049126075535,-3.70440674399875,
-30.0651155870792));
#35155=CARTESIAN_POINT('Ctrl Pts',(-36.9905070830313,-3.62448835210827,
-25.6445247857299));
#35156=CARTESIAN_POINT('Ctrl Pts',(-35.9097128452123,-3.53802316526296,
-21.3859911440621));
#35157=CARTESIAN_POINT('Ctrl Pts',(-34.2055389888196,-3.46032715355504,
-17.376786716545));
#35158=CARTESIAN_POINT('Ctrl Pts',(-32.025881660209,-3.39690914788247,-13.6134581369143));
#35159=CARTESIAN_POINT('Ctrl Pts',(-29.2810301768391,-3.35971861494906,
-10.2154057282584));
#35160=CARTESIAN_POINT('Ctrl Pts',(-26.0150609941361,-3.35817927654809,
-7.26920630790089));
#35161=CARTESIAN_POINT('Ctrl Pts',(-22.8785479745878,-3.38391914529348,
-5.09316256015692));
#35162=CARTESIAN_POINT('Ctrl Pts',(-20.5762738134618,-3.42007079724739,
-3.90153887791587));
#35163=CARTESIAN_POINT('Ctrl Pts',(-18.9946367288233,-3.45006162272336,
-3.21055807057412));
#35164=CARTESIAN_POINT('Ctrl Pts',(-18.6117176519029,-3.45770043113048,
-3.05262827696875));
#35165=CARTESIAN_POINT('Ctrl Pts',(-18.2271537838515,-3.46574819271174,
-2.903176732322));
#35166=CARTESIAN_POINT('Ctrl Pts',(-35.326274595645,-2.2653457359543,-39.4500974478482));
#35167=CARTESIAN_POINT('Ctrl Pts',(-35.4379808442489,-2.26761569662348,
-39.0613392238265));
#35168=CARTESIAN_POINT('Ctrl Pts',(-35.5426083546314,-2.26951335386862,
-38.6689747224565));
#35169=CARTESIAN_POINT('Ctrl Pts',(-35.9569344920503,-2.27586002752392,
-36.9847938818377));
#35170=CARTESIAN_POINT('Ctrl Pts',(-36.4206636132443,-2.27671432942662,
-34.4020927243131));
#35171=CARTESIAN_POINT('Ctrl Pts',(-36.6240902972401,-2.25814179129592,
-30.5497210056551));
#35172=CARTESIAN_POINT('Ctrl Pts',(-36.3088242271421,-2.2214798205824,-26.1269314979888));
#35173=CARTESIAN_POINT('Ctrl Pts',(-35.3300068268744,-2.17652897108851,
-21.8516114957386));
#35174=CARTESIAN_POINT('Ctrl Pts',(-33.7289661625207,-2.13845241575724,
-17.8104750562544));
#35175=CARTESIAN_POINT('Ctrl Pts',(-31.6524613437962,-2.11316923258448,
-14.0028112042569));
#35176=CARTESIAN_POINT('Ctrl Pts',(-29.0096518231127,-2.11235831802136,
-10.5445663919547));
#35177=CARTESIAN_POINT('Ctrl Pts',(-25.8429103198821,-2.14581153060268,
-7.52180526966867));
#35178=CARTESIAN_POINT('Ctrl Pts',(-22.7887438706414,-2.20085463389179,
-5.26868502893114));
#35179=CARTESIAN_POINT('Ctrl Pts',(-20.5390486779056,-2.25628908058851,
-4.01789268754426));
#35180=CARTESIAN_POINT('Ctrl Pts',(-18.9911128255576,-2.29898278275007,
-3.28532599364926));
#35181=CARTESIAN_POINT('Ctrl Pts',(-18.6160074043562,-2.30966173471912,
-3.11717983531058));
#35182=CARTESIAN_POINT('Ctrl Pts',(-18.2389512637551,-2.32072459453129,
-2.95732567869355));
#35183=CARTESIAN_POINT('Ctrl Pts',(-33.5155942144999,0.42091842584111,-40.2974780341865));
#35184=CARTESIAN_POINT('Ctrl Pts',(-33.6410979392138,0.412015546281074,
-39.9131480760228));
#35185=CARTESIAN_POINT('Ctrl Pts',(-33.7597625875287,0.403442573942463,
-39.5249756224605));
#35186=CARTESIAN_POINT('Ctrl Pts',(-34.2348236846508,0.368526239150617,
-37.8575734340774));
#35187=CARTESIAN_POINT('Ctrl Pts',(-34.793938864872,0.324281374370589,-35.2950638376772));
#35188=CARTESIAN_POINT('Ctrl Pts',(-35.1465248468338,0.279215865745994,
-31.4560451821976));
#35189=CARTESIAN_POINT('Ctrl Pts',(-35.0108071356808,0.243759038204317,
-27.0285126878594));
#35190=CARTESIAN_POINT('Ctrl Pts',(-34.2164710060877,0.21967725703067,-22.7223557888659));
#35191=CARTESIAN_POINT('Ctrl Pts',(-32.8018337863586,0.192114722189047,
-18.6232863589188));
#35192=CARTESIAN_POINT('Ctrl Pts',(-30.9116489876761,0.154437491851918,
-14.7354972118828));
#35193=CARTESIAN_POINT('Ctrl Pts',(-28.4530247891845,0.0954817696064694,
-11.1687518835629));
#35194=CARTESIAN_POINT('Ctrl Pts',(-25.4652872492237,0.0048363712043943,
-8.00819339300858));
#35195=CARTESIAN_POINT('Ctrl Pts',(-22.5596132517522,-0.0979118428630517,
-5.61646217028398));
#35196=CARTESIAN_POINT('Ctrl Pts',(-20.4047003250856,-0.184631554593919,
-4.25932715177338));
#35197=CARTESIAN_POINT('Ctrl Pts',(-18.9175087484012,-0.247909792323189,
-3.45203690874275));
#35198=CARTESIAN_POINT('Ctrl Pts',(-18.5565095119815,-0.263520166061751,
-3.26551414254701));
#35199=CARTESIAN_POINT('Ctrl Pts',(-18.1930293280116,-0.279478515480188,
-3.08692920705276));
#35200=CARTESIAN_POINT('Ctrl Pts',(-30.7058158632503,3.93922736422659,-41.6156780667464));
#35201=CARTESIAN_POINT('Ctrl Pts',(-30.8512244437417,3.92273017306588,-41.2373131455902));
#35202=CARTESIAN_POINT('Ctrl Pts',(-30.9901280488388,3.90651491483579,-40.8547832308081));
#35203=CARTESIAN_POINT('Ctrl Pts',(-31.5527136406494,3.83888692720806,-39.209945734774));
#35204=CARTESIAN_POINT('Ctrl Pts',(-32.2490817339818,3.74496038387833,-36.6743179499844));
#35205=CARTESIAN_POINT('Ctrl Pts',(-32.8157306685883,3.6271896762232,-32.8520021930134));
#35206=CARTESIAN_POINT('Ctrl Pts',(-32.9371004388341,3.50969140214063,-28.415607351119));
#35207=CARTESIAN_POINT('Ctrl Pts',(-32.4062568303131,3.40771510315772,-24.064179586933));
#35208=CARTESIAN_POINT('Ctrl Pts',(-31.2572950158716,3.30695483103527,-19.8820198922113));
#35209=CARTESIAN_POINT('Ctrl Pts',(-29.6322618431089,3.1998573133211,-15.8801579160552));
#35210=CARTESIAN_POINT('Ctrl Pts',(-27.4352928661237,3.07607789704229,-12.1597154252998));
#35211=CARTESIAN_POINT('Ctrl Pts',(-24.7014561356057,2.92448144596071,-8.8045323297206));
#35212=CARTESIAN_POINT('Ctrl Pts',(-22.0061590174955,2.77158317941627,-6.21733539620513));
#35213=CARTESIAN_POINT('Ctrl Pts',(-19.9853803676448,2.65236568914073,-4.71041174116156));
#35214=CARTESIAN_POINT('Ctrl Pts',(-18.584109044878,2.56779645721963,-3.79791853180525));
#35215=CARTESIAN_POINT('Ctrl Pts',(-18.2431180339001,2.54707902977605,-3.58548942342471));
#35216=CARTESIAN_POINT('Ctrl Pts',(-17.8989488792197,2.52604544176493,-3.38046479825666));
#35217=CARTESIAN_POINT('Ctrl Pts',(-27.2065229004271,7.64857049485316,-43.2599712710379));
#35218=CARTESIAN_POINT('Ctrl Pts',(-27.375180737316,7.62538079009264,-42.8882187054049));
#35219=CARTESIAN_POINT('Ctrl Pts',(-27.5377062922894,7.6024320797305,-42.5119551641807));
#35220=CARTESIAN_POINT('Ctrl Pts',(-28.2023793530123,7.50598047950645,-40.8922328334449));
#35221=CARTESIAN_POINT('Ctrl Pts',(-29.0586537190346,7.36825978906471,-38.3863291832077));
#35222=CARTESIAN_POINT('Ctrl Pts',(-29.8741803512828,7.18657585481396,-34.5817019673071));
#35223=CARTESIAN_POINT('Ctrl Pts',(-30.2938961583478,6.99739878870591,-30.1336568230252));
#35224=CARTESIAN_POINT('Ctrl Pts',(-30.0681891276577,6.82819742189185,-25.729106971718));
#35225=CARTESIAN_POINT('Ctrl Pts',(-29.226307184173,6.66543158101024,-21.4507349741909));
#35226=CARTESIAN_POINT('Ctrl Pts',(-27.9073056775005,6.50060855796851,-17.3173530581892));
#35227=CARTESIAN_POINT('Ctrl Pts',(-26.0118012369813,6.32441606849526,-13.420225676104));
#35228=CARTESIAN_POINT('Ctrl Pts',(-23.5699870405407,6.12505774886043,-9.84169230501458));
#35229=CARTESIAN_POINT('Ctrl Pts',(-21.1163074171586,5.93384517916791,-7.0303844759557));
#35230=CARTESIAN_POINT('Ctrl Pts',(-19.24935046319,5.79035915091665,-5.35183470637228));
#35231=CARTESIAN_POINT('Ctrl Pts',(-17.9465329640227,5.69001969995687,-4.3188326702563));
#35232=CARTESIAN_POINT('Ctrl Pts',(-17.6285601762503,5.66551509710643,-4.07669727210146));
#35233=CARTESIAN_POINT('Ctrl Pts',(-17.3066979614427,5.64071489355821,-3.84132255077521));
#35234=CARTESIAN_POINT('Ctrl Pts',(-23.9106075275297,10.6050661536892,-44.8102927658334));
#35235=CARTESIAN_POINT('Ctrl Pts',(-24.0999482352423,10.5777689837161,-44.4441954546609));
#35236=CARTESIAN_POINT('Ctrl Pts',(-24.2834699596018,10.5506896266998,-44.0733056545029));
#35237=CARTESIAN_POINT('Ctrl Pts',(-25.0388108524095,10.4365567481294,-42.4751911006532));
#35238=CARTESIAN_POINT('Ctrl Pts',(-26.0369733432726,10.2719415070743,-39.9947595312251));
#35239=CARTESIAN_POINT('Ctrl Pts',(-27.0729575257367,10.0511774947007,-36.204886014752));
#35240=CARTESIAN_POINT('Ctrl Pts',(-27.7565345002429,9.81863871620139,-31.7458974134181));
#35241=CARTESIAN_POINT('Ctrl Pts',(-27.8001970917429,9.60967367489776,-27.2942342918104));
#35242=CARTESIAN_POINT('Ctrl Pts',(-27.2289251235294,9.41153176383594,-22.9311595449484));
#35243=CARTESIAN_POINT('Ctrl Pts',(-26.1792365799165,9.21500541081661,-18.6822692512467));
#35244=CARTESIAN_POINT('Ctrl Pts',(-24.5485602461104,9.01175979868378,-14.6302206321163));
#35245=CARTESIAN_POINT('Ctrl Pts',(-22.3628067019381,8.78956564702969,-10.8560325847683));
#35246=CARTESIAN_POINT('Ctrl Pts',(-20.1206530946606,8.58124477590158,-7.84850018302945));
#35247=CARTESIAN_POINT('Ctrl Pts',(-18.3881253877929,8.42762540105217,-6.0197322565147));
#35248=CARTESIAN_POINT('Ctrl Pts',(-17.1712672933703,8.32086564673385,-4.88126724545499));
#35249=CARTESIAN_POINT('Ctrl Pts',(-16.873476253482,8.29482075310626,-4.61312950964513));
#35250=CARTESIAN_POINT('Ctrl Pts',(-16.5712568612584,8.26849188852043,-4.35118157863571));
#35251=CARTESIAN_POINT('Ctrl Pts',(-19.9077523571373,13.6252616883324,-46.6938992239532));
#35252=CARTESIAN_POINT('Ctrl Pts',(-20.1209446867673,13.5952855444977,-46.3342027946698));
#35253=CARTESIAN_POINT('Ctrl Pts',(-20.328655271869,13.5655149131873,-45.9694174486435));
#35254=CARTESIAN_POINT('Ctrl Pts',(-21.1883542692841,13.4398628522405,-44.3959569514256));
#35255=CARTESIAN_POINT('Ctrl Pts',(-22.3497277547974,13.2576618204372,-41.944601857953));
#35256=CARTESIAN_POINT('Ctrl Pts',(-23.6389889994787,13.0115743729063,-38.1716237995733));
#35257=CARTESIAN_POINT('Ctrl Pts',(-24.6253432650482,12.751644575675,-33.700270230942));
#35258=CARTESIAN_POINT('Ctrl Pts',(-24.9776401721497,12.5189796899122,-29.195033885056));
#35259=CARTESIAN_POINT('Ctrl Pts',(-24.7159386768495,12.301865256328,-24.7355540748207));
#35260=CARTESIAN_POINT('Ctrl Pts',(-23.973932481888,12.0904144587841,-20.3551525544938));
#35261=CARTESIAN_POINT('Ctrl Pts',(-22.6452804926613,11.8774764455751,-16.1266720944649));
#35262=CARTESIAN_POINT('Ctrl Pts',(-20.7509637909255,11.6504923923572,-12.1296170528026));
#35263=CARTESIAN_POINT('Ctrl Pts',(-18.7491181417974,11.4410171343385,-8.89853855417975));
#35264=CARTESIAN_POINT('Ctrl Pts',(-17.1689877263805,11.2882220371981,-6.89861628429694));
#35265=CARTESIAN_POINT('Ctrl Pts',(-16.0494601752109,11.1823584691134,-5.63998274787565));
#35266=CARTESIAN_POINT('Ctrl Pts',(-15.7746139887752,11.1565388193505,-5.34224033696405));
#35267=CARTESIAN_POINT('Ctrl Pts',(-15.4948206145188,11.1304479812224,-5.05005712611216));
#35268=CARTESIAN_POINT('Ctrl Pts',(-16.2180432174767,15.9398275064074,-48.4301828651543));
#35269=CARTESIAN_POINT('Ctrl Pts',(-16.4521938275456,15.9092719019138,-48.076086901104));
#35270=CARTESIAN_POINT('Ctrl Pts',(-16.6811358152299,15.8789225535602,-47.7166629869837));
#35271=CARTESIAN_POINT('Ctrl Pts',(-17.6323385975404,15.7507918597713,-46.1649547628248));
#35272=CARTESIAN_POINT('Ctrl Pts',(-18.936758193489,15.5646999212503,-43.7393392481435));
#35273=CARTESIAN_POINT('Ctrl Pts',(-20.4478002103812,15.3133344724918,-39.9816616098395));
#35274=CARTESIAN_POINT('Ctrl Pts',(-21.6990238014656,15.0487502016962,-35.5001764568839));
#35275=CARTESIAN_POINT('Ctrl Pts',(-22.3209682180315,14.8142492774957,-30.9488592309027));
#35276=CARTESIAN_POINT('Ctrl Pts',(-22.3293422064976,14.5991383033468,-26.4059293305493));
#35277=CARTESIAN_POINT('Ctrl Pts',(-21.8554243838307,14.3930646018661,-21.9114461411382));
#35278=CARTESIAN_POINT('Ctrl Pts',(-20.7894641003817,14.1899609567462,-17.5296852489892));
#35279=CARTESIAN_POINT('Ctrl Pts',(-19.1480898546693,13.977122935371,-13.3388231592936));
#35280=CARTESIAN_POINT('Ctrl Pts',(-17.3543937104353,13.7824369346935,-9.91324173232946));
#35281=CARTESIAN_POINT('Ctrl Pts',(-15.9059529139166,13.6409944051188,-7.76433835467781));
#35282=CARTESIAN_POINT('Ctrl Pts',(-14.8704133561947,13.5429643472183,-6.40108514071164));
#35283=CARTESIAN_POINT('Ctrl Pts',(-14.6154376715172,13.5190447294408,-6.07761083543428));
#35284=CARTESIAN_POINT('Ctrl Pts',(-14.3551373099958,13.4948677704672,-5.75918559466514));
#35285=CARTESIAN_POINT('Ctrl Pts',(-11.822716088486,18.188947172369,-50.4975069982862));
#35286=CARTESIAN_POINT('Ctrl Pts',(-12.0807460479859,18.1597316481657,-50.149900849382));
#35287=CARTESIAN_POINT('Ctrl Pts',(-12.3338504324003,18.1307342364494,-49.7967145807944));
#35288=CARTESIAN_POINT('Ctrl Pts',(-13.3890724600746,18.0083786966032,-48.2704339664839));
#35289=CARTESIAN_POINT('Ctrl Pts',(-14.85607927955,17.830846834045,-45.87512597419));
#35290=CARTESIAN_POINT('Ctrl Pts',(-16.6190813424255,17.5925027676131,-42.1363421540281));
#35291=CARTESIAN_POINT('Ctrl Pts',(-18.1710314843799,17.3443426911773,-37.6450078774674));
#35292=CARTESIAN_POINT('Ctrl Pts',(-19.098835784666,17.1289494695207,-33.042870247926));
#35293=CARTESIAN_POINT('Ctrl Pts',(-19.4131698285569,16.9369213116231,-28.4065295399037));
#35294=CARTESIAN_POINT('Ctrl Pts',(-19.2425984638769,16.7575317657622,-23.7837227318492));
#35295=CARTESIAN_POINT('Ctrl Pts',(-18.4733495985464,16.5859876106103,-19.2289587859595));
#35296=CARTESIAN_POINT('Ctrl Pts',(-17.1170188880216,16.4095763329362,-14.8188969944352));
#35297=CARTESIAN_POINT('Ctrl Pts',(-15.5573630806058,16.2491906636996,-11.1730748288595));
#35298=CARTESIAN_POINT('Ctrl Pts',(-14.2565853340076,16.1323920433636,-8.85532759071016));
#35299=CARTESIAN_POINT('Ctrl Pts',(-13.3150650046537,16.0510402241362,-7.37346260225604));
#35300=CARTESIAN_POINT('Ctrl Pts',(-13.0823954562657,16.0311583490605,-7.02088379334164));
#35301=CARTESIAN_POINT('Ctrl Pts',(-12.8440411184632,16.01103806515,-6.67284079394564));
#35302=CARTESIAN_POINT('Ctrl Pts',(-7.8411699938905,19.7983627848149,-52.3687269376966));
#35303=CARTESIAN_POINT('Ctrl Pts',(-8.11992829303053,19.7720645135703,-52.0269336332472));
#35304=CARTESIAN_POINT('Ctrl Pts',(-8.39398168231564,19.7460021313493,-51.6793544625476));
#35305=CARTESIAN_POINT('Ctrl Pts',(-9.53928451332661,19.6361820466171,-50.1760284730572));
#35306=CARTESIAN_POINT('Ctrl Pts',(-11.14709799416,19.4774394485581,-47.8083359664954));
#35307=CARTESIAN_POINT('Ctrl Pts',(-13.1282713733665,19.2670183310104,-44.0877853258967));
#35308=CARTESIAN_POINT('Ctrl Pts',(-14.9405198598359,19.0520629838802,-39.5898882349583));
#35309=CARTESIAN_POINT('Ctrl Pts',(-16.1328704916667,18.8717166252608,-34.9454307905654));
#35310=CARTESIAN_POINT('Ctrl Pts',(-16.7115351800607,18.7178122962125,-30.2296013374526));
#35311=CARTESIAN_POINT('Ctrl Pts',(-16.8027339787928,18.5794411422907,-25.4968369057016));
#35312=CARTESIAN_POINT('Ctrl Pts',(-16.289068982041,18.4529446490623,-20.7931224538683));
#35313=CARTESIAN_POINT('Ctrl Pts',(-15.1776736379726,18.3257380682571,-16.1937918909369));
#35314=CARTESIAN_POINT('Ctrl Pts',(-13.818636740357,18.2102139945187,-12.3575006396806));
#35315=CARTESIAN_POINT('Ctrl Pts',(-12.6440494074441,18.1249152482566,-9.89355822405953));
#35316=CARTESIAN_POINT('Ctrl Pts',(-11.7827259364293,18.064727637235,-8.30894077759558));
#35317=CARTESIAN_POINT('Ctrl Pts',(-11.5691191440624,18.0499634327475,-7.93121921616813));
#35318=CARTESIAN_POINT('Ctrl Pts',(-11.3495571850093,18.0349776243875,-7.5576561263274));
#35319=CARTESIAN_POINT('Ctrl Pts',(-4.92431549867914,20.6836496418694,-53.7378814684056));
#35320=CARTESIAN_POINT('Ctrl Pts',(-5.21764882463673,20.6606519170286,-53.4003910101086));
#35321=CARTESIAN_POINT('Ctrl Pts',(-5.50641809554749,20.6379063239872,-53.0569754366587));
#35322=CARTESIAN_POINT('Ctrl Pts',(-6.71493902102225,20.5422448076096,-51.5707569872934));
#35323=CARTESIAN_POINT('Ctrl Pts',(-8.42160241882005,20.4047755971079,-49.2238878429916));
#35324=CARTESIAN_POINT('Ctrl Pts',(-10.5559839035698,20.225761668211,-45.5180413008222));
#35325=CARTESIAN_POINT('Ctrl Pts',(-12.5510196597057,20.0475517349526,-41.0174600421653));
#35326=CARTESIAN_POINT('Ctrl Pts',(-13.9290667150874,19.9048724048602,-36.3448359479815));
#35327=CARTESIAN_POINT('Ctrl Pts',(-14.6931006487833,19.790507905872,-31.5743538869703));
#35328=CARTESIAN_POINT('Ctrl Pts',(-14.9676760376565,19.6935273080542,-26.7652261036137));
#35329=CARTESIAN_POINT('Ctrl Pts',(-14.6327324280219,19.6110850660289,-21.9573646480998));
#35330=CARTESIAN_POINT('Ctrl Pts',(-13.6921672345661,19.530779076001,-17.2251601923033));
#35331=CARTESIAN_POINT('Ctrl Pts',(-12.4726763896338,19.4573327991495,-13.2548574676923));
#35332=CARTESIAN_POINT('Ctrl Pts',(-11.3855615935515,19.4012238336331,-10.6878836640295));
#35333=CARTESIAN_POINT('Ctrl Pts',(-10.579708766175,19.3605693891818,-9.03080166569367));
#35334=CARTESIAN_POINT('Ctrl Pts',(-10.3792982715972,19.3505226070412,-8.63539384629041));
#35335=CARTESIAN_POINT('Ctrl Pts',(-10.17275733115,19.3402634731691,-8.24392214707791));
#35336=CARTESIAN_POINT('Ctrl Pts',(-3.28313391958304,21.117312799858,-54.5077715750056));
#35337=CARTESIAN_POINT('Ctrl Pts',(-3.58453926185978,21.0964267127388,-54.1727240990175));
#35338=CARTESIAN_POINT('Ctrl Pts',(-3.88145363778616,21.0758020890032,-53.8316755867277));
#35339=CARTESIAN_POINT('Ctrl Pts',(-5.12494438152081,20.9891913310095,-52.3551981425261));
#35340=CARTESIAN_POINT('Ctrl Pts',(-6.88629963355924,20.8653273744228,-50.0202471636553));
#35341=CARTESIAN_POINT('Ctrl Pts',(-9.10547002832004,20.7063681300896,-46.323055763502));
#35342=CARTESIAN_POINT('Ctrl Pts',(-11.2016741138313,20.5515335415639,-41.8215054727501));
#35343=CARTESIAN_POINT('Ctrl Pts',(-12.6824932627098,20.4326519806542,-37.1336983778281));
#35344=CARTESIAN_POINT('Ctrl Pts',(-13.549084907869,20.3430531321453,-32.3332605226414));
#35345=CARTESIAN_POINT('Ctrl Pts',(-13.9250741545097,20.2718184169426,-27.4820679213417));
#35346=CARTESIAN_POINT('Ctrl Pts',(-13.6888986754112,20.2165549432469,-22.6166458941869));
#35347=CARTESIAN_POINT('Ctrl Pts',(-12.8426375694204,20.164982094833,-17.8108595922544));
#35348=CARTESIAN_POINT('Ctrl Pts',(-11.7000922537864,20.117197691553,-13.7662661051264));
#35349=CARTESIAN_POINT('Ctrl Pts',(-10.6611372059216,20.0788282397779,-11.1421302429153));
#35350=CARTESIAN_POINT('Ctrl Pts',(-9.88579572272463,20.0500302875854,-9.44483158002572));
#35351=CARTESIAN_POINT('Ctrl Pts',(-9.69264545280016,20.0428451797642,-9.03962286423958));
#35352=CARTESIAN_POINT('Ctrl Pts',(-9.49327031140026,20.0354515632684,-8.63824109957652));
#35353=CARTESIAN_POINT('Ctrl Pts',(-2.8163592485811,21.2334813897109,-54.7266862394484));
#35354=CARTESIAN_POINT('Ctrl Pts',(-3.12005132129948,21.2132228077857,-54.3923338233844));
#35355=CARTESIAN_POINT('Ctrl Pts',(-3.41927252450223,21.1932283095702,-54.051958820629));
#35356=CARTESIAN_POINT('Ctrl Pts',(-4.67266466131728,21.1093059289188,-52.578253438475));
#35357=CARTESIAN_POINT('Ctrl Pts',(-6.44950317520521,20.9894835119608,-50.2466975711262));
#35358=CARTESIAN_POINT('Ctrl Pts',(-8.69266751409434,20.8364792943525,-46.5519878921847));
#35359=CARTESIAN_POINT('Ctrl Pts',(-10.8174853479259,20.6885792302246,-42.0502021694425));
#35360=CARTESIAN_POINT('Ctrl Pts',(-12.3273479522208,20.5767478260626,-37.3581435871616));
#35361=CARTESIAN_POINT('Ctrl Pts',(-13.2228929109269,20.4944756050622,-32.5492847655305));
#35362=CARTESIAN_POINT('Ctrl Pts',(-13.6274817449899,20.4308554028779,-27.6862587662835));
#35363=CARTESIAN_POINT('Ctrl Pts',(-13.4191180933562,20.3836340081555,-22.8046364371979));
#35364=CARTESIAN_POINT('Ctrl Pts',(-12.5993630644216,20.340580727313,-17.9781318076291));
#35365=CARTESIAN_POINT('Ctrl Pts',(-11.4784037767259,20.3004356869138,-13.9126108423358));
#35366=CARTESIAN_POINT('Ctrl Pts',(-10.4529327913986,20.2673681898868,-11.272358363803));
#35367=CARTESIAN_POINT('Ctrl Pts',(-9.68612423728318,20.2421246596599,-9.56371335956087));
#35368=CARTESIAN_POINT('Ctrl Pts',(-9.49500452080127,20.2357981340653,-9.15574211803836));
#35369=CARTESIAN_POINT('Ctrl Pts',(-9.29763363791485,20.2292648564311,-8.75156952718668));
#35370=CARTESIAN_POINT('Ctrl Pts',(-2.34821392037626,21.3428689572265,-54.9461960408909));
#35371=CARTESIAN_POINT('Ctrl Pts',(-2.65418949424281,21.323266505305,-54.6125406100865));
#35372=CARTESIAN_POINT('Ctrl Pts',(-2.95571399231871,21.303930781031,-54.2728409939294));
#35373=CARTESIAN_POINT('Ctrl Pts',(-4.21899114535187,21.2228186866547,-52.8019155745608));
#35374=CARTESIAN_POINT('Ctrl Pts',(-6.0112853374839,21.1072213437662,-50.4737675281765));
#35375=CARTESIAN_POINT('Ctrl Pts',(-8.27839193827317,20.9604400919523,-46.7815631436401));
#35376=CARTESIAN_POINT('Ctrl Pts',(-10.4317474491813,20.819779963638,-42.2795772720142));
#35377=CARTESIAN_POINT('Ctrl Pts',(-11.9705535559543,20.7152993064879,-37.5833174183362));
#35378=CARTESIAN_POINT('Ctrl Pts',(-12.8949237610472,20.6406553883908,-32.7661078399796));
#35379=CARTESIAN_POINT('Ctrl Pts',(-13.3279556694048,20.5849601975755,-27.8913403249881));
#35380=CARTESIAN_POINT('Ctrl Pts',(-13.1472110199265,20.5461109852346,-22.9936375250261));
#35381=CARTESIAN_POINT('Ctrl Pts',(-12.353730422049,20.5119420676311,-18.1465609279757));
#35382=CARTESIAN_POINT('Ctrl Pts',(-11.2541276071585,20.4797911688045,-14.0602526474523));
#35383=CARTESIAN_POINT('Ctrl Pts',(-10.2419708153508,20.4522911786996,-11.4039786634214));
#35384=CARTESIAN_POINT('Ctrl Pts',(-9.48357772483115,20.4307901345004,-9.68404750188143));
#35385=CARTESIAN_POINT('Ctrl Pts',(-9.29446059008481,20.4253683033402,-9.27333014503118));
#35386=CARTESIAN_POINT('Ctrl Pts',(-9.09906630802712,20.4197421663948,-8.86638496754931));
#35387=CARTESIAN_POINT('',(-9.57349520052307,20.5529756002067,-45.8869621655533));
#35388=CARTESIAN_POINT('Ctrl Pts',(-37.0325800073215,-3.27137127985419,
-28.7376556530266));
#35389=CARTESIAN_POINT('Ctrl Pts',(-34.5044867351128,1.76302065361439,-31.995465657097));
#35390=CARTESIAN_POINT('Ctrl Pts',(-30.8416008390371,6.26298702225072,-35.7871583427932));
#35391=CARTESIAN_POINT('Ctrl Pts',(-23.5458744462642,12.5188402724799,-40.6337606863442));
#35392=CARTESIAN_POINT('Ctrl Pts',(-20.9044174504492,14.4577038717082,-42.0668269045533));
#35393=CARTESIAN_POINT('Ctrl Pts',(-15.4358826795028,17.848637426394,-44.3535277717808));
#35394=CARTESIAN_POINT('Ctrl Pts',(-12.5747622055328,19.3555632898771,-45.2608009663176));
#35395=CARTESIAN_POINT('Ctrl Pts',(-9.57349520052268,20.5529756002057,-45.8869621655533));
#35396=CARTESIAN_POINT('Ctrl Pts',(-12.693647630517,19.9464420456703,-16.2756753502908));
#35397=CARTESIAN_POINT('Ctrl Pts',(-14.0225517860209,20.0189549105364,-21.1794341117034));
#35398=CARTESIAN_POINT('Ctrl Pts',(-14.4019245709807,20.0954766247834,-26.3285862792967));
#35399=CARTESIAN_POINT('Ctrl Pts',(-13.3354239934069,20.2752040736289,-36.426648889325));
#35400=CARTESIAN_POINT('Ctrl Pts',(-11.8914352859286,20.3824974081049,-41.3760085159638));
#35401=CARTESIAN_POINT('Ctrl Pts',(-9.57349520052296,20.5529756002056,-45.8869621655532));
#35402=CARTESIAN_POINT('Ctrl Pts',(-4.32846278832924,20.9435908393615,-53.6183358849051));
#35403=CARTESIAN_POINT('Ctrl Pts',(-4.42954047863754,20.9358615047579,-53.5003794779475));
#35404=CARTESIAN_POINT('Ctrl Pts',(-4.53061816894586,20.9281321701544,-53.3824230709899));
#35405=CARTESIAN_POINT('Ctrl Pts',(-4.63169585925417,20.9204028355509,-53.2644666640323));
#35406=CARTESIAN_POINT('Ctrl Pts',(-14.7394648900858,20.1474693751975,-41.4688259682726));
#35407=CARTESIAN_POINT('Ctrl Pts',(-16.9746112199935,20.0812550388979,-23.7323694053441));
#35408=CARTESIAN_POINT('Ctrl Pts',(-10.2693271530803,19.8399463130827,-9.7334219899501));
#35409=CARTESIAN_POINT('Ctrl Pts',(-4.32855128811855,20.9469886892296,-53.6183010608916));
#35410=CARTESIAN_POINT('Ctrl Pts',(-4.42963628382275,20.9392720585054,-53.5003480807636));
#35411=CARTESIAN_POINT('Ctrl Pts',(-4.53072127952695,20.9315554277811,-53.3823951006357));
#35412=CARTESIAN_POINT('Ctrl Pts',(-4.63180627523115,20.9238387970569,-53.2644421205078));
#35413=CARTESIAN_POINT('Ctrl Pts',(-14.7403058456515,20.1521757246323,-41.4691441077164));
#35414=CARTESIAN_POINT('Ctrl Pts',(-16.9750472014194,20.0873688943554,-23.7324733387566));
#35415=CARTESIAN_POINT('Ctrl Pts',(-10.2700125053852,19.8474084919615,-9.73349139492549));
#35416=CARTESIAN_POINT('Ctrl Pts',(-4.32863978790787,20.9503865390978,-53.618266236878));
#35417=CARTESIAN_POINT('Ctrl Pts',(-4.42973208900795,20.9426826122528,-53.5003166835798));
#35418=CARTESIAN_POINT('Ctrl Pts',(-4.53082439010804,20.9349786854078,-53.3823671302816));
#35419=CARTESIAN_POINT('Ctrl Pts',(-4.63191669120813,20.9272747585629,-53.2644175769833));
#35420=CARTESIAN_POINT('Ctrl Pts',(-14.7411468012171,20.1568820740671,-41.4694622471602));
#35421=CARTESIAN_POINT('Ctrl Pts',(-16.9754831828453,20.093482749813,-23.7325772721691));
#35422=CARTESIAN_POINT('Ctrl Pts',(-10.27069785769,19.8548706708402,-9.73356079990087));
#35423=CARTESIAN_POINT('Ctrl Pts',(-4.32872828769718,20.9537843889659,-53.6182314128645));
#35424=CARTESIAN_POINT('Ctrl Pts',(-4.42982789419316,20.9460931660003,-53.500285286396));
#35425=CARTESIAN_POINT('Ctrl Pts',(-4.53092750068913,20.9384019430346,-53.3823391599274));
#35426=CARTESIAN_POINT('Ctrl Pts',(-4.63202710718511,20.9307107200689,-53.2643930334589));
#35427=CARTESIAN_POINT('Ctrl Pts',(-14.7419877567828,20.1615884235019,-41.469780386604));
#35428=CARTESIAN_POINT('Ctrl Pts',(-16.9759191642713,20.0995966052706,-23.7326812055816));
#35429=CARTESIAN_POINT('Ctrl Pts',(-10.2713832099948,19.862332849719,-9.73363020487625));
#35430=CARTESIAN_POINT('Ctrl Pts',(-4.3289970382214,20.9641027630587,-53.6181256615179));
#35431=CARTESIAN_POINT('Ctrl Pts',(-4.43011882927837,20.9564501184246,-53.5001899414275));
#35432=CARTESIAN_POINT('Ctrl Pts',(-4.53124062033534,20.9487974737906,-53.3822542213371));
#35433=CARTESIAN_POINT('Ctrl Pts',(-4.63236241139232,20.9411448291565,-53.2643185012467));
#35434=CARTESIAN_POINT('Ctrl Pts',(-14.7445415170896,20.1758803657488,-41.4707464922068));
#35435=CARTESIAN_POINT('Ctrl Pts',(-16.9772431249007,20.1181627721728,-23.7329968239499));
#35436=CARTESIAN_POINT('Ctrl Pts',(-10.2734644442286,19.8849935193208,-9.73384096948556));
#35437=CARTESIAN_POINT('Ctrl Pts',(-4.32953453931903,20.9847395112521,-53.6179141585457));
#35438=CARTESIAN_POINT('Ctrl Pts',(-4.43070069948158,20.9771640232786,-53.4999992513047));
#35439=CARTESIAN_POINT('Ctrl Pts',(-4.53186685964413,20.9695885353052,-53.3820843440637));
#35440=CARTESIAN_POINT('Ctrl Pts',(-4.63303301980668,20.9620130473318,-53.2641694368227));
#35441=CARTESIAN_POINT('Ctrl Pts',(-14.7496490360618,20.2044642499886,-41.4726787127218));
#35442=CARTESIAN_POINT('Ctrl Pts',(-16.979891048797,20.1552951062578,-23.7336280561961));
#35443=CARTESIAN_POINT('Ctrl Pts',(-10.2776269126961,19.9303148585245,-9.7342624987041));
#35444=CARTESIAN_POINT('Ctrl Pts',(-4.33034079481653,21.0156946339229,-53.6175968855001));
#35445=CARTESIAN_POINT('Ctrl Pts',(-4.43157350735379,21.0082348808134,-53.4997132037288));
#35446=CARTESIAN_POINT('Ctrl Pts',(-4.53280621989104,21.000775127704,-53.3818295219576));
#35447=CARTESIAN_POINT('Ctrl Pts',(-4.63403893242831,20.9933153745945,-53.2639458401864));
#35448=CARTESIAN_POINT('Ctrl Pts',(-14.7573101861541,20.2473400636495,-41.475577663063));
#35449=CARTESIAN_POINT('Ctrl Pts',(-16.9838631037067,20.2109936225946,-23.7345746294339));
#35450=CARTESIAN_POINT('Ctrl Pts',(-10.2838706153973,19.9982968673298,-9.73489479253199));
#35451=CARTESIAN_POINT('Ctrl Pts',(-4.33114705535237,21.0466497571015,-53.6172795880003));
#35452=CARTESIAN_POINT('Ctrl Pts',(-4.43244631858488,21.0393057386868,-53.4994271398503));
#35453=CARTESIAN_POINT('Ctrl Pts',(-4.53374558181739,21.0319617202721,-53.3815746917003));
#35454=CARTESIAN_POINT('Ctrl Pts',(-4.6350448450499,21.0246177018574,-53.2637222435503));
#35455=CARTESIAN_POINT('Ctrl Pts',(-14.7649711683006,20.2902158603888,-41.4784774285487));
#35456=CARTESIAN_POINT('Ctrl Pts',(-16.9878353803218,20.2666921589687,-23.735520837746));
#35457=CARTESIAN_POINT('Ctrl Pts',(-10.2901143180985,20.0662788761352,-9.73552708635984));
#35458=CARTESIAN_POINT('Ctrl Pts',(-4.33168456489443,21.0672865061488,-53.6170680439928));
#35459=CARTESIAN_POINT('Ctrl Pts',(-4.43302819441772,21.0600196441101,-53.4992364223706));
#35460=CARTESIAN_POINT('Ctrl Pts',(-4.534371823941,21.0527527820714,-53.3814048007483));
#35461=CARTESIAN_POINT('Ctrl Pts',(-4.63571545346429,21.0454859200326,-53.2635731791261));
#35462=CARTESIAN_POINT('Ctrl Pts',(-14.7700784057928,20.3187997161584,-41.480411016901));
#35463=CARTESIAN_POINT('Ctrl Pts',(-16.9904836763181,20.3038245267329,-23.7361514571359));
#35464=CARTESIAN_POINT('Ctrl Pts',(-10.294276786566,20.1116002153389,-9.73594861557842));
#35465=CARTESIAN_POINT('Ctrl Pts',(-4.33195331968768,21.0776048806767,-53.6169622718518));
#35466=CARTESIAN_POINT('Ctrl Pts',(-4.43331913234895,21.0703765968246,-53.4991410635392));
#35467=CARTESIAN_POINT('Ctrl Pts',(-4.53468494501022,21.0631483129724,-53.3813198552266));
#35468=CARTESIAN_POINT('Ctrl Pts',(-4.63605075767149,21.0559200291202,-53.263498646914));
#35469=CARTESIAN_POINT('Ctrl Pts',(-14.7726320237987,20.3330916439037,-41.4813778156538));
#35470=CARTESIAN_POINT('Ctrl Pts',(-16.9918078255791,20.3223907107576,-23.7364667644556));
#35471=CARTESIAN_POINT('Ctrl Pts',(-10.2963580207998,20.1342608849406,-9.73615938018771));
#35472=CARTESIAN_POINT('Ctrl Pts',(-4.33197921695597,21.0785991614118,-53.6169520796261));
#35473=CARTESIAN_POINT('Ctrl Pts',(-4.43334716718907,21.0713745949617,-53.4991318747422));
#35474=CARTESIAN_POINT('Ctrl Pts',(-4.53471511742217,21.0641500285117,-53.3813116698583));
#35475=CARTESIAN_POINT('Ctrl Pts',(-4.63608306765527,21.0569254620617,-53.2634914649744));
#35476=CARTESIAN_POINT('Ctrl Pts',(-14.7728780909656,20.3344688170607,-41.4814709765845));
#35477=CARTESIAN_POINT('Ctrl Pts',(-16.9919354208798,20.3241797521467,-23.7364971475351));
#35478=CARTESIAN_POINT('Ctrl Pts',(-10.2965585689673,20.1364444718193,-9.73617968950969));
#35479=CARTESIAN_POINT('Ctrl Pts',(-4.33200511422425,21.0795934421468,-53.6169418874004));
#35480=CARTESIAN_POINT('Ctrl Pts',(-4.43337520202918,21.0723725930989,-53.4991226859452));
#35481=CARTESIAN_POINT('Ctrl Pts',(-4.53474528983412,21.0651517440511,-53.38130348449));
#35482=CARTESIAN_POINT('Ctrl Pts',(-4.63611537763905,21.0579308950032,-53.2634842830348));
#35483=CARTESIAN_POINT('Ctrl Pts',(-14.7731241581326,20.3358459902176,-41.4815641375152));
#35484=CARTESIAN_POINT('Ctrl Pts',(-16.9920630161805,20.3259687935359,-23.7365275306146));
#35485=CARTESIAN_POINT('Ctrl Pts',(-10.2967591171349,20.1386280586979,-9.73619999883167));
#35486=CARTESIAN_POINT('Ctrl Pts',(-4.33203101149253,21.0805877228818,-53.6169316951747));
#35487=CARTESIAN_POINT('Ctrl Pts',(-4.43340323686929,21.0733705912361,-53.4991134971482));
#35488=CARTESIAN_POINT('Ctrl Pts',(-4.53477546224606,21.0661534595904,-53.3812952991217));
#35489=CARTESIAN_POINT('Ctrl Pts',(-4.63614768762283,21.0589363279447,-53.2634771010952));
#35490=CARTESIAN_POINT('Ctrl Pts',(-14.7733702252996,20.3372231633746,-41.4816572984459));
#35491=CARTESIAN_POINT('Ctrl Pts',(-16.9921906114812,20.327757834925,-23.7365579136941));
#35492=CARTESIAN_POINT('Ctrl Pts',(-10.2969596653024,20.1408116455766,-9.73622030815366));
#35493=CARTESIAN_POINT('',(-9.57349520052307,20.5529756002067,-45.8869621655533));
#35494=CARTESIAN_POINT('Ctrl Pts',(41.5338854879026,21.2883239772394,-36.0695034689956));
#35495=CARTESIAN_POINT('Ctrl Pts',(41.0846323742273,21.2711623310641,-36.1012631617903));
#35496=CARTESIAN_POINT('Ctrl Pts',(40.6334458830462,21.2542807820542,-36.1258258257493));
#35497=CARTESIAN_POINT('Ctrl Pts',(38.7003746729656,21.1834525291307,-36.1994712829289));
#35498=CARTESIAN_POINT('Ctrl Pts',(35.7665128029796,21.0834264338425,-36.1538221981106));
#35499=CARTESIAN_POINT('Ctrl Pts',(31.4706193903941,20.9598507183575,-35.6306050471236));
#35500=CARTESIAN_POINT('Ctrl Pts',(26.6116490303384,20.8461335954997,-34.5136923836127));
#35501=CARTESIAN_POINT('Ctrl Pts',(21.9820498844225,20.7684839093916,-32.7937965035444));
#35502=CARTESIAN_POINT('Ctrl Pts',(17.6392262517605,20.7206230093664,-30.5164009130032));
#35503=CARTESIAN_POINT('Ctrl Pts',(13.5564176935285,20.6916936542703,-27.8174434572283));
#35504=CARTESIAN_POINT('Ctrl Pts',(9.83679756541101,20.6796111419738,-24.6221938557458));
#35505=CARTESIAN_POINT('Ctrl Pts',(6.53737025169527,20.6722203558656,-20.9770285762437));
#35506=CARTESIAN_POINT('Ctrl Pts',(4.02334403386231,20.6630225594897,-17.5654457985485));
#35507=CARTESIAN_POINT('Ctrl Pts',(2.57388245082573,20.6508204531822,-15.113926606545));
#35508=CARTESIAN_POINT('Ctrl Pts',(1.70050164113498,20.6394053700742,-13.4476684937515));
#35509=CARTESIAN_POINT('Ctrl Pts',(1.49772795208305,20.6364191357732,-13.0451744663849));
#35510=CARTESIAN_POINT('Ctrl Pts',(1.30176076245774,20.6332209087108,-12.6401723051977));
#35511=CARTESIAN_POINT('Ctrl Pts',(41.0553385871247,21.2398788304839,-36.3063481667607));
#35512=CARTESIAN_POINT('Ctrl Pts',(40.6069577406517,21.2217224127637,-36.3359253951444));
#35513=CARTESIAN_POINT('Ctrl Pts',(40.1566717112114,21.2038412173392,-36.3583034059402));
#35514=CARTESIAN_POINT('Ctrl Pts',(38.2275650759369,21.1287309618461,-36.4226172332441));
#35515=CARTESIAN_POINT('Ctrl Pts',(35.3006333280818,21.0222253289507,-36.362933817479));
#35516=CARTESIAN_POINT('Ctrl Pts',(31.0176144035341,20.8890564489947,-35.8196649322046));
#35517=CARTESIAN_POINT('Ctrl Pts',(26.1764415972354,20.7641817659416,-34.6807967040055));
#35518=CARTESIAN_POINT('Ctrl Pts',(21.5679637464527,20.6752847595175,-32.941081673653));
#35519=CARTESIAN_POINT('Ctrl Pts',(17.2493666899064,20.6159219251614,-30.6465070408524));
#35520=CARTESIAN_POINT('Ctrl Pts',(13.1931414583562,20.5752144761384,-27.9327521590155));
#35521=CARTESIAN_POINT('Ctrl Pts',(9.50290666680764,20.5509334123338,-24.7260153799557));
#35522=CARTESIAN_POINT('Ctrl Pts',(6.23545253050602,20.5308579865904,-21.0731719660711));
#35523=CARTESIAN_POINT('Ctrl Pts',(3.75050463941357,20.510426256151,-17.6578544106669));
#35524=CARTESIAN_POINT('Ctrl Pts',(2.32149642341642,20.4905046142392,-15.2058935398892));
#35525=CARTESIAN_POINT('Ctrl Pts',(1.461904576083,20.4739374093561,-13.5400701424733));
#35526=CARTESIAN_POINT('Ctrl Pts',(1.26244386876925,20.469713411733,-13.1377165065184));
#35527=CARTESIAN_POINT('Ctrl Pts',(1.06979295763457,20.4652767483487,-12.7328912152449));
#35528=CARTESIAN_POINT('Ctrl Pts',(40.5765712162756,21.1822016013635,-36.5432363573627));
#35529=CARTESIAN_POINT('Ctrl Pts',(40.1290759580594,21.1630886105529,-36.5706167703566));
#35530=CARTESIAN_POINT('Ctrl Pts',(39.6797043153639,21.1442460408093,-36.5907956150282));
#35531=CARTESIAN_POINT('Ctrl Pts',(37.7546244070558,21.0650173413637,-36.6457152698332));
#35532=CARTESIAN_POINT('Ctrl Pts',(34.834719528204,20.9522796229575,-36.5719047491734));
#35533=CARTESIAN_POINT('Ctrl Pts',(30.564729265643,20.8098799445818,-36.0084522400929));
#35534=CARTESIAN_POINT('Ctrl Pts',(25.7415493990861,20.6742608619688,-34.8474814639788));
#35535=CARTESIAN_POINT('Ctrl Pts',(21.1544150649873,20.5745198093833,-33.0878073038153));
#35536=CARTESIAN_POINT('Ctrl Pts',(16.8603017440869,20.5040526001987,-30.7759199377636));
#35537=CARTESIAN_POINT('Ctrl Pts',(12.8309540677332,20.4519664047462,-28.0472375270115));
#35538=CARTESIAN_POINT('Ctrl Pts',(9.17044859363215,20.4158956934967,-24.8288876342323));
#35539=CARTESIAN_POINT('Ctrl Pts',(5.93536538892685,20.3835681705302,-21.1682420847945));
#35540=CARTESIAN_POINT('Ctrl Pts',(3.4798777735314,20.3523071857454,-17.7490792127145));
#35541=CARTESIAN_POINT('Ctrl Pts',(2.07159762237086,20.3249607749065,-15.2965986559777));
#35542=CARTESIAN_POINT('Ctrl Pts',(1.22598078542615,20.3034475984546,-13.6311553685555));
#35543=CARTESIAN_POINT('Ctrl Pts',(1.02987911483698,20.2980359714688,-13.2289305040802));
#35544=CARTESIAN_POINT('Ctrl Pts',(0.840591872499916,20.29241155197,-12.8242719045711));
#35545=CARTESIAN_POINT('Ctrl Pts',(38.864870590485,20.942701117012,-37.389907526004));
#35546=CARTESIAN_POINT('Ctrl Pts',(38.4205864863258,20.9203083949833,-37.4093895318307));
#35547=CARTESIAN_POINT('Ctrl Pts',(37.974531956119,20.898168919688,-37.4216601598091));
#35548=CARTESIAN_POINT('Ctrl Pts',(36.0640667257951,20.8048139743737,-37.4427929138755));
#35549=CARTESIAN_POINT('Ctrl Pts',(33.1696229811387,20.6706999592586,-37.3181767877764));
#35550=CARTESIAN_POINT('Ctrl Pts',(28.9467502385986,20.496623371127,-36.6821372599687));
#35551=CARTESIAN_POINT('Ctrl Pts',(24.1885780130219,20.3241023157428,-35.4416663669379));
#35552=CARTESIAN_POINT('Ctrl Pts',(19.6785235596824,20.1870685788371,-33.6101721563812));
#35553=CARTESIAN_POINT('Ctrl Pts',(15.4728400094719,20.0783595881962,-31.2359396151031));
#35554=CARTESIAN_POINT('Ctrl Pts',(11.5406116990385,19.9870599496472,-28.4534448376217));
#35555=CARTESIAN_POINT('Ctrl Pts',(7.98759743124033,19.9103458023656,-25.1931366133823));
#35556=CARTESIAN_POINT('Ctrl Pts',(4.86963900159542,19.8358125374395,-21.5041524234108));
#35557=CARTESIAN_POINT('Ctrl Pts',(2.52081339113073,19.767331746443,-18.0708361527821));
#35558=CARTESIAN_POINT('Ctrl Pts',(1.18759818617417,19.7145309927478,-15.6162047066094));
#35559=CARTESIAN_POINT('Ctrl Pts',(0.392591845678522,19.6760973304852,-13.9519133948385));
#35560=CARTESIAN_POINT('Ctrl Pts',(0.208661738215443,19.6666248028076,-13.5501067434657));
#35561=CARTESIAN_POINT('Ctrl Pts',(0.0315693147396978,19.6569408091057,
-13.1460092493455));
#35562=CARTESIAN_POINT('Ctrl Pts',(36.4261761409748,20.4780024533914,-38.5952224603748));
#35563=CARTESIAN_POINT('Ctrl Pts',(35.986637929013,20.4514551579611,-38.6032854778725));
#35564=CARTESIAN_POINT('Ctrl Pts',(35.5454891020888,20.4251375618498,-38.6041190220481));
#35565=CARTESIAN_POINT('Ctrl Pts',(33.6566517848401,20.3138746691076,-38.5763723973499));
#35566=CARTESIAN_POINT('Ctrl Pts',(30.799764830004,20.1526659052326,-38.3782553300922));
#35567=CARTESIAN_POINT('Ctrl Pts',(26.6460909339275,19.938389785095,-37.6371881197587));
#35568=CARTESIAN_POINT('Ctrl Pts',(21.9831266869516,19.7189203495023,-36.2816526896943));
#35569=CARTESIAN_POINT('Ctrl Pts',(17.5857043101642,19.5342279169114,-34.3461449082959));
#35570=CARTESIAN_POINT('Ctrl Pts',(13.5090535945347,19.3763677050182,-31.8815190659229));
#35571=CARTESIAN_POINT('Ctrl Pts',(9.71842519564791,19.2344308170631,-29.0208914311038));
#35572=CARTESIAN_POINT('Ctrl Pts',(6.3220243987362,19.1049298841923,-25.6994767197043));
#35573=CARTESIAN_POINT('Ctrl Pts',(3.37464546431908,18.9752993129734,-21.9689400080561));
#35574=CARTESIAN_POINT('Ctrl Pts',(1.18113008703572,18.8580619466085,-18.5145574386863));
#35575=CARTESIAN_POINT('Ctrl Pts',(-0.0427945786360649,18.7718242877839,
-16.0563358690166));
#35576=CARTESIAN_POINT('Ctrl Pts',(-0.764115527911374,18.7111415689428,
-14.3933658531605));
#35577=CARTESIAN_POINT('Ctrl Pts',(-0.930311638349101,18.6963263828107,
-13.9920962059114));
#35578=CARTESIAN_POINT('Ctrl Pts',(-1.08962388875839,18.6812985797984,-13.5887572530535));
#35579=CARTESIAN_POINT('Ctrl Pts',(32.8663379166031,19.4355555088431,-40.352388449454));
#35580=CARTESIAN_POINT('Ctrl Pts',(32.4341853602501,19.4044605226273,-40.3432433773694));
#35581=CARTESIAN_POINT('Ctrl Pts',(32.0006794219008,19.3735658358572,-40.3268336283199));
#35582=CARTESIAN_POINT('Ctrl Pts',(30.1455752260411,19.2426748194849,-40.225361844379));
#35583=CARTESIAN_POINT('Ctrl Pts',(27.3470061899373,19.0517849995255,-39.9163785780022));
#35584=CARTESIAN_POINT('Ctrl Pts',(23.3001475854099,18.7933185397158,-39.0168456268584));
#35585=CARTESIAN_POINT('Ctrl Pts',(18.7835937846305,18.5218580841843,-37.4876069944926));
#35586=CARTESIAN_POINT('Ctrl Pts',(14.5588498457702,18.2836948825759,-35.3949061736525));
#35587=CARTESIAN_POINT('Ctrl Pts',(10.6796571258641,18.0697821020849,-32.7934064906319));
#35588=CARTESIAN_POINT('Ctrl Pts',(7.10550345028232,17.8693333343866,-29.8141833444967));
#35589=CARTESIAN_POINT('Ctrl Pts',(3.94833414086203,17.6778661310593,-26.3995431411007));
#35590=CARTESIAN_POINT('Ctrl Pts',(1.261414339538,17.4826662284719,-22.6048988734338));
#35591=CARTESIAN_POINT('Ctrl Pts',(-0.694991270314942,17.3068805329357,
-19.1172262254337));
#35592=CARTESIAN_POINT('Ctrl Pts',(-1.75206424347501,17.1802068447994,-16.6523685039809));
#35593=CARTESIAN_POINT('Ctrl Pts',(-2.36088439247878,17.0925519552341,-14.9905124109959));
#35594=CARTESIAN_POINT('Ctrl Pts',(-2.49997738438369,17.0712544126695,-14.5898820052411));
#35595=CARTESIAN_POINT('Ctrl Pts',(-2.63209034972266,17.0497370990139,-14.1875565005782));
#35596=CARTESIAN_POINT('Ctrl Pts',(28.8476080321524,17.8320672383652,-42.3340573620036));
#35597=CARTESIAN_POINT('Ctrl Pts',(28.4242559702612,17.7976045693245,-42.3048025675408));
#35598=CARTESIAN_POINT('Ctrl Pts',(27.9998760163417,17.7633163796081,-42.2682319449215));
#35599=CARTESIAN_POINT('Ctrl Pts',(26.1851332576131,17.6178640028275,-42.0805220574034));
#35600=CARTESIAN_POINT('Ctrl Pts',(23.4561592290513,17.4049846203341,-41.6418489334921));
#35601=CARTESIAN_POINT('Ctrl Pts',(19.5363333532145,17.1135517229592,-40.5568927329762));
#35602=CARTESIAN_POINT('Ctrl Pts',(15.1935312115776,16.8027253827761,-38.8243026322638));
#35603=CARTESIAN_POINT('Ctrl Pts',(11.1733728412317,16.523022337621,-36.5474036026815));
#35604=CARTESIAN_POINT('Ctrl Pts',(7.52791143671306,16.2641978724915,-33.7852548504584));
#35605=CARTESIAN_POINT('Ctrl Pts',(4.20988819682692,16.0157341831644,-30.6665573081524));
#35606=CARTESIAN_POINT('Ctrl Pts',(1.33569436348711,15.7719994721116,-27.1418227474879));
#35607=CARTESIAN_POINT('Ctrl Pts',(-1.04314652395158,15.5202180684676,-23.2707912034377));
#35608=CARTESIAN_POINT('Ctrl Pts',(-2.71906488312326,15.2931736272884,-19.7427113117026));
#35609=CARTESIAN_POINT('Ctrl Pts',(-3.5787250746749,15.130708702949,-17.2689175280809));
#35610=CARTESIAN_POINT('Ctrl Pts',(-4.0544204118661,15.0190926843839,-15.6075225274741));
#35611=CARTESIAN_POINT('Ctrl Pts',(-4.16141291752838,14.9920326361705,-15.2075025129441));
#35612=CARTESIAN_POINT('Ctrl Pts',(-4.26128529310459,14.9647422323135,-14.806289065777));
#35613=CARTESIAN_POINT('Ctrl Pts',(25.0217595366867,15.7638142683891,-44.2188893423579));
#35614=CARTESIAN_POINT('Ctrl Pts',(24.6072996956272,15.7283726072843,-44.1695456082369));
#35615=CARTESIAN_POINT('Ctrl Pts',(24.1921654581022,15.6930928161318,-44.1128268187239));
#35616=CARTESIAN_POINT('Ctrl Pts',(22.4184201291253,15.543379415412,-43.838904024895));
#35617=CARTESIAN_POINT('Ctrl Pts',(19.7600483717488,15.3241289383934,-43.2705677716271));
#35618=CARTESIAN_POINT('Ctrl Pts',(15.968898677068,15.0227233638938,-42.0001634916369));
#35619=CARTESIAN_POINT('Ctrl Pts',(11.8019542210027,14.6988957424381,-40.0640851202867));
#35620=CARTESIAN_POINT('Ctrl Pts',(7.98876258105558,14.4035050799014,-37.6026779566113));
#35621=CARTESIAN_POINT('Ctrl Pts',(4.57974174037815,14.1252237593235,-34.6793426631575));
#35622=CARTESIAN_POINT('Ctrl Pts',(1.52084636993269,13.8539516979883,-31.4204234207614));
#35623=CARTESIAN_POINT('Ctrl Pts',(-1.0669830575238,13.5829362127958,-27.7845505376458));
#35624=CARTESIAN_POINT('Ctrl Pts',(-3.13392029853443,13.2994842764397,-23.8357408245836));
#35625=CARTESIAN_POINT('Ctrl Pts',(-4.52575473794716,13.0425486753816,-20.2658011034729));
#35626=CARTESIAN_POINT('Ctrl Pts',(-5.18537945381502,12.8585920936854,-17.781914569308));
#35627=CARTESIAN_POINT('Ctrl Pts',(-5.52614664487988,12.7324540777387,-16.1201531218344));
#35628=CARTESIAN_POINT('Ctrl Pts',(-5.60058735037131,12.7018988467546,-15.7206244118355));
#35629=CARTESIAN_POINT('Ctrl Pts',(-5.66775192133469,12.6711030837425,-15.3204821076368));
#35630=CARTESIAN_POINT('Ctrl Pts',(21.4264044178079,13.2592937677246,-45.9895910901952));
#35631=CARTESIAN_POINT('Ctrl Pts',(21.0207170797347,13.2252177231213,-45.9202794452612));
#35632=CARTESIAN_POINT('Ctrl Pts',(20.6147340271746,13.191306123502,-45.8435284862164));
#35633=CARTESIAN_POINT('Ctrl Pts',(18.8816955041136,13.0474600457288,-45.4838725167592));
#35634=CARTESIAN_POINT('Ctrl Pts',(16.2935316715566,12.8372075593629,-44.7865804199157));
#35635=CARTESIAN_POINT('Ctrl Pts',(12.630646501664,12.5484949329477,-43.331681055911));
#35636=CARTESIAN_POINT('Ctrl Pts',(8.63931769810801,12.2377054846042,-41.1930723986167));
#35637=CARTESIAN_POINT('Ctrl Pts',(5.03318068432933,11.9522310106351,-38.5478898203658));
#35638=CARTESIAN_POINT('Ctrl Pts',(1.86105994601815,11.6797819251771,-35.4638295667092));
#35639=CARTESIAN_POINT('Ctrl Pts',(-0.937931348316951,11.4108111467242,
-32.0649104072594));
#35640=CARTESIAN_POINT('Ctrl Pts',(-3.23820124717178,11.1374939458242,-28.3177932082873));
#35641=CARTESIAN_POINT('Ctrl Pts',(-4.99158979822284,10.8473681096278,-24.2907317008292));
#35642=CARTESIAN_POINT('Ctrl Pts',(-6.09760889024641,10.5820480444149,-20.6782568121355));
#35643=CARTESIAN_POINT('Ctrl Pts',(-6.55582155513239,10.3910369789073,-18.1836367061482));
#35644=CARTESIAN_POINT('Ctrl Pts',(-6.76067954601502,10.2599216927486,-16.5210211970993));
#35645=CARTESIAN_POINT('Ctrl Pts',(-6.80233473263,10.2281653805015,-16.1219457386587));
#35646=CARTESIAN_POINT('Ctrl Pts',(-6.83656167557387,10.1961599190035,-15.7229135514833));
#35647=CARTESIAN_POINT('Ctrl Pts',(18.0357269294045,10.420684636249,-47.659627975918));
#35648=CARTESIAN_POINT('Ctrl Pts',(17.6385928198955,10.3898269637342,-47.5704962016297));
#35649=CARTESIAN_POINT('Ctrl Pts',(17.2415658583442,10.3591499865554,-47.4738593047325));
#35650=CARTESIAN_POINT('Ctrl Pts',(15.5485091238301,10.2291883131935,-47.0290943922104));
#35651=CARTESIAN_POINT('Ctrl Pts',(13.029492102221,10.0401067219452,-46.2037726571784));
#35652=CARTESIAN_POINT('Ctrl Pts',(9.493446906322,9.78206378055234,-44.5656595342354));
#35653=CARTESIAN_POINT('Ctrl Pts',(5.67628649226391,9.50499638561923,-42.2258694110056));
#35654=CARTESIAN_POINT('Ctrl Pts',(2.27604713466135,9.24981780003299,-39.3980542159176));
#35655=CARTESIAN_POINT('Ctrl Pts',(-0.660012836774006,9.00337535985762,
-36.1541737706072));
#35656=CARTESIAN_POINT('Ctrl Pts',(-3.19967324810691,8.75677479408939,-32.6159534467063));
#35657=CARTESIAN_POINT('Ctrl Pts',(-5.21261012281686,8.50116890088297,-28.7580142662565));
#35658=CARTESIAN_POINT('Ctrl Pts',(-6.65231229913932,8.22444592813344,-24.6528208257726));
#35659=CARTESIAN_POINT('Ctrl Pts',(-7.47214165787956,7.96804930448713,-20.9976952088575));
#35660=CARTESIAN_POINT('Ctrl Pts',(-7.72851793086956,7.78162503245108,-18.4921122305609));
#35661=CARTESIAN_POINT('Ctrl Pts',(-7.79712912596018,7.65323614745839,-16.8284397915245));
#35662=CARTESIAN_POINT('Ctrl Pts',(-7.80594114112445,7.62212996336316,-16.429842680561));
#35663=CARTESIAN_POINT('Ctrl Pts',(-7.80719772122039,7.59076668565169,-16.0320169120303));
#35664=CARTESIAN_POINT('Ctrl Pts',(14.9263225873298,7.18298363715391,-49.1920433928168));
#35665=CARTESIAN_POINT('Ctrl Pts',(14.5373462477221,7.15763661423686,-49.083341668369));
#35666=CARTESIAN_POINT('Ctrl Pts',(14.1488989149765,7.13250342173354,-48.9670696710061));
#35667=CARTESIAN_POINT('Ctrl Pts',(12.4943021862807,7.02634360727853,-48.4382762487368));
#35668=CARTESIAN_POINT('Ctrl Pts',(10.0421734244781,6.87350147707393,-47.4865326623943));
#35669=CARTESIAN_POINT('Ctrl Pts',(6.62981736222956,6.66841421880391,-45.6674560418548));
#35670=CARTESIAN_POINT('Ctrl Pts',(2.98344680610714,6.45075222930465,-43.1288991805643));
#35671=CARTESIAN_POINT('Ctrl Pts',(-0.21387899888273,6.25122984378583,-40.1205772506902));
#35672=CARTESIAN_POINT('Ctrl Pts',(-2.91644126996934,6.05595707526583,-36.7186795841497));
#35673=CARTESIAN_POINT('Ctrl Pts',(-5.1989863376844,5.8568061689083,-33.042686700556));
#35674=CARTESIAN_POINT('Ctrl Pts',(-6.92635942816575,5.64398234710963,-29.0750920509953));
#35675=CARTESIAN_POINT('Ctrl Pts',(-8.05368554515301,5.40587468584602,-24.8925459720573));
#35676=CARTESIAN_POINT('Ctrl Pts',(-8.58812995110823,5.18017895256177,-21.195162220079));
#35677=CARTESIAN_POINT('Ctrl Pts',(-8.6429926139357,5.01301666232781,-18.6786887740101));
#35678=CARTESIAN_POINT('Ctrl Pts',(-8.57549902139121,4.89707445701614,-17.0139432928344));
#35679=CARTESIAN_POINT('Ctrl Pts',(-8.55154256695504,4.86894780999335,-16.6158843105388));
#35680=CARTESIAN_POINT('Ctrl Pts',(-8.51994489356607,4.84055053954568,-16.219385523394));
#35681=CARTESIAN_POINT('Ctrl Pts',(12.1368282372958,3.57357815210241,-50.5688018516697));
#35682=CARTESIAN_POINT('Ctrl Pts',(11.7554123328022,3.55599962931061,-50.4408839449622));
#35683=CARTESIAN_POINT('Ctrl Pts',(11.3749590315426,3.53868515668548,-50.3053323379297));
#35684=CARTESIAN_POINT('Ctrl Pts',(9.75637557807125,3.46609807861293,-49.694041504612));
#35685=CARTESIAN_POINT('Ctrl Pts',(7.36747465897793,3.36435917107101,-48.6181602146532));
#35686=CARTESIAN_POINT('Ctrl Pts',(4.07359311144879,3.23426720235262,-46.6213471567875));
#35687=CARTESIAN_POINT('Ctrl Pts',(0.592266114139445,3.10147907156715,-43.8875382056778));
#35688=CARTESIAN_POINT('Ctrl Pts',(-2.40745520099751,2.98285053627008,-40.7018914156105));
#35689=CARTESIAN_POINT('Ctrl Pts',(-4.881376482725,2.86388130857434,-37.1448007849025));
#35690=CARTESIAN_POINT('Ctrl Pts',(-6.91129700276302,2.73730530568202,-33.3335628727181));
#35691=CARTESIAN_POINT('Ctrl Pts',(-8.35713647436029,2.59247375589619,-29.2584572853056));
#35692=CARTESIAN_POINT('Ctrl Pts',(-9.17565778305131,2.41842603756845,-25.0003067251804));
#35693=CARTESIAN_POINT('Ctrl Pts',(-9.42746720654185,2.24547053120763,-21.2618875642968));
#35694=CARTESIAN_POINT('Ctrl Pts',(-9.28244579831276,2.11246131963295,-18.7351534976944));
#35695=CARTESIAN_POINT('Ctrl Pts',(-9.07985419139475,2.01884144332686,-17.0696884188939));
#35696=CARTESIAN_POINT('Ctrl Pts',(-9.02342492784415,1.99605339732081,-16.6722973051515));
#35697=CARTESIAN_POINT('Ctrl Pts',(-8.95932258452836,1.9729679754383,-16.277297154442));
#35698=CARTESIAN_POINT('Ctrl Pts',(9.98308729044565,0.237308438758995,-51.6337369763077));
#35699=CARTESIAN_POINT('Ctrl Pts',(9.60764508493566,0.227921876287717,-51.4896368989849));
#35700=CARTESIAN_POINT('Ctrl Pts',(9.23354409583478,0.218854274805993,-51.337851066959));
#35701=CARTESIAN_POINT('Ctrl Pts',(7.64372668599397,0.181679983795775,-50.6571053064643));
#35702=CARTESIAN_POINT('Ctrl Pts',(5.30586692108267,0.133848323063104,-49.4766978346564));
#35703=CARTESIAN_POINT('Ctrl Pts',(2.10900967202317,0.0830496793456984,
-47.3302024745056));
#35704=CARTESIAN_POINT('Ctrl Pts',(-1.23588264070169,0.0403924264632703,
-44.4319527811565));
#35705=CARTESIAN_POINT('Ctrl Pts',(-4.07094224723787,0.00837005963384143,
-41.0969843078284));
#35706=CARTESIAN_POINT('Ctrl Pts',(-6.35327641927623,-0.0279539839125438,
-37.4092823789468));
#35707=CARTESIAN_POINT('Ctrl Pts',(-8.17079469610385,-0.0750512999789021,
-33.4843188337937));
#35708=CARTESIAN_POINT('Ctrl Pts',(-9.37913231578503,-0.14423024726241,
-29.3189890563375));
#35709=CARTESIAN_POINT('Ctrl Pts',(-9.93646401117645,-0.245792879606331,
-24.9976885304961));
#35710=CARTESIAN_POINT('Ctrl Pts',(-9.94880670058422,-0.358291148292244,
-21.2253259653454));
#35711=CARTESIAN_POINT('Ctrl Pts',(-9.6341833149091,-0.451704594358635,
-18.6904927531654));
#35712=CARTESIAN_POINT('Ctrl Pts',(-9.31688770623376,-0.519340602547392,
-17.0248284403669));
#35713=CARTESIAN_POINT('Ctrl Pts',(-9.23293653279146,-0.535923052101836,
-16.6281324481184));
#35714=CARTESIAN_POINT('Ctrl Pts',(-9.1413335698033,-0.552841667182328,
-16.2345595159175));
#35715=CARTESIAN_POINT('Ctrl Pts',(8.71742711504317,-2.14030259993981,-52.261248116584));
#35716=CARTESIAN_POINT('Ctrl Pts',(8.34557578703409,-2.14321532053782,-52.1065889728662));
#35717=CARTESIAN_POINT('Ctrl Pts',(7.97531637712704,-2.14576465810466,-51.9442091427789));
#35718=CARTESIAN_POINT('Ctrl Pts',(6.40299033232049,-2.15494826818845,-51.2181372647421));
#35719=CARTESIAN_POINT('Ctrl Pts',(4.09662385140589,-2.16016260296573,-49.9695063715731));
#35720=CARTESIAN_POINT('Ctrl Pts',(0.960796243239608,-2.1481556077715,-47.7253009393472));
#35721=CARTESIAN_POINT('Ctrl Pts',(-2.29722537800971,-2.11918777525101,
-44.7197113769873));
#35722=CARTESIAN_POINT('Ctrl Pts',(-5.02637319628328,-2.08197924289826,
-41.2873053734851));
#35723=CARTESIAN_POINT('Ctrl Pts',(-7.18462246766922,-2.05170003121316,
-37.5144569913459));
#35724=CARTESIAN_POINT('Ctrl Pts',(-8.86400315627726,-2.03426137368081,
-33.5154567077776));
#35725=CARTESIAN_POINT('Ctrl Pts',(-9.91725418147156,-2.04135770257883,
-29.2915725925193));
#35726=CARTESIAN_POINT('Ctrl Pts',(-10.303501409541,-2.08278583441843,-24.9295834958016));
#35727=CARTESIAN_POINT('Ctrl Pts',(-10.158671970043,-2.14471303148954,-21.1356778940573));
#35728=CARTESIAN_POINT('Ctrl Pts',(-9.73254376982651,-2.20477046252904,
-18.5960886707828));
#35729=CARTESIAN_POINT('Ctrl Pts',(-9.33978118010959,-2.25046208753918,
-16.9306893408303));
#35730=CARTESIAN_POINT('Ctrl Pts',(-9.23774716358698,-2.26180965939547,
-16.5345551280317));
#35731=CARTESIAN_POINT('Ctrl Pts',(-9.12809944685942,-2.27353152926925,
-16.1420338282393));
#35732=CARTESIAN_POINT('Ctrl Pts',(7.90542948215533,-3.83428286431684,-52.6645839345492));
#35733=CARTESIAN_POINT('Ctrl Pts',(7.53590165189136,-3.83237339034492,-52.5027148758859));
#35734=CARTESIAN_POINT('Ctrl Pts',(7.16813877523133,-3.83006698099443,-52.3331010949965));
#35735=CARTESIAN_POINT('Ctrl Pts',(5.60722374759459,-3.81839846831683,-51.5760790939397));
#35736=CARTESIAN_POINT('Ctrl Pts',(3.321604168471,-3.79185933798401,-50.2808595028402));
#35737=CARTESIAN_POINT('Ctrl Pts',(0.226485183062754,-3.73301479320489,
-47.9699259107911));
#35738=CARTESIAN_POINT('Ctrl Pts',(-2.97314542399398,-3.65055513724086,
-44.8910367634591));
#35739=CARTESIAN_POINT('Ctrl Pts',(-5.63065732580343,-3.56151400652134,
-41.3921119532622));
#35740=CARTESIAN_POINT('Ctrl Pts',(-7.70462720584958,-3.48120332570528,
-37.5611761746473));
#35741=CARTESIAN_POINT('Ctrl Pts',(-9.28995114080236,-3.41513875248544,
-33.5117165341006));
#35742=CARTESIAN_POINT('Ctrl Pts',(-10.2373525252032,-3.37526128513496,
-29.2480114872144));
#35743=CARTESIAN_POINT('Ctrl Pts',(-10.5066198560549,-3.37099617994084,
-24.8584895527468));
#35744=CARTESIAN_POINT('Ctrl Pts',(-10.25419810544,-3.39437469848804,-21.0501600279107));
#35745=CARTESIAN_POINT('Ctrl Pts',(-9.75166572177836,-3.42893690611626,
-18.5075691746829));
#35746=CARTESIAN_POINT('Ctrl Pts',(-9.30717122040251,-3.45783930783476,
-16.8425331931811));
#35747=CARTESIAN_POINT('Ctrl Pts',(-9.1927532889878,-3.46518513130081,-16.4468304726437));
#35748=CARTESIAN_POINT('Ctrl Pts',(-9.07075916440024,-3.47293757911652,
-16.0550786758666));
#35749=CARTESIAN_POINT('Ctrl Pts',(7.68836219406744,-4.30636894546118,-52.7724905334873));
#35750=CARTESIAN_POINT('Ctrl Pts',(7.31945172587889,-4.3031084050989,-52.6086479674884));
#35751=CARTESIAN_POINT('Ctrl Pts',(6.95235378291849,-4.29944065268701,-52.4370535891093));
#35752=CARTESIAN_POINT('Ctrl Pts',(5.39448449972533,-4.28192251284736,-51.6715555556563));
#35753=CARTESIAN_POINT('Ctrl Pts',(3.11444173302997,-4.24645759656194,-50.363570522352));
#35754=CARTESIAN_POINT('Ctrl Pts',(0.0303625865548424,-4.17439213330946,
-48.0343394120201));
#35755=CARTESIAN_POINT('Ctrl Pts',(-3.15334948925292,-4.07676875425951,
-44.9353406529986));
#35756=CARTESIAN_POINT('Ctrl Pts',(-5.79125328317668,-3.97294922980807,
-41.4181631696894));
#35757=CARTESIAN_POINT('Ctrl Pts',(-7.84210278345764,-3.87828739688684,
-37.5712950799821));
#35758=CARTESIAN_POINT('Ctrl Pts',(-9.40160361738414,-3.79820251809058,
-33.5080100112351));
#35759=CARTESIAN_POINT('Ctrl Pts',(-10.3199373397262,-3.74469501429227,
-29.2334176019375));
#35760=CARTESIAN_POINT('Ctrl Pts',(-10.5571010912029,-3.72710099262819,
-24.836399911188));
#35761=CARTESIAN_POINT('Ctrl Pts',(-10.2751885578156,-3.7392015362719,-21.024174995613));
#35762=CARTESIAN_POINT('Ctrl Pts',(-9.75173749052255,-3.76629674044718,
-18.4808048167157));
#35763=CARTESIAN_POINT('Ctrl Pts',(-9.29309014227641,-3.79028538091932,
-16.8158973741638));
#35764=CARTESIAN_POINT('Ctrl Pts',(-9.17528674009693,-3.79646095010219,
-16.4203194311401));
#35765=CARTESIAN_POINT('Ctrl Pts',(-9.04991979836604,-3.80305340259771,
-16.0287845536983));
#35766=CARTESIAN_POINT('Ctrl Pts',(7.478964497047,-4.78145508078572,-52.8766677431764));
#35767=CARTESIAN_POINT('Ctrl Pts',(7.11064672563727,-4.77682808742727,-52.7108751022984));
#35768=CARTESIAN_POINT('Ctrl Pts',(6.74418835556891,-4.7717826224726,-52.5373229559984));
#35769=CARTESIAN_POINT('Ctrl Pts',(5.18925364106368,-4.74834091216943,-51.7634436186052));
#35770=CARTESIAN_POINT('Ctrl Pts',(2.914623657922,-4.70381966688121,-50.4428290878201));
#35771=CARTESIAN_POINT('Ctrl Pts',(-0.158642874478715,-4.61828583278682,
-48.0954812155703));
#35772=CARTESIAN_POINT('Ctrl Pts',(-3.32668125548832,-4.50515190400754,
-44.9765610052481));
#35773=CARTESIAN_POINT('Ctrl Pts',(-5.9452007299524,-4.38613315046716,-41.4412978481233));
#35774=CARTESIAN_POINT('Ctrl Pts',(-7.97314324858038,-4.27662792828432,
-37.5786495133028));
#35775=CARTESIAN_POINT('Ctrl Pts',(-9.50703969681092,-4.18197237106197,
-33.5016851686292));
#35776=CARTESIAN_POINT('Ctrl Pts',(-10.3965461370179,-4.11421750462538,
-29.2163430123597));
#35777=CARTESIAN_POINT('Ctrl Pts',(-10.6018933961317,-4.08262421860679,
-24.8119552227925));
#35778=CARTESIAN_POINT('Ctrl Pts',(-10.2907910363082,-4.0828488851085,-20.9959306432894));
#35779=CARTESIAN_POINT('Ctrl Pts',(-9.74665866616106,-4.10207414795096,
-18.4518304865827));
#35780=CARTESIAN_POINT('Ctrl Pts',(-9.27403000727624,-4.12088738197538,
-16.7870776721948));
#35781=CARTESIAN_POINT('Ctrl Pts',(-9.15288357365941,-4.12583098108427,
-16.3916291076865));
#35782=CARTESIAN_POINT('Ctrl Pts',(-9.0241874000593,-4.13120272145022,-16.0003140988939));
#35783=CARTESIAN_POINT('Ctrl Pts',(29.890987486445,20.7105311502984,-36.1080966928895));
#35784=CARTESIAN_POINT('Ctrl Pts',(24.8085647057379,20.5483438544848,-35.0888701401329));
#35785=CARTESIAN_POINT('Ctrl Pts',(19.9373459642322,20.4520245495079,-33.0660880724366));
#35786=CARTESIAN_POINT('Ctrl Pts',(11.2454199314767,20.3052748660675,-27.4198879717431));
#35787=CARTESIAN_POINT('Ctrl Pts',(7.42198356668275,20.248474007324,-23.7979876220315));
#35788=CARTESIAN_POINT('Ctrl Pts',(4.42502927770989,20.1925493450898,-19.5734565969181));
#35789=CARTESIAN_POINT('Ctrl Pts',(-0.621425836154269,-3.27137100779394,
-46.8708764744697));
#35790=CARTESIAN_POINT('Ctrl Pts',(-1.19192002758132,-3.25992112656234,
-46.3438042435511));
#35791=CARTESIAN_POINT('Ctrl Pts',(-1.74006508034292,-3.24789096764871,
-45.7971167502074));
#35792=CARTESIAN_POINT('Ctrl Pts',(-2.26512505204463,-3.23555894384663,
-45.2323405814156));
#35793=CARTESIAN_POINT('Ctrl Pts',(-3.55101548575753,-3.2053573815679,-43.8491837768993));
#35794=CARTESIAN_POINT('Ctrl Pts',(-4.69844665488631,-3.1733453434745,-42.3575352047323));
#35795=CARTESIAN_POINT('Ctrl Pts',(-5.69672404631823,-3.14345008158505,
-40.7799123033163));
#35796=CARTESIAN_POINT('Ctrl Pts',(-6.36224234103277,-3.12351990598108,
-39.7281636490199));
#35797=CARTESIAN_POINT('Ctrl Pts',(-6.96147006117184,-3.10453051989494,
-38.6382041778315));
#35798=CARTESIAN_POINT('Ctrl Pts',(-7.49127781852105,-3.08752071373526,
-37.5167253952501));
#35799=CARTESIAN_POINT('Ctrl Pts',(-8.02108557559295,-3.07051090758448,
-36.3952466132557));
#35800=CARTESIAN_POINT('Ctrl Pts',(-8.48147336995429,-3.0554806813514,-35.2422485198971));
#35801=CARTESIAN_POINT('Ctrl Pts',(-8.86932876672715,-3.04339100491456,
-34.0644287179805));
#35802=CARTESIAN_POINT('Ctrl Pts',(-9.45111186116346,-3.02525649028182,
-32.2976990173011));
#35803=CARTESIAN_POINT('Ctrl Pts',(-9.86969706149374,-3.01373821257335,
-30.4751204725295));
#35804=CARTESIAN_POINT('Ctrl Pts',(-10.1146971067807,-3.01128625574909,
-28.6193144325686));
#35805=CARTESIAN_POINT('Ctrl Pts',(-10.2780304699219,-3.00965161787009,
-27.382110408833));
#35806=CARTESIAN_POINT('Ctrl Pts',(-10.3642148756369,-3.01204645592803,
-26.1301386094594));
#35807=CARTESIAN_POINT('Ctrl Pts',(-10.3702000810198,-3.01891855380822,
-24.8700965047755));
#35808=CARTESIAN_POINT('Ctrl Pts',(-10.376185285685,-3.02579065086441,-23.6100545511774));
#35809=CARTESIAN_POINT('Ctrl Pts',(-10.3019713092703,-3.03714000665748,
-22.3419422941696));
#35810=CARTESIAN_POINT('Ctrl Pts',(-10.1445181071464,-3.05321938564873,
-21.0724462245572));
#35811=CARTESIAN_POINT('Ctrl Pts',(-10.0796369494723,-3.05984515577954,
-20.5493296823207));
#35812=CARTESIAN_POINT('Ctrl Pts',(-10.0006218827985,-3.06727406915267,
-20.0259781834012));
#35813=CARTESIAN_POINT('Ctrl Pts',(-9.90726126923415,-3.07550335254719,
-19.5028585426849));
#35814=CARTESIAN_POINT('Ctrl Pts',(7.33894778785658,-4.68328060676847,-52.9495146826653));
#35815=CARTESIAN_POINT('Ctrl Pts',(6.96962866947374,-4.67927906663786,-52.7827309003488));
#35816=CARTESIAN_POINT('Ctrl Pts',(6.60219995041845,-4.67486342687383,-52.6081308809317));
#35817=CARTESIAN_POINT('Ctrl Pts',(5.04785466086252,-4.65418501649615,-51.831828678971));
#35818=CARTESIAN_POINT('Ctrl Pts',(2.77634573789732,-4.61395560865182,-50.5086100724079));
#35819=CARTESIAN_POINT('Ctrl Pts',(-0.292045807321255,-4.53496565777432,
-48.1574762822767));
#35820=CARTESIAN_POINT('Ctrl Pts',(-3.45417942420346,-4.42959393838223,
-45.034302216954));
#35821=CARTESIAN_POINT('Ctrl Pts',(-6.06653279283,-4.31850354734918,-41.495020322408));
#35822=CARTESIAN_POINT('Ctrl Pts',(-8.08805877753573,-4.2170896233612,-37.6286344119132));
#35823=CARTESIAN_POINT('Ctrl Pts',(-9.61533213266668,-4.13063759391767,
-33.5481785074831));
#35824=CARTESIAN_POINT('Ctrl Pts',(-10.4979663275097,-4.07121155600733,
-29.2596885385511));
#35825=CARTESIAN_POINT('Ctrl Pts',(-10.6962016209548,-4.04803120464602,
-24.8525448652187));
#35826=CARTESIAN_POINT('Ctrl Pts',(-10.3788445940736,-4.055480889925,-21.0344500928801));
#35827=CARTESIAN_POINT('Ctrl Pts',(-9.83045198196616,-4.07952578289679,
-18.4891787747176));
#35828=CARTESIAN_POINT('Ctrl Pts',(-9.35438474400941,-4.10152925776619,
-16.8215905800271));
#35829=CARTESIAN_POINT('Ctrl Pts',(-9.23187396168105,-4.1072571624472,-16.4239003651629));
#35830=CARTESIAN_POINT('Ctrl Pts',(-9.10174148617946,-4.11341014061892,
-16.030408965445));
#35831=CARTESIAN_POINT('Ctrl Pts',(7.59886962875189,-4.24009445412503,-52.8204795434402));
#35832=CARTESIAN_POINT('Ctrl Pts',(7.22880440070895,-4.23725223817857,-52.6558021234907));
#35833=CARTESIAN_POINT('Ctrl Pts',(6.86057612481852,-4.23400446880359,-52.4833150943556));
#35834=CARTESIAN_POINT('Ctrl Pts',(5.30259606036827,-4.21832863439708,-51.7160246632286));
#35835=CARTESIAN_POINT('Ctrl Pts',(3.02458111694869,-4.18572164472913,-50.4063763572215));
#35836=CARTESIAN_POINT('Ctrl Pts',(-0.0563369732475343,-4.11799618192084,
-48.0747261660015));
#35837=CARTESIAN_POINT('Ctrl Pts',(-3.2362291943784,-4.02550335874969,-44.9730096590617));
#35838=CARTESIAN_POINT('Ctrl Pts',(-5.87015686281,-3.92690475481451,-41.4532657427213));
#35839=CARTESIAN_POINT('Ctrl Pts',(-7.91688453516029,-3.83755718932749,
-37.6040122637326));
#35840=CARTESIAN_POINT('Ctrl Pts',(-9.4721479569566,-3.76285616468038,-33.5385007226496));
#35841=CARTESIAN_POINT('Ctrl Pts',(-10.3861063459171,-3.71481495977278,
-29.2619011417045));
#35842=CARTESIAN_POINT('Ctrl Pts',(-10.6187640483301,-3.70275434803773,
-24.863123274024));
#35843=CARTESIAN_POINT('Ctrl Pts',(-10.3329026491843,-3.71962751323487,
-21.0495715365539));
#35844=CARTESIAN_POINT('Ctrl Pts',(-9.80676713372355,-3.74992063397164,
-18.5054458515168));
#35845=CARTESIAN_POINT('Ctrl Pts',(-9.3457471942309,-3.77604797989279,-16.8379483906474));
#35846=CARTESIAN_POINT('Ctrl Pts',(-9.22684691101437,-3.78276245762616,
-16.4401792867344));
#35847=CARTESIAN_POINT('Ctrl Pts',(-9.10030801587574,-3.78989370687861,
-16.0465102000721));
#35848=CARTESIAN_POINT('Ctrl Pts',(7.86406357984036,-3.80075287541765,-52.6888944549166));
#35849=CARTESIAN_POINT('Ctrl Pts',(7.49323426140441,-3.79905339336963,-52.5263353523576));
#35850=CARTESIAN_POINT('Ctrl Pts',(7.12418814332937,-3.79695621683146,-52.3559727587527));
#35851=CARTESIAN_POINT('Ctrl Pts',(5.56249423822884,-3.78620663871065,-51.5977405820072));
#35852=CARTESIAN_POINT('Ctrl Pts',(3.27786174290937,-3.76109400159902,-50.3017259640724));
#35853=CARTESIAN_POINT('Ctrl Pts',(0.184278354359802,-3.70440674399875,
-47.9896355736996));
#35854=CARTESIAN_POINT('Ctrl Pts',(-3.01350108687011,-3.62448835210827,
-44.9094470052877));
#35855=CARTESIAN_POINT('Ctrl Pts',(-5.66909257188744,-3.53802316526296,
-41.4092957476385));
#35856=CARTESIAN_POINT('Ctrl Pts',(-7.74107979291541,-3.46032715355504,
-37.5772209009879));
#35857=CARTESIAN_POINT('Ctrl Pts',(-9.32437443940699,-3.39690914788247,
-33.5266991900448));
#35858=CARTESIAN_POINT('Ctrl Pts',(-10.2696918840725,-3.35971861494906,
-29.2620368626687));
#35859=CARTESIAN_POINT('Ctrl Pts',(-10.5368248659369,-3.35817927654809,
-24.8716740420261));
#35860=CARTESIAN_POINT('Ctrl Pts',(-10.2825404940654,-3.38391914529348,
-21.0627083330555));
#35861=CARTESIAN_POINT('Ctrl Pts',(-9.77874494355101,-3.42007079724739,
-18.5197526990839));
#35862=CARTESIAN_POINT('Ctrl Pts',(-9.33284089999827,-3.45006162272336,
-16.8523595458168));
#35863=CARTESIAN_POINT('Ctrl Pts',(-9.2175692452616,-3.45770043113048,-16.4545137405203));
#35864=CARTESIAN_POINT('Ctrl Pts',(-9.09464351807648,-3.46574819271174,
-16.0606680874987));
#35865=CARTESIAN_POINT('Ctrl Pts',(8.8177622376813,-2.2653457359543,-52.2159314161534));
#35866=CARTESIAN_POINT('Ctrl Pts',(8.44417111226431,-2.26761569662348,-52.0608800900341));
#35867=CARTESIAN_POINT('Ctrl Pts',(8.072174006773,-2.26951335386862,-51.8980459063678));
#35868=CARTESIAN_POINT('Ctrl Pts',(6.49710028208358,-2.27586002752392,-51.1719095459996));
#35869=CARTESIAN_POINT('Ctrl Pts',(4.18873282943485,-2.27671432942662,-49.924179739321));
#35870=CARTESIAN_POINT('Ctrl Pts',(1.04999287472117,-2.25814179129592,-47.6813106456907));
#35871=CARTESIAN_POINT('Ctrl Pts',(-2.21131802312341,-2.2214798205824,-44.6772615529364));
#35872=CARTESIAN_POINT('Ctrl Pts',(-4.94361513155905,-2.17652897108851,
-41.2463728727339));
#35873=CARTESIAN_POINT('Ctrl Pts',(-7.10487029831094,-2.13845241575724,
-37.4750215186926));
#35874=CARTESIAN_POINT('Ctrl Pts',(-8.78714219447284,-2.11316923258448,
-33.4775050972905));
#35875=CARTESIAN_POINT('Ctrl Pts',(-9.84314207841108,-2.11235831802136,
-29.2550930390527));
#35876=CARTESIAN_POINT('Ctrl Pts',(-10.2320008554077,-2.14581153060268,
-24.8945741017885));
#35877=CARTESIAN_POINT('Ctrl Pts',(-10.0893195591215,-2.20085463389179,
-21.1019331266132));
#35878=CARTESIAN_POINT('Ctrl Pts',(-9.66456637968633,-2.25628908058851,
-18.5631943298776));
#35879=CARTESIAN_POINT('Ctrl Pts',(-9.27218786611045,-2.29898278275007,
-16.896221484846));
#35880=CARTESIAN_POINT('Ctrl Pts',(-9.16977542161468,-2.30966173471912,
-16.4981148423604));
#35881=CARTESIAN_POINT('Ctrl Pts',(-9.05966377546826,-2.32072459453129,
-16.1036530445452));
#35882=CARTESIAN_POINT('Ctrl Pts',(10.6092118097825,0.42091842584111,-51.328617643362));
#35883=CARTESIAN_POINT('Ctrl Pts',(10.23048025638,0.412015546281074,-51.1871145970464));
#35884=CARTESIAN_POINT('Ctrl Pts',(9.8530086134927,0.403442573942463,-51.0378687887964));
#35885=CARTESIAN_POINT('Ctrl Pts',(8.25318533936325,0.368526239150617,-50.3696782505686));
#35886=CARTESIAN_POINT('Ctrl Pts',(5.90113204983879,0.324281374370589,-49.2091135002706));
#35887=CARTESIAN_POINT('Ctrl Pts',(2.67983263917123,0.279215865745994,-47.0911873404082));
#35888=CARTESIAN_POINT('Ctrl Pts',(-0.697133045717137,0.243759038204317,
-44.2245576034823));
#35889=CARTESIAN_POINT('Ctrl Pts',(-3.56856160174788,0.21967725703067,-40.9186756979785));
#35890=CARTESIAN_POINT('Ctrl Pts',(-5.89133125107194,0.192114722189047,
-37.2569397966404));
#35891=CARTESIAN_POINT('Ctrl Pts',(-7.75241625781529,0.154437491851918,
-33.3551369283939));
#35892=CARTESIAN_POINT('Ctrl Pts',(-9.00808293107892,0.0954817696064694,
-29.2090777884208));
#35893=CARTESIAN_POINT('Ctrl Pts',(-9.61628317437987,0.0048363712043943,
-24.9025945312891));
#35894=CARTESIAN_POINT('Ctrl Pts',(-9.67455583695819,-0.0979118428630517,
-21.1396270961213));
#35895=CARTESIAN_POINT('Ctrl Pts',(-9.39204048671938,-0.184631554593919,
-18.6086884842893));
#35896=CARTESIAN_POINT('Ctrl Pts',(-9.0959566327371,-0.247909792323189,
-16.9426180555065));
#35897=CARTESIAN_POINT('Ctrl Pts',(-9.01670666115945,-0.263520166061751,
-16.5440824447891));
#35898=CARTESIAN_POINT('Ctrl Pts',(-8.9297037981404,-0.279478515480188,
-16.1485563076619));
#35899=CARTESIAN_POINT('Ctrl Pts',(13.3916902429157,3.93922736422659,-49.9537287467088));
#35900=CARTESIAN_POINT('Ctrl Pts',(13.0052118686551,3.92273017306588,-49.8315070830361));
#35901=CARTESIAN_POINT('Ctrl Pts',(12.6195329570733,3.90651491483579,-49.7016027937567));
#35902=CARTESIAN_POINT('Ctrl Pts',(10.9827808399633,3.83888692720806,-49.115910516525));
#35903=CARTESIAN_POINT('Ctrl Pts',(8.56616880546154,3.74496038387833,-48.0794149501526));
#35904=CARTESIAN_POINT('Ctrl Pts',(5.22446217876673,3.6271896762232,-46.1392640327796));
#35905=CARTESIAN_POINT('Ctrl Pts',(1.68027620871272,3.50969140214063,-43.4681077992377));
#35906=CARTESIAN_POINT('Ctrl Pts',(-1.39083143471865,3.40771510315772,-40.3400067193343));
#35907=CARTESIAN_POINT('Ctrl Pts',(-3.94420957473155,3.30695483103527,-36.8341782812466));
#35908=CARTESIAN_POINT('Ctrl Pts',(-6.05979964528246,3.1998573133211,-33.0685560561463));
#35909=CARTESIAN_POINT('Ctrl Pts',(-7.59877096111654,3.07607789704229,-29.0312385925458));
#35910=CARTESIAN_POINT('Ctrl Pts',(-8.51743941326012,2.92448144596071,-24.801916525237));
#35911=CARTESIAN_POINT('Ctrl Pts',(-8.85970116110627,2.77158317941627,-21.0815574802459));
#35912=CARTESIAN_POINT('Ctrl Pts',(-8.77792663629936,2.65236568914073,-18.562097581594));
#35913=CARTESIAN_POINT('Ctrl Pts',(-8.61766417553023,2.56779645721963,-16.8976093356764));
#35914=CARTESIAN_POINT('Ctrl Pts',(-8.57114352238457,2.54707902977605,-16.4985644453621));
#35915=CARTESIAN_POINT('Ctrl Pts',(-8.51685227096455,2.52604544176493,-16.1016514020163));
#35916=CARTESIAN_POINT('Ctrl Pts',(16.8590239124754,7.64857049485316,-48.2430713861362));
#35917=CARTESIAN_POINT('Ctrl Pts',(16.4632196116715,7.62538079009264,-48.1431494592939));
#35918=CARTESIAN_POINT('Ctrl Pts',(16.0677119033701,7.6024320797305,-48.0356205741132));
#35919=CARTESIAN_POINT('Ctrl Pts',(14.3869451174134,7.50598047950645,-47.5454025434781));
#35920=CARTESIAN_POINT('Ctrl Pts',(11.8938724168184,7.36825978906471,-46.6524594301012));
#35921=CARTESIAN_POINT('Ctrl Pts',(8.41082254202169,7.18657585481396,-44.9179175569957));
#35922=CARTESIAN_POINT('Ctrl Pts',(4.67151228739915,6.99739878870591,-42.4727538029817));
#35923=CARTESIAN_POINT('Ctrl Pts',(1.3686225793903,6.82819742189185,-39.5500970265053));
#35924=CARTESIAN_POINT('Ctrl Pts',(-1.45143853585427,6.66543158101024,-36.2243659095515));
#35925=CARTESIAN_POINT('Ctrl Pts',(-3.86066265880184,6.50060855796851,-32.6160075343978));
#35926=CARTESIAN_POINT('Ctrl Pts',(-5.72573184926258,6.32441606849526,-28.7042233083674));
#35927=CARTESIAN_POINT('Ctrl Pts',(-7.00109565032812,6.12505774886043,-24.5639570327674));
#35928=CARTESIAN_POINT('Ctrl Pts',(-7.66922039578791,5.93384517916791,-20.8927712940131));
#35929=CARTESIAN_POINT('Ctrl Pts',(-7.81753482922903,5.79035915091665,-18.3865669077403));
#35930=CARTESIAN_POINT('Ctrl Pts',(-7.81287491810413,5.69001969995687,-16.7239169361633));
#35931=CARTESIAN_POINT('Ctrl Pts',(-7.80393120495686,5.66551509710643,-16.3243468486962));
#35932=CARTESIAN_POINT('Ctrl Pts',(-7.78727676373068,5.64071489355821,-15.9259510977805));
#35933=CARTESIAN_POINT('Ctrl Pts',(20.1260836878443,10.6050661536892,-46.632830625662));
#35934=CARTESIAN_POINT('Ctrl Pts',(19.7218052839872,10.5777689837161,-46.5526052118606));
#35935=CARTESIAN_POINT('Ctrl Pts',(19.3174080381398,10.5506896266998,-46.4648422656697));
#35936=CARTESIAN_POINT('Ctrl Pts',(17.5970044237572,10.4365567481294,-46.058983429135));
#35937=CARTESIAN_POINT('Ctrl Pts',(15.0353807990198,10.2719415070743,-45.2928545013636));
#35938=CARTESIAN_POINT('Ctrl Pts',(11.4264127966159,10.0511774947007,-43.7398720626974));
#35939=CARTESIAN_POINT('Ctrl Pts',(7.51403185573689,9.81863871620139,-41.4941801425206));
#35940=CARTESIAN_POINT('Ctrl Pts',(4.00635829739916,9.60967367489776,-38.7527503735285));
#35941=CARTESIAN_POINT('Ctrl Pts',(0.951351346209991,9.41153176383594,-35.5857793543118));
#35942=CARTESIAN_POINT('Ctrl Pts',(-1.7160947488882,9.21500541081661,-32.1159600367897));
#35943=CARTESIAN_POINT('Ctrl Pts',(-3.86740386355494,9.01175979868378,-28.314634950641));
#35944=CARTESIAN_POINT('Ctrl Pts',(-5.45538785555814,8.78956564702969,-24.2525762590724));
#35945=CARTESIAN_POINT('Ctrl Pts',(-6.40881146344196,8.58124477590158,-20.6244241991297));
#35946=CARTESIAN_POINT('Ctrl Pts',(-6.75838644584931,8.42762540105217,-18.1296613415041));
#35947=CARTESIAN_POINT('Ctrl Pts',(-6.88977562100234,8.32086564673385,-16.4684620494197));
#35948=CARTESIAN_POINT('Ctrl Pts',(-6.91374446804093,8.29482075310626,-16.0684584954673));
#35949=CARTESIAN_POINT('Ctrl Pts',(-6.9301128982961,8.26849188852043,-15.6688519964121));
#35950=CARTESIAN_POINT('Ctrl Pts',(24.0944858944396,13.6252616883324,-44.6776818510423));
#35951=CARTESIAN_POINT('Ctrl Pts',(23.6803406585357,13.5952855444977,-44.6200952707445));
#35952=CARTESIAN_POINT('Ctrl Pts',(23.2656345591204,13.5655149131873,-44.555050002304));
#35953=CARTESIAN_POINT('Ctrl Pts',(21.4994400484191,13.4398628522405,-44.2461531702864));
#35954=CARTESIAN_POINT('Ctrl Pts',(18.8587889372672,13.2576618204372,-43.6257566226496));
#35955=CARTESIAN_POINT('Ctrl Pts',(15.1051146705744,13.0115743729063,-42.2813283108309));
#35956=CARTESIAN_POINT('Ctrl Pts',(10.9942878557702,12.751644575675,-40.2646477779735));
#35957=CARTESIAN_POINT('Ctrl Pts',(7.25229871579309,12.5189796899122,-37.7311156744984));
#35958=CARTESIAN_POINT('Ctrl Pts',(3.92890521817145,12.301865256328,-34.7460690231871));
#35959=CARTESIAN_POINT('Ctrl Pts',(0.96680269920358,12.0904144587841,-31.4348095438096));
#35960=CARTESIAN_POINT('Ctrl Pts',(-1.51075548194581,11.8774764455751,-27.7596131452014));
#35961=CARTESIAN_POINT('Ctrl Pts',(-3.45469180565196,11.6504923923572,-23.7864536540749));
#35962=CARTESIAN_POINT('Ctrl Pts',(-4.73272035107421,11.4410171343385,-20.2068032096485));
#35963=CARTESIAN_POINT('Ctrl Pts',(-5.31112734453827,11.2882220371981,-17.7244763646882));
#35964=CARTESIAN_POINT('Ctrl Pts',(-5.59715265714841,11.1823584691134,-16.0644493054574));
#35965=CARTESIAN_POINT('Ctrl Pts',(-5.65857325334263,11.1565388193505,-15.6639265472815));
#35966=CARTESIAN_POINT('Ctrl Pts',(-5.71256297075867,11.1304479812224,-15.2630020264613));
#35967=CARTESIAN_POINT('Ctrl Pts',(27.7524631280282,15.9398275064074,-42.8755062279286));
#35968=CARTESIAN_POINT('Ctrl Pts',(27.3296292380419,15.9092719019138,-42.8377973240549));
#35969=CARTESIAN_POINT('Ctrl Pts',(26.9058773118923,15.8789225535602,-42.7926942326871));
#35970=CARTESIAN_POINT('Ctrl Pts',(25.0996377363701,15.7507918597713,-42.5689002608853));
#35971=CARTESIAN_POINT('Ctrl Pts',(22.3899228472107,15.5646999212503,-42.076390030712));
#35972=CARTESIAN_POINT('Ctrl Pts',(18.5099328809061,15.3133344724918,-40.9148965646952));
#35973=CARTESIAN_POINT('Ctrl Pts',(14.2260415512262,15.0487502016962,-39.0989822697625));
#35974=CARTESIAN_POINT('Ctrl Pts',(10.2799024562032,14.8142492774957,-36.7475381195557));
#35975=CARTESIAN_POINT('Ctrl Pts',(6.72287574105206,14.5991383033468,-33.9216147039428));
#35976=CARTESIAN_POINT('Ctrl Pts',(3.50443021549915,14.3930646018661,-30.7488263968559));
#35977=CARTESIAN_POINT('Ctrl Pts',(0.743246967286701,14.1899609567462,-27.1834418577565));
#35978=CARTESIAN_POINT('Ctrl Pts',(-1.50992084988385,13.977122935371,-23.2872040240248));
#35979=CARTESIAN_POINT('Ctrl Pts',(-3.06979700167895,13.7824369346935,-19.7490208233323));
#35980=CARTESIAN_POINT('Ctrl Pts',(-3.84678924988332,13.6409944051188,-17.2767648669773));
#35981=CARTESIAN_POINT('Ctrl Pts',(-4.26697517747692,13.5429643472183,-15.6171729631503));
#35982=CARTESIAN_POINT('Ctrl Pts',(-4.36090283399386,13.5190447294408,-15.2161420151018));
#35983=CARTESIAN_POINT('Ctrl Pts',(-4.44756309121091,13.4948677704672,-14.8140961072926));
#35984=CARTESIAN_POINT('Ctrl Pts',(32.1092038605354,18.188947172369,-40.7280566168821));
#35985=CARTESIAN_POINT('Ctrl Pts',(31.6765553815004,18.1597316481657,-40.7130636737339));
#35986=CARTESIAN_POINT('Ctrl Pts',(31.2426152350551,18.1307342364494,-40.6907406131988));
#35987=CARTESIAN_POINT('Ctrl Pts',(29.3914008267549,18.0083786966032,-40.5641260176311));
#35988=CARTESIAN_POINT('Ctrl Pts',(26.6040098369721,17.830846834045,-40.2176280285863));
#35989=CARTESIAN_POINT('Ctrl Pts',(22.5816971333687,17.5925027676131,-39.2649049617731));
#35990=CARTESIAN_POINT('Ctrl Pts',(18.1026055111639,17.3443426911773,-37.6779673237996));
#35991=CARTESIAN_POINT('Ctrl Pts',(13.9260329063887,17.1289494695207,-35.5339680565631));
#35992=CARTESIAN_POINT('Ctrl Pts',(10.1052117066657,16.9369213116231,-32.8890131586941));
#35993=CARTESIAN_POINT('Ctrl Pts',(6.59730531312819,16.7575317657622,-29.8733821949946));
#35994=CARTESIAN_POINT('Ctrl Pts',(3.5158662876463,16.5859876106103,-26.4321103440903));
#35995=CARTESIAN_POINT('Ctrl Pts',(0.913599505363284,16.4095763329362,-22.6220597413816));
#35996=CARTESIAN_POINT('Ctrl Pts',(-0.964389552830138,16.2491906636996,
-19.1295387897028));
#35997=CARTESIAN_POINT('Ctrl Pts',(-1.9654556525298,16.1323920433636,-16.6674580294462));
#35998=CARTESIAN_POINT('Ctrl Pts',(-2.53699602967554,16.0510402241362,-15.007420086541));
#35999=CARTESIAN_POINT('Ctrl Pts',(-2.66758615191287,16.0311583490605,-14.60568241689));
#36000=CARTESIAN_POINT('Ctrl Pts',(-2.79108562724462,16.01103806515,-14.2023282308814));
#36001=CARTESIAN_POINT('Ctrl Pts',(36.0546359053991,19.7983627848149,-38.7818450804867));
#36002=CARTESIAN_POINT('Ctrl Pts',(35.6136081827865,19.7720645135703,-38.7866824550858));
#36003=CARTESIAN_POINT('Ctrl Pts',(35.1709903510993,19.7460021313493,-38.7842339544363));
#36004=CARTESIAN_POINT('Ctrl Pts',(33.2815581289281,19.6361820466171,-38.742359341364));
#36005=CARTESIAN_POINT('Ctrl Pts',(30.4279662779038,19.4774394485581,-38.5231664068375));
#36006=CARTESIAN_POINT('Ctrl Pts',(26.2838812573179,19.2670183310104,-37.7523847452164));
#36007=CARTESIAN_POINT('Ctrl Pts',(21.6373652569733,19.0520629838802,-36.3648646999831));
#36008=CARTESIAN_POINT('Ctrl Pts',(17.2627637487776,18.8717166252608,-34.4013101103432));
#36009=CARTESIAN_POINT('Ctrl Pts',(13.2149882844746,18.7178122962125,-31.9134568102013));
#36010=CARTESIAN_POINT('Ctrl Pts',(9.45790253167546,18.5794411422907,-29.0339285444168));
#36011=CARTESIAN_POINT('Ctrl Pts',(6.10065537573886,18.4529446490623,-25.6996110869408));
#36012=CARTESIAN_POINT('Ctrl Pts',(3.19769760622167,18.3257380682571,-21.9630515161149));
#36013=CARTESIAN_POINT('Ctrl Pts',(1.04570997608589,18.2102139945187,-18.5086252116051));
#36014=CARTESIAN_POINT('Ctrl Pts',(-0.148334551971419,18.1249152482566,
-16.0540528873188));
#36015=CARTESIAN_POINT('Ctrl Pts',(-0.850211959005697,18.064727637235,-14.392650263373));
#36016=CARTESIAN_POINT('Ctrl Pts',(-1.01234491068815,18.0499634327475,-13.9901402067394));
#36017=CARTESIAN_POINT('Ctrl Pts',(-1.16751365266792,18.0349776243875,-13.5855669779328));
#36018=CARTESIAN_POINT('Ctrl Pts',(38.9437130531413,20.6836496418694,-37.3550102934179));
#36019=CARTESIAN_POINT('Ctrl Pts',(38.4969620505322,20.6606519170286,-37.3739256635358));
#36020=CARTESIAN_POINT('Ctrl Pts',(38.0484242481362,20.6379063239872,-37.3855784628576));
#36021=CARTESIAN_POINT('Ctrl Pts',(36.1329514022312,20.5422448076096,-37.4037961231016));
#36022=CARTESIAN_POINT('Ctrl Pts',(33.2340079962508,20.4047755971079,-37.2748703197067));
#36023=CARTESIAN_POINT('Ctrl Pts',(29.0058954113699,20.225761668211,-36.6330394337848));
#36024=CARTESIAN_POINT('Ctrl Pts',(24.243314845652,20.0475517349526,-35.3867546793722));
#36025=CARTESIAN_POINT('Ctrl Pts',(19.7309119375686,19.9048724048602,-33.550821780949));
#36026=CARTESIAN_POINT('Ctrl Pts',(15.5248315097876,19.790507905872,-31.1738206489958));
#36027=CARTESIAN_POINT('Ctrl Pts',(11.593709050744,19.6935273080542,-28.3900502035695));
#36028=CARTESIAN_POINT('Ctrl Pts',(8.04360552628351,19.6110850660289,-25.130528158443));
#36029=CARTESIAN_POINT('Ctrl Pts',(4.93025190736926,19.530779076001,-21.4446834603861));
#36030=CARTESIAN_POINT('Ctrl Pts',(2.58648434761514,19.4573327991495,-18.0158038661496));
#36031=CARTESIAN_POINT('Ctrl Pts',(1.25734840204799,19.4012238336331,-15.5653813052934));
#36032=CARTESIAN_POINT('Ctrl Pts',(0.46423054638623,19.3605693891818,-13.9021664678085));
#36033=CARTESIAN_POINT('Ctrl Pts',(0.280042164317415,19.3505226070412,-13.4989464907574));
#36034=CARTESIAN_POINT('Ctrl Pts',(0.10275343541301,19.3402634731691,-13.0933876689219));
#36035=CARTESIAN_POINT('Ctrl Pts',(40.5688973540866,21.117312799858,-36.551901496451));
#36036=CARTESIAN_POINT('Ctrl Pts',(40.1190235321024,21.0964267127388,-36.5786509976099));
#36037=CARTESIAN_POINT('Ctrl Pts',(39.66725798273,21.0758020890032,-36.5981477349547));
#36038=CARTESIAN_POINT('Ctrl Pts',(37.737597636275,20.9891913310095,-36.6497793174299));
#36039=CARTESIAN_POINT('Ctrl Pts',(34.8138724138779,20.8653273744228,-36.5710441821179));
#36040=CARTESIAN_POINT('Ctrl Pts',(30.5396616708079,20.7063681300896,-36.0009003281876));
#36041=CARTESIAN_POINT('Ctrl Pts',(25.7132460636541,20.5515335415639,-34.8331079770803));
#36042=CARTESIAN_POINT('Ctrl Pts',(21.1248952553841,20.4326519806542,-33.0680590907502));
#36043=CARTESIAN_POINT('Ctrl Pts',(16.8314507574351,20.3430531321453,-30.7525636742139));
#36044=CARTESIAN_POINT('Ctrl Pts',(12.804210193334,20.2718184169426,-28.0218547905441));
#36045=CARTESIAN_POINT('Ctrl Pts',(9.14752307967792,20.2165549432469,-24.8036643499281));
#36046=CARTESIAN_POINT('Ctrl Pts',(5.91784322010844,20.164982094833,-21.145672025709));
#36047=CARTESIAN_POINT('Ctrl Pts',(3.46801805054593,20.117197691553,-17.7306313359114));
#36048=CARTESIAN_POINT('Ctrl Pts',(2.0641638961292,20.0788282397779,-15.2822216218412));
#36049=CARTESIAN_POINT('Ctrl Pts',(1.22057987406261,20.0500302875854,-13.6177868335942));
#36050=CARTESIAN_POINT('Ctrl Pts',(1.02420216661473,20.0428451797642,-13.2141323698032));
#36051=CARTESIAN_POINT('Ctrl Pts',(0.834697633919559,20.0354515632684,-12.8079971705157));
#36052=CARTESIAN_POINT('Ctrl Pts',(41.0310809778576,21.2334813897109,-36.3234534242004));
#36053=CARTESIAN_POINT('Ctrl Pts',(40.5803248224942,21.2132228077857,-36.3524241259849));
#36054=CARTESIAN_POINT('Ctrl Pts',(40.1276475607981,21.1932283095702,-36.3741443398451));
#36055=CARTESIAN_POINT('Ctrl Pts',(38.1939810821135,21.1093059289188,-36.4352454955676));
#36056=CARTESIAN_POINT('Ctrl Pts',(35.2632566089281,20.9894835119608,-36.3707324792311));
#36057=CARTESIAN_POINT('Ctrl Pts',(30.9760261741618,20.8364792943525,-35.8208951740754));
#36058=CARTESIAN_POINT('Ctrl Pts',(26.1315861185953,20.6885792302246,-34.6753271627914));
#36059=CARTESIAN_POINT('Ctrl Pts',(21.5218030653981,20.5767478260626,-32.9303346052545));
#36060=CARTESIAN_POINT('Ctrl Pts',(17.2037226950434,20.4944756050622,-30.6322254140711));
#36061=CARTESIAN_POINT('Ctrl Pts',(13.1493988567874,20.4308554028779,-27.9164985852922));
#36062=CARTESIAN_POINT('Ctrl Pts',(9.46270544626104,20.3836340081555,-24.7099515839323));
#36063=CARTESIAN_POINT('Ctrl Pts',(6.20030107714963,20.340580727313,-21.0597648792395));
#36064=CARTESIAN_POINT('Ctrl Pts',(3.72065547802652,20.3004356869138,-17.6485527564509));
#36065=CARTESIAN_POINT('Ctrl Pts',(2.295793670099,20.2673681898868,-15.200636761067));
#36066=CARTESIAN_POINT('Ctrl Pts',(1.43801852688975,20.2421246596599,-13.5357989572919));
#36067=CARTESIAN_POINT('Ctrl Pts',(1.23821496048648,20.2357981340653,-13.1320096374851));
#36068=CARTESIAN_POINT('Ctrl Pts',(1.04527883727151,20.2292648564311,-12.7257013789351));
#36069=CARTESIAN_POINT('Ctrl Pts',(41.4945844892592,21.3428689572265,-36.094304790847));
#36070=CARTESIAN_POINT('Ctrl Pts',(41.0429495192362,21.323266505305,-36.1254953689207));
#36071=CARTESIAN_POINT('Ctrl Pts',(40.5893642151814,21.303930781031,-36.1494374678826));
#36072=CARTESIAN_POINT('Ctrl Pts',(38.6517079921192,21.2228186866547,-36.2200003189353));
#36073=CARTESIAN_POINT('Ctrl Pts',(35.7140114028846,21.1072213437662,-36.1696957800508));
#36074=CARTESIAN_POINT('Ctrl Pts',(31.4138119300288,20.9604400919523,-35.6401393145224));
#36075=CARTESIAN_POINT('Ctrl Pts',(26.5514224411379,20.819779963638,-34.5167581668256));
#36076=CARTESIAN_POINT('Ctrl Pts',(21.9203087230707,20.7152993064879,-32.791775100868));
#36077=CARTESIAN_POINT('Ctrl Pts',(17.5777272210475,20.6406553883908,-30.5109957831435));
#36078=CARTESIAN_POINT('Ctrl Pts',(13.4964895293743,20.5849601975755,-27.8101859299812));
#36079=CARTESIAN_POINT('Ctrl Pts',(9.7800037342825,20.5461109852346,-24.6152063244202));
#36080=CARTESIAN_POINT('Ctrl Pts',(6.48513371352389,20.5119420676311,-20.972735385183));
#36081=CARTESIAN_POINT('Ctrl Pts',(3.97592039392024,20.4797911688045,-17.5652597461339));
#36082=CARTESIAN_POINT('Ctrl Pts',(2.53023120471821,20.4522911786996,-15.1177639611188));
#36083=CARTESIAN_POINT('Ctrl Pts',(1.65838523268764,20.4307901345004,-13.4524688277451));
#36084=CARTESIAN_POINT('Ctrl Pts',(1.45518607757715,20.4253683033402,-13.0485330144838));
#36085=CARTESIAN_POINT('Ctrl Pts',(1.25884986838775,20.4197421663948,-12.6420414452013));
#36086=CARTESIAN_POINT('Ctrl Pts',(4.81048155583834,19.9464420456703,-20.0720152820648));
#36087=CARTESIAN_POINT('Ctrl Pts',(7.81583634933486,20.0189549105364,-24.1684379665366));
#36088=CARTESIAN_POINT('Ctrl Pts',(11.6050705594528,20.0954766247834,-27.675487418123));
#36089=CARTESIAN_POINT('Ctrl Pts',(20.1650060536999,20.2752040736289,-33.1377027463891));
#36090=CARTESIAN_POINT('Ctrl Pts',(24.9348834609741,20.3824974081049,-35.0946221674948));
#36091=CARTESIAN_POINT('Ctrl Pts',(29.9069010447471,20.5529756002056,-36.0949172314264));
#36092=CARTESIAN_POINT('Ctrl Pts',(39.2217566406836,20.9435908393615,-36.8146184333826));
#36093=CARTESIAN_POINT('Ctrl Pts',(39.0665136990626,20.9358615047579,-36.8200995370388));
#36094=CARTESIAN_POINT('Ctrl Pts',(38.9112707574417,20.9281321701544,-36.825580640695));
#36095=CARTESIAN_POINT('Ctrl Pts',(38.7560278158208,20.9204028355509,-36.8310617443513));
#36096=CARTESIAN_POINT('Ctrl Pts',(23.2317336537277,20.1474693751975,-37.3791721099748));
#36097=CARTESIAN_POINT('Ctrl Pts',(7.97122258304409,20.0812550388979,-28.0681800905232));
#36098=CARTESIAN_POINT('Ctrl Pts',(1.20708100656079,19.8399463130827,-14.0975769578644));
#36099=CARTESIAN_POINT('Ctrl Pts',(39.2216742354573,20.9469886892296,-36.8146659128868));
#36100=CARTESIAN_POINT('Ctrl Pts',(39.0664294181999,20.9392720585054,-36.8201548647248));
#36101=CARTESIAN_POINT('Ctrl Pts',(38.9111846009425,20.9315554277811,-36.8256438165629));
#36102=CARTESIAN_POINT('Ctrl Pts',(38.7559397836851,20.9238387970569,-36.831132768401));
#36103=CARTESIAN_POINT('Ctrl Pts',(23.2314580579417,20.1521757246323,-37.3800279522102));
#36104=CARTESIAN_POINT('Ctrl Pts',(7.9710320114852,20.0873688943554,-28.0685857559505));
#36105=CARTESIAN_POINT('Ctrl Pts',(1.20670795938283,19.8474084919615,-14.0981560611673));
#36106=CARTESIAN_POINT('Ctrl Pts',(39.2215918302311,20.9503865390978,-36.8147133923909));
#36107=CARTESIAN_POINT('Ctrl Pts',(39.0663451373372,20.9426826122528,-36.8202101924109));
#36108=CARTESIAN_POINT('Ctrl Pts',(38.9110984444433,20.9349786854078,-36.8257069924308));
#36109=CARTESIAN_POINT('Ctrl Pts',(38.7558517515493,20.9272747585629,-36.8312037924508));
#36110=CARTESIAN_POINT('Ctrl Pts',(23.2311824621557,20.1568820740671,-37.3808837944456));
#36111=CARTESIAN_POINT('Ctrl Pts',(7.97084143992632,20.093482749813,-28.0689914213779));
#36112=CARTESIAN_POINT('Ctrl Pts',(1.20633491220488,19.8548706708402,-14.0987351644701));
#36113=CARTESIAN_POINT('Ctrl Pts',(39.2215094250049,20.9537843889659,-36.8147608718951));
#36114=CARTESIAN_POINT('Ctrl Pts',(39.0662608564745,20.9460931660003,-36.8202655200969));
#36115=CARTESIAN_POINT('Ctrl Pts',(38.911012287944,20.9384019430346,-36.8257701682987));
#36116=CARTESIAN_POINT('Ctrl Pts',(38.7557637194136,20.9307107200689,-36.8312748165005));
#36117=CARTESIAN_POINT('Ctrl Pts',(23.2309068663697,20.1615884235019,-37.3817396366809));
#36118=CARTESIAN_POINT('Ctrl Pts',(7.97065086836744,20.0995966052706,-28.0693970868052));
#36119=CARTESIAN_POINT('Ctrl Pts',(1.20596186502693,19.862332849719,-14.099314267773));
#36120=CARTESIAN_POINT('Ctrl Pts',(39.2212591820617,20.9641027630587,-36.8149050546298));
#36121=CARTESIAN_POINT('Ctrl Pts',(39.0660049177178,20.9564501184246,-36.8204335356904));
#36122=CARTESIAN_POINT('Ctrl Pts',(38.9107506533739,20.9487974737906,-36.8259620167511));
#36123=CARTESIAN_POINT('Ctrl Pts',(38.75549638903,20.9411448291565,-36.8314904978117));
#36124=CARTESIAN_POINT('Ctrl Pts',(23.2300699546376,20.1758803657488,-37.3843386038783));
#36125=CARTESIAN_POINT('Ctrl Pts',(7.97007215279367,20.1181627721728,-28.0706289857407));
#36126=CARTESIAN_POINT('Ctrl Pts',(1.20482901911385,19.8849935193208,-14.1010728518038));
#36127=CARTESIAN_POINT('Ctrl Pts',(39.2207586959266,20.9847395112521,-36.8151934199635));
#36128=CARTESIAN_POINT('Ctrl Pts',(39.0654930400387,20.9771640232786,-36.8207695667871));
#36129=CARTESIAN_POINT('Ctrl Pts',(38.9102273841508,20.9695885353052,-36.8263457136107));
#36130=CARTESIAN_POINT('Ctrl Pts',(38.754961728263,20.9620130473318,-36.8319218604343));
#36131=CARTESIAN_POINT('Ctrl Pts',(23.2283961394753,20.2044642499886,-37.3895365427941));
#36132=CARTESIAN_POINT('Ctrl Pts',(7.96891471649109,20.1552951062578,-28.0730927828742));
#36133=CARTESIAN_POINT('Ctrl Pts',(1.20256332728765,19.9303148585245,-14.1045900198654));
#36134=CARTESIAN_POINT('Ctrl Pts',(39.2200079497906,21.0156946339229,-36.815625959386));
#36135=CARTESIAN_POINT('Ctrl Pts',(39.0647252122311,21.0082348808134,-36.8212736077134));
#36136=CARTESIAN_POINT('Ctrl Pts',(38.9094424746716,21.000775127704,-36.8269212560407));
#36137=CARTESIAN_POINT('Ctrl Pts',(38.7541597371122,20.9933153745945,-36.832568904368));
#36138=CARTESIAN_POINT('Ctrl Pts',(23.2258859811651,20.2473400636495,-37.3973337371021));
#36139=CARTESIAN_POINT('Ctrl Pts',(7.96717824152021,20.2109936225946,-28.0767884392132));
#36140=CARTESIAN_POINT('Ctrl Pts',(1.19916478954841,19.9982968673298,-14.1098657719579));
#36141=CARTESIAN_POINT('Ctrl Pts',(39.2192571813942,21.0466497571015,-36.8160584875007));
#36142=CARTESIAN_POINT('Ctrl Pts',(39.0639573695833,21.0393057386868,-36.8217776411011));
#36143=CARTESIAN_POINT('Ctrl Pts',(38.9086575577724,21.0319617202721,-36.8274967947015));
#36144=CARTESIAN_POINT('Ctrl Pts',(38.7533577459615,21.0246177018574,-36.8332159483019));
#36145=CARTESIAN_POINT('Ctrl Pts',(23.223376564873,20.2902158603888,-37.4051313083389));
#36146=CARTESIAN_POINT('Ctrl Pts',(7.96544134300785,20.2666921589687,-28.0804840413609));
#36147=CARTESIAN_POINT('Ctrl Pts',(1.19576625180914,20.0662788761352,-14.1151415240503));
#36148=CARTESIAN_POINT('Ctrl Pts',(39.2187566579113,21.0672865061488,-36.8163468338515));
#36149=CARTESIAN_POINT('Ctrl Pts',(39.0634454670057,21.0600196441101,-36.8221136595425));
#36150=CARTESIAN_POINT('Ctrl Pts',(38.9081342761,21.0527527820714,-36.8278804852334));
#36151=CARTESIAN_POINT('Ctrl Pts',(38.7528230851944,21.0454859200326,-36.8336473109243));
#36152=CARTESIAN_POINT('Ctrl Pts',(23.2217039946289,20.3187997161584,-37.4103298800174));
#36153=CARTESIAN_POINT('Ctrl Pts',(7.96428319555438,20.3038245267329,-28.0829477473042));
#36154=CARTESIAN_POINT('Ctrl Pts',(1.19350055998297,20.1116002153389,-14.1186586921119));
#36155=CARTESIAN_POINT('Ctrl Pts',(39.2185063960488,21.0776048806767,-36.8164910069587));
#36156=CARTESIAN_POINT('Ctrl Pts',(39.0631895156361,21.0703765968246,-36.8222816687177));
#36157=CARTESIAN_POINT('Ctrl Pts',(38.9078726352235,21.0631483129724,-36.8280723304767));
#36158=CARTESIAN_POINT('Ctrl Pts',(38.7525557548108,21.0559200291202,-36.8338629922356));
#36159=CARTESIAN_POINT('Ctrl Pts',(23.2208677135466,20.3330916439037,-37.4129291681314));
#36160=CARTESIAN_POINT('Ctrl Pts',(7.96370411918316,20.3223907107576,-28.0841795997822));
#36161=CARTESIAN_POINT('Ctrl Pts',(1.19236771406988,20.1342608849406,-14.1204172761427));
#36162=CARTESIAN_POINT('Ctrl Pts',(39.2184822807631,21.0785991614118,-36.8165048995096));
#36163=CARTESIAN_POINT('Ctrl Pts',(39.0631648521084,21.0713745949617,-36.8222978581171));
#36164=CARTESIAN_POINT('Ctrl Pts',(38.9078474234537,21.0641500285117,-36.8280908167246));
#36165=CARTESIAN_POINT('Ctrl Pts',(38.752529994799,21.0569254620617,-36.833883775332));
#36166=CARTESIAN_POINT('Ctrl Pts',(23.220787129326,20.3344688170607,-37.4131796360796));
#36167=CARTESIAN_POINT('Ctrl Pts',(7.9636483192625,20.3241797521467,-28.0842983013455));
#36168=CARTESIAN_POINT('Ctrl Pts',(1.19225855279994,20.1364444718193,-14.120586733669));
#36169=CARTESIAN_POINT('Ctrl Pts',(39.2184581654775,21.0795934421468,-36.8165187920605));
#36170=CARTESIAN_POINT('Ctrl Pts',(39.0631401885807,21.0723725930989,-36.8223140475165));
#36171=CARTESIAN_POINT('Ctrl Pts',(38.9078222116839,21.0651517440511,-36.8281093029725));
#36172=CARTESIAN_POINT('Ctrl Pts',(38.7525042347871,21.0579308950032,-36.8339045584284));
#36173=CARTESIAN_POINT('Ctrl Pts',(23.2207065451054,20.3358459902176,-37.4134301040277));
#36174=CARTESIAN_POINT('Ctrl Pts',(7.96359251934184,20.3259687935359,-28.0844170029088));
#36175=CARTESIAN_POINT('Ctrl Pts',(1.19214939153001,20.1386280586979,-14.1207561911953));
#36176=CARTESIAN_POINT('Ctrl Pts',(39.2184340501919,21.0805877228818,-36.8165326846113));
#36177=CARTESIAN_POINT('Ctrl Pts',(39.063115525053,21.0733705912361,-36.8223302369158));
#36178=CARTESIAN_POINT('Ctrl Pts',(38.9077969999141,21.0661534595904,-36.8281277892204));
#36179=CARTESIAN_POINT('Ctrl Pts',(38.7524784747752,21.0589363279447,-36.8339253415249));
#36180=CARTESIAN_POINT('Ctrl Pts',(23.2206259608848,20.3372231633746,-37.4136805719759));
#36181=CARTESIAN_POINT('Ctrl Pts',(7.96353671942118,20.327757834925,-28.0845357044721));
#36182=CARTESIAN_POINT('Ctrl Pts',(1.19204023026007,20.1408116455766,-14.1209256487216));
#36183=CARTESIAN_POINT('Ctrl Pts',(54.096233416894,21.2883239772394,9.98352735473641));
#36184=CARTESIAN_POINT('Ctrl Pts',(53.8409594097646,21.2711623310641,9.61248528230055));
#36185=CARTESIAN_POINT('Ctrl Pts',(53.5788530977531,21.2542807820542,9.24441890854599));
#36186=CARTESIAN_POINT('Ctrl Pts',(52.4311812489649,21.1834525291307,7.68716578714771));
#36187=CARTESIAN_POINT('Ctrl Pts',(50.5662584013097,21.0834264338425,5.42184195082861));
#36188=CARTESIAN_POINT('Ctrl Pts',(47.4787450278816,20.9598507183575,2.3893977933402));
#36189=CARTESIAN_POINT('Ctrl Pts',(43.575989077353,20.8461335954997,-0.713114551264511));
#36190=CARTESIAN_POINT('Ctrl Pts',(39.3448124775761,20.7684839093916,-3.2603433732672));
#36191=CARTESIAN_POINT('Ctrl Pts',(34.8565666606213,20.7206230093664,-5.23576668658806));
#36192=CARTESIAN_POINT('Ctrl Pts',(30.2008472528554,20.6916936542703,-6.74506250497749));
#36193=CARTESIAN_POINT('Ctrl Pts',(25.3835553034033,20.6796111419738,-7.66097308304403));
#36194=CARTESIAN_POINT('Ctrl Pts',(20.4764910470132,20.6722203558656,-7.96784585316283));
#36195=CARTESIAN_POINT('Ctrl Pts',(16.2417385179411,20.6630225594897,-7.80630362792482));
#36196=CARTESIAN_POINT('Ctrl Pts',(13.4213391185488,20.6508204531822,-7.4110411108956));
#36197=CARTESIAN_POINT('Ctrl Pts',(11.5740620400678,20.6394053700742,-7.05498278350414));
#36198=CARTESIAN_POINT('Ctrl Pts',(11.132952210758,20.6364191357732,-6.96256671604898));
#36199=CARTESIAN_POINT('Ctrl Pts',(10.694125226444,20.6332209087108,-6.8632653171979));
#36200=CARTESIAN_POINT('Ctrl Pts',(53.9830369457162,21.2398788304839,9.46171406818988));
#36201=CARTESIAN_POINT('Ctrl Pts',(53.7266004689061,21.2217224127637,9.09271470601715));
#36202=CARTESIAN_POINT('Ctrl Pts',(53.4633475549858,21.2038412173392,8.7267144505681));
#36203=CARTESIAN_POINT('Ctrl Pts',(52.3108518161382,21.1287309618461,7.17837913463006));
#36204=CARTESIAN_POINT('Ctrl Pts',(50.4392773471876,21.0222253289507,4.92722374819142));
#36205=CARTESIAN_POINT('Ctrl Pts',(47.3441140086114,20.8890564489947,1.91734732260939));
#36206=CARTESIAN_POINT('Ctrl Pts',(43.4352890996597,20.7641817659416,-1.15756126347997));
#36207=CARTESIAN_POINT('Ctrl Pts',(39.2017861763524,20.6752847595175,-3.67591975391337));
#36208=CARTESIAN_POINT('Ctrl Pts',(34.7152142664626,20.6159219251614,-5.62169100966009));
#36209=CARTESIAN_POINT('Ctrl Pts',(30.0645001982276,20.5752144761384,-7.1009771020976));
#36210=CARTESIAN_POINT('Ctrl Pts',(25.2565486693757,20.5509334123338,-7.98675116083998));
#36211=CARTESIAN_POINT('Ctrl Pts',(20.3634163558495,20.5308579865904,-8.26383905577707));
#36212=CARTESIAN_POINT('Ctrl Pts',(16.1438739001623,20.510426256151,-8.07723388342209));
#36213=CARTESIAN_POINT('Ctrl Pts',(13.335881648162,20.4905046142392,-7.66570489790757));
#36214=CARTESIAN_POINT('Ctrl Pts',(11.4975417212571,20.4739374093561,-7.29913696623926));
#36215=CARTESIAN_POINT('Ctrl Pts',(11.0586072647004,20.469713411733,-7.2042182379738));
#36216=CARTESIAN_POINT('Ctrl Pts',(10.6219862286722,20.4652767483487,-7.10243434478152));
#36217=CARTESIAN_POINT('Ctrl Pts',(53.8697370177666,21.1822016013635,8.93970129386049));
#36218=CARTESIAN_POINT('Ctrl Pts',(53.6121351567703,21.1630886105529,8.57276400445957));
#36219=CARTESIAN_POINT('Ctrl Pts',(53.3477329763492,21.1442460408093,8.20884980300576));
#36220=CARTESIAN_POINT('Ctrl Pts',(52.1904032008889,21.0650173413637,6.66951987973133));
#36221=CARTESIAN_POINT('Ctrl Pts',(50.312164897738,20.9522796229575,4.4326664265343));
#36222=CARTESIAN_POINT('Ctrl Pts',(47.2093446045204,20.8098799445818,1.44556050267551));
#36223=CARTESIAN_POINT('Ctrl Pts',(43.2944576422004,20.6742608619688,-1.60149992344141));
#36224=CARTESIAN_POINT('Ctrl Pts',(39.0586575078325,20.5745198093833,-4.09072706669367));
#36225=CARTESIAN_POINT('Ctrl Pts',(34.5738153175261,20.5040526001987,-6.00656185447961));
#36226=CARTESIAN_POINT('Ctrl Pts',(29.9281883187936,20.4519664047462,-7.45552706604719));
#36227=CARTESIAN_POINT('Ctrl Pts',(25.1296932182711,20.4158956934967,-8.31081715048489));
#36228=CARTESIAN_POINT('Ctrl Pts',(20.250643895266,20.3835681705302,-8.55773188003308));
#36229=CARTESIAN_POINT('Ctrl Pts',(16.0464632313985,20.3523071857454,-8.34569622092367));
#36230=CARTESIAN_POINT('Ctrl Pts',(13.2509884095923,20.3249607749065,-7.91763736285362));
#36231=CARTESIAN_POINT('Ctrl Pts',(11.4216589411055,20.3034475984546,-7.5403803228002));
#36232=CARTESIAN_POINT('Ctrl Pts',(10.9849194872874,20.2980359714688,-7.44291568157701));
#36233=CARTESIAN_POINT('Ctrl Pts',(10.5505259893207,20.29241155197,-7.33860589683737));
#36234=CARTESIAN_POINT('Ctrl Pts',(53.4644633086927,20.942701117012,7.07354901688149));
#36235=CARTESIAN_POINT('Ctrl Pts',(53.2026883461185,20.9203083949833,6.71404688513704));
#36236=CARTESIAN_POINT('Ctrl Pts',(52.9341714587248,20.898168919688,6.35765679911698));
#36237=CARTESIAN_POINT('Ctrl Pts',(51.7595381232525,20.8048139743737,4.85081887924358));
#36238=CARTESIAN_POINT('Ctrl Pts',(49.857453155798,20.6706999592586,2.66554851920846));
#36239=CARTESIAN_POINT('Ctrl Pts',(46.7272593393429,20.496623371127,-0.239462178198342));
#36240=CARTESIAN_POINT('Ctrl Pts',(42.7907482839516,20.3241023157428,-3.18613007185183));
#36241=CARTESIAN_POINT('Ctrl Pts',(38.5468554926957,20.1870685788371,-5.5703146686724));
#36242=CARTESIAN_POINT('Ctrl Pts',(34.0684049418232,20.0783595881962,-7.37814069679685));
#36243=CARTESIAN_POINT('Ctrl Pts',(29.4412586748499,19.9870599496472,-8.71762346866089));
#36244=CARTESIAN_POINT('Ctrl Pts',(24.6769789007594,19.9103458023656,-9.46271295215423));
#36245=CARTESIAN_POINT('Ctrl Pts',(19.8487996392098,19.8358125374395,-9.60038699181189));
#36246=CARTESIAN_POINT('Ctrl Pts',(15.7000560750932,19.767331746443,-9.29613511960772));
#36247=CARTESIAN_POINT('Ctrl Pts',(12.9497018486459,19.7145309927478,-8.8080470657374));
#36248=CARTESIAN_POINT('Ctrl Pts',(11.1528281593933,19.6760973304852,-8.39193939128734));
#36249=CARTESIAN_POINT('Ctrl Pts',(10.724004523227,19.6666248028076,-8.28521939042578));
#36250=CARTESIAN_POINT('Ctrl Pts',(10.2976530603138,19.6569408091057,-8.17172515586503));
#36251=CARTESIAN_POINT('Ctrl Pts',(52.8863153515536,20.4780024533914,4.41539935052617));
#36252=CARTESIAN_POINT('Ctrl Pts',(52.6185716797916,20.4514551579611,4.06672732948473));
#36253=CARTESIAN_POINT('Ctrl Pts',(52.344171576181,20.4251375618498,3.72130358184864));
#36254=CARTESIAN_POINT('Ctrl Pts',(51.1448075867849,20.3138746691076,2.2618508394985));
#36255=CARTESIAN_POINT('Ctrl Pts',(49.208673544985,20.1526659052326,0.151770647364792));
#36256=CARTESIAN_POINT('Ctrl Pts',(46.0395105548711,19.938389785095,-2.63365452435864));
#36257=CARTESIAN_POINT('Ctrl Pts',(42.0723996256245,19.7189203495023,-5.434144257564));
#36258=CARTESIAN_POINT('Ctrl Pts',(37.817410701173,19.5342279169114,-7.66541815032562));
#36259=CARTESIAN_POINT('Ctrl Pts',(33.3487384781665,19.3763677050182,-9.3160029447135));
#36260=CARTESIAN_POINT('Ctrl Pts',(28.7487915843048,19.2344308170631,-10.4960634080756));
#36261=CARTESIAN_POINT('Ctrl Pts',(24.0343837367008,19.1049298841923,-11.0806082778795));
#36262=CARTESIAN_POINT('Ctrl Pts',(19.2800719812092,18.9752993129734,-11.0590103243977));
#36263=CARTESIAN_POINT('Ctrl Pts',(15.2116924680306,18.8580619466085,-10.6201973999149));
#36264=CARTESIAN_POINT('Ctrl Pts',(12.5266729066911,18.7718242877839,-10.044424156308));
#36265=CARTESIAN_POINT('Ctrl Pts',(10.7767743381542,18.7111415689428,-9.57153073773204));
#36266=CARTESIAN_POINT('Ctrl Pts',(10.3594275150096,18.6963263828107,-9.45128055628077));
#36267=CARTESIAN_POINT('Ctrl Pts',(9.94475486011823,18.6812985797984,-9.32435816539428));
#36268=CARTESIAN_POINT('Ctrl Pts',(52.0406002125752,19.4355555088431,0.536630679855416));
#36269=CARTESIAN_POINT('Ctrl Pts',(51.7640075955767,19.4044605226273,0.204462065251584));
#36270=CARTESIAN_POINT('Ctrl Pts',(51.4808914055444,19.3735658358572,-0.124235214003335));
#36271=CARTESIAN_POINT('Ctrl Pts',(50.2449190227734,19.2426748194849,-1.51134745512144));
#36272=CARTESIAN_POINT('Ctrl Pts',(48.2584669237558,19.0517849995255,-3.50670891787662));
#36273=CARTESIAN_POINT('Ctrl Pts',(45.0320086735472,18.7933185397158,-6.10982075851879));
#36274=CARTESIAN_POINT('Ctrl Pts',(41.020376532225,18.5218580841843,-8.68754002034028));
#36275=CARTESIAN_POINT('Ctrl Pts',(36.7501523857616,18.2836948825759,-10.685800216972));
#36276=CARTESIAN_POINT('Ctrl Pts',(32.2975809316394,18.0697821020849,-12.0966666900533));
#36277=CARTESIAN_POINT('Ctrl Pts',(27.7398821156923,17.8693333343866,-13.0335373077252));
#36278=CARTESIAN_POINT('Ctrl Pts',(23.1017460362113,17.6778661310593,-13.3729183254776));
#36279=CARTESIAN_POINT('Ctrl Pts',(18.4597065884447,17.4826662284719,-13.1077148144475));
#36280=CARTESIAN_POINT('Ctrl Pts',(14.5131353656531,17.3068805329357,-12.4627659844579));
#36281=CARTESIAN_POINT('Ctrl Pts',(11.926957780631,17.1802068447994,-11.7524052617819));
#36282=CARTESIAN_POINT('Ctrl Pts',(10.2480732137341,17.0925519552341,-11.192249695301));
#36283=CARTESIAN_POINT('Ctrl Pts',(9.84812468771829,17.0712544126695,-11.0512080030603));
#36284=CARTESIAN_POINT('Ctrl Pts',(9.45120285539089,17.0497370990139,-10.9036522294195));
#36285=CARTESIAN_POINT('Ctrl Pts',(51.0842942568547,17.8320672383652,-3.84088922097839));
#36286=CARTESIAN_POINT('Ctrl Pts',(50.7974662443455,17.7976045693245,-4.1536391251297));
#36287=CARTESIAN_POINT('Ctrl Pts',(50.5042776068662,17.7633163796081,-4.46263132338155));
#36288=CARTESIAN_POINT('Ctrl Pts',(49.2260465041698,17.6178640028275,-5.7644191441608));
#36289=CARTESIAN_POINT('Ctrl Pts',(47.1815905690377,17.4049846203341,-7.62450873541984));
#36290=CARTESIAN_POINT('Ctrl Pts',(43.8893661957293,17.1135517229592,-10.0126928844568));
#36291=CARTESIAN_POINT('Ctrl Pts',(39.827079861979,16.8027253827761,-12.3277800623226));
#36292=CARTESIAN_POINT('Ctrl Pts',(35.5404007724829,16.523022337621,-14.0512431159597));
#36293=CARTESIAN_POINT('Ctrl Pts',(31.1079579099481,16.2641978724915,-15.1792080319066));
#36294=CARTESIAN_POINT('Ctrl Pts',(26.6009083346784,16.0157341831644,-15.8288669477005));
#36295=CARTESIAN_POINT('Ctrl Pts',(22.0531293441551,15.7719994721116,-15.8783661204877));
#36296=CARTESIAN_POINT('Ctrl Pts',(17.5434519798272,15.5202180684676,-15.3246701276807));
#36297=CARTESIAN_POINT('Ctrl Pts',(13.7401700421149,15.2931736272884,-14.4352340302876));
#36298=CARTESIAN_POINT('Ctrl Pts',(11.2700908184494,15.130708702949,-13.5649582362775));
#36299=CARTESIAN_POINT('Ctrl Pts',(9.67456871062958,15.0190926843839,-12.9010089872194));
#36300=CARTESIAN_POINT('Ctrl Pts',(9.29511173349696,14.9920326361705,-12.7352506969355));
#36301=CARTESIAN_POINT('Ctrl Pts',(8.91916102165301,14.9647422323135,-12.5631815717126));
#36302=CARTESIAN_POINT('Ctrl Pts',(50.1725377178788,15.7638142683891,-8.00723153985461));
#36303=CARTESIAN_POINT('Ctrl Pts',(49.8755477488999,15.7283726072843,-8.30050397680349));
#36304=CARTESIAN_POINT('Ctrl Pts',(49.5723712501119,15.6930928161318,-8.58970540631576));
#36305=CARTESIAN_POINT('Ctrl Pts',(48.2522976624192,15.543379415412,-9.80568727794157));
#36306=CARTESIAN_POINT('Ctrl Pts',(46.1504868067129,15.3241289383934,-11.5297341520232));
#36307=CARTESIAN_POINT('Ctrl Pts',(42.7935015732012,15.0227233638938,-13.7016902252622));
#36308=CARTESIAN_POINT('Ctrl Pts',(38.6817671766857,14.6988957424381,-15.7524134665736));
#36309=CARTESIAN_POINT('Ctrl Pts',(34.3798754649118,14.4035050799014,-17.1990244745944));
#36310=CARTESIAN_POINT('Ctrl Pts',(29.9688301701935,14.1252237593235,-18.0416345493436));
#36311=CARTESIAN_POINT('Ctrl Pts',(25.5137144392418,13.8539516979883,-18.4012723388184));
#36312=CARTESIAN_POINT('Ctrl Pts',(21.0575892960011,13.5829362127958,-18.1575891929838));
#36313=CARTESIAN_POINT('Ctrl Pts',(16.6815712532013,13.2994842764397,-17.3115432147165));
#36314=CARTESIAN_POINT('Ctrl Pts',(13.0226854098743,13.0425486753816,-16.1739021884697));
#36315=CARTESIAN_POINT('Ctrl Pts',(10.6694354351882,12.8585920936854,-15.1409396349232));
#36316=CARTESIAN_POINT('Ctrl Pts',(9.1577531507647,12.7324540777387,-14.3712708374681));
#36317=CARTESIAN_POINT('Ctrl Pts',(8.79897600642064,12.7018988467546,-14.1803688483644));
#36318=CARTESIAN_POINT('Ctrl Pts',(8.44425573048895,12.6711030837425,-13.9833955784899));
#36319=CARTESIAN_POINT('Ctrl Pts',(49.3152608397176,13.2592937677246,-11.9222078443566));
#36320=CARTESIAN_POINT('Ctrl Pts',(49.0081288955748,13.2252177231213,-12.1961718735344));
#36321=CARTESIAN_POINT('Ctrl Pts',(48.6949962864853,13.191306123502,-12.4657287651272));
#36322=CARTESIAN_POINT('Ctrl Pts',(47.3332740813492,13.0474600457288,-13.596431013652));
#36323=CARTESIAN_POINT('Ctrl Pts',(45.1744154124219,12.8372075593629,-15.1851844684315));
#36324=CARTESIAN_POINT('Ctrl Pts',(41.7531577370126,12.5484949329477,-17.1418284947311));
#36325=CARTESIAN_POINT('Ctrl Pts',(37.5925733551791,12.2377054846042,-18.9289743222429));
#36326=CARTESIAN_POINT('Ctrl Pts',(33.2760966864303,11.9522310106351,-20.0991214081145));
#36327=CARTESIAN_POINT('Ctrl Pts',(28.8870963556916,11.6797819251771,-20.6563051510431));
#36328=CARTESIAN_POINT('Ctrl Pts',(24.4845718229607,11.4108111467242,-20.725453230849));
#36329=CARTESIAN_POINT('Ctrl Pts',(20.1207628048483,11.1374939458242,-20.1875872960187));
#36330=CARTESIAN_POINT('Ctrl Pts',(15.8790594562062,10.8473681096278,-19.0476098848715));
#36331=CARTESIAN_POINT('Ctrl Pts',(12.3651212340625,10.5820480444149,-17.6599891786549));
#36332=CARTESIAN_POINT('Ctrl Pts',(10.1290577747649,10.3910369789073,-16.4628640701335));
#36333=CARTESIAN_POINT('Ctrl Pts',(8.70144575840633,10.2599216927486,-15.5864046825366));
#36334=CARTESIAN_POINT('Ctrl Pts',(8.36346441706814,10.2281653805015,-15.3701525403304));
#36335=CARTESIAN_POINT('Ctrl Pts',(8.03014834074206,10.1961599190035,-15.1481197425553));
#36336=CARTESIAN_POINT('Ctrl Pts',(48.5068954184471,10.420684636249,-15.6143972186621));
#36337=CARTESIAN_POINT('Ctrl Pts',(48.1896003239712,10.3898269637342,-15.8693164159478));
#36338=CARTESIAN_POINT('Ctrl Pts',(47.8665042940188,10.3591499865554,-16.1194724741786));
#36339=CARTESIAN_POINT('Ctrl Pts',(46.463169475174,10.2291883131935,-17.1658511436441));
#36340=CARTESIAN_POINT('Ctrl Pts',(44.2473255358791,10.0401067219452,-18.6207182709661));
#36341=CARTESIAN_POINT('Ctrl Pts',(40.7619090059636,9.78206378055234,-20.3639629021039));
#36342=CARTESIAN_POINT('Ctrl Pts',(36.5526268350307,9.50499638561923,-21.8895038071216));
#36343=CARTESIAN_POINT('Ctrl Pts',(32.2217373255655,9.24981780003299,-22.7848040491436));
#36344=CARTESIAN_POINT('Ctrl Pts',(27.8549660182239,9.00337535985762,-23.057781793126));
#36345=CARTESIAN_POINT('Ctrl Pts',(23.5052216104395,8.75677479408939,-22.8373239688022));
#36346=CARTESIAN_POINT('Ctrl Pts',(19.2339176885499,8.50116890088297,-22.0057156544696));
#36347=CARTESIAN_POINT('Ctrl Pts',(15.1267085905075,8.22444592813344,-20.5717738964972));
#36348=CARTESIAN_POINT('Ctrl Pts',(11.757861066389,7.96804930448713,-18.9338087527527));
#36349=CARTESIAN_POINT('Ctrl Pts',(9.63906942037282,7.78162503245108,-17.5720463596553));
#36350=CARTESIAN_POINT('Ctrl Pts',(8.29557955058743,7.65323614745839,-16.5884059526543));
#36351=CARTESIAN_POINT('Ctrl Pts',(7.97844957882663,7.62212996336316,-16.3467742297976));
#36352=CARTESIAN_POINT('Ctrl Pts',(7.66663340357728,7.59076668565169,-16.0997163540814));
#36353=CARTESIAN_POINT('Ctrl Pts',(47.7663041384592,7.18298363715391,-19.0008728096664));
#36354=CARTESIAN_POINT('Ctrl Pts',(47.4387949271775,7.15763661423686,-19.2372123412692));
#36355=CARTESIAN_POINT('Ctrl Pts',(47.1056968685837,7.13250342173354,-19.4684182906929));
#36356=CARTESIAN_POINT('Ctrl Pts',(45.6606453368009,7.02634360727853,-20.4323367979011));
#36357=CARTESIAN_POINT('Ctrl Pts',(43.3876649619329,6.87350147707393,-21.7560858428746));
#36358=CARTESIAN_POINT('Ctrl Pts',(39.8378843858508,6.66841421880391,-23.2897975200252));
#36359=CARTESIAN_POINT('Ctrl Pts',(35.5796858561183,6.45075222930465,-24.557880503093));
#36360=CARTESIAN_POINT('Ctrl Pts',(31.2341850293128,6.25122984378583,-25.181992433157));
#36361=CARTESIAN_POINT('Ctrl Pts',(26.8894543185663,6.05595707526583,-25.1738921979679));
#36362=CARTESIAN_POINT('Ctrl Pts',(22.592303780841,5.8568061689083,-24.6665137174336));
#36363=CARTESIAN_POINT('Ctrl Pts',(18.4133138682224,5.64398234710963,-23.5432735796297));
#36364=CARTESIAN_POINT('Ctrl Pts',(14.4403913295249,5.40587468584602,-21.8168778028767));
#36365=CARTESIAN_POINT('Ctrl Pts',(11.2164396726889,5.18017895256177,-19.9294422021648));
#36366=CARTESIAN_POINT('Ctrl Pts',(9.21477519698173,5.01301666232781,-18.4033400289031));
#36367=CARTESIAN_POINT('Ctrl Pts',(7.9553063361445,4.89707445701614,-17.3126195831835));
#36368=CARTESIAN_POINT('Ctrl Pts',(7.65902789693625,4.86894780999335,-17.0457039568974));
#36369=CARTESIAN_POINT('Ctrl Pts',(7.3687334895065,4.84055053954568,-16.773786950835));
#36370=CARTESIAN_POINT('Ctrl Pts',(47.1034759657558,3.57357815210241,-22.0401821714072));
#36371=CARTESIAN_POINT('Ctrl Pts',(46.7656567924019,3.55599962931061,-22.258629623147));
#36372=CARTESIAN_POINT('Ctrl Pts',(46.422469525106,3.53868515668548,-22.4715649470704));
#36373=CARTESIAN_POINT('Ctrl Pts',(44.9353728299774,3.46609807861293,-23.3558908474528));
#36374=CARTESIAN_POINT('Ctrl Pts',(42.6047596053836,3.36435917107101,-24.5528077821968));
#36375=CARTESIAN_POINT('Ctrl Pts',(38.9898867387259,3.23426720235262,-25.883075497778));
#36376=CARTESIAN_POINT('Ctrl Pts',(34.6819369539376,3.10147907156715,-26.9003845437934));
#36377=CARTESIAN_POINT('Ctrl Pts',(30.3210023530336,2.98285053627008,-27.2594428206669));
#36378=CARTESIAN_POINT('Ctrl Pts',(25.9974922221956,2.86388130857434,-26.9758226313354));
#36379=CARTESIAN_POINT('Ctrl Pts',(21.7521116924467,2.73730530568202,-26.1866104301047));
#36380=CARTESIAN_POINT('Ctrl Pts',(17.6645996841604,2.59247375589619,-24.7762264723451));
#36381=CARTESIAN_POINT('Ctrl Pts',(13.8251038305928,2.41842603756845,-22.7612587515336));
#36382=CARTESIAN_POINT('Ctrl Pts',(10.745289428394,2.24547053120763,-20.6272650645164));
#36383=CARTESIAN_POINT('Ctrl Pts',(8.86022855638182,2.11246131963295,-18.9384898393954));
#36384=CARTESIAN_POINT('Ctrl Pts',(7.68442932568005,2.01884144332686,-17.7416968510392));
#36385=CARTESIAN_POINT('Ctrl Pts',(7.40891951245342,1.99605339732081,-17.4498093694952));
#36386=CARTESIAN_POINT('Ctrl Pts',(7.14006311638173,1.9729679754383,-17.1534135736909));
#36387=CARTESIAN_POINT('Ctrl Pts',(46.5932402567772,0.237308438758995,-24.3880208385881));
#36388=CARTESIAN_POINT('Ctrl Pts',(46.2464938933772,0.227921876287717,-24.5917084460452));
#36389=CARTESIAN_POINT('Ctrl Pts',(45.8945747997372,0.218854274805993,-24.789555458612));
#36390=CARTESIAN_POINT('Ctrl Pts',(44.3711113907725,0.181679983795775,-25.6080867216743));
#36391=CARTESIAN_POINT('Ctrl Pts',(41.9905999455746,0.133848323063104,-26.6999270667671));
#36392=CARTESIAN_POINT('Ctrl Pts',(38.3191944032503,0.0830496793456984,
-27.8610127422469));
#36393=CARTESIAN_POINT('Ctrl Pts',(33.9677453036371,0.0403924264632703,
-28.6691257307571));
#36394=CARTESIAN_POINT('Ctrl Pts',(29.592731205814,0.00837005963384143,
-28.8063457531801));
#36395=CARTESIAN_POINT('Ctrl Pts',(25.2865576591566,-0.0279539839125438,
-28.2915019174398));
#36396=CARTESIAN_POINT('Ctrl Pts',(21.0846934817227,-0.0750512999789021,
-27.2653201831544));
#36397=CARTESIAN_POINT('Ctrl Pts',(17.0747213437724,-0.14423024726241,-25.6129959380492));
#36398=CARTESIAN_POINT('Ctrl Pts',(13.3487019191347,-0.245792879606331,
-23.3544485950546));
#36399=CARTESIAN_POINT('Ctrl Pts',(10.3916545614428,-0.358291148292244,
-21.0120689099268));
#36400=CARTESIAN_POINT('Ctrl Pts',(8.60600662574962,-0.451704594358635,
-19.1856437846783));
#36401=CARTESIAN_POINT('Ctrl Pts',(7.50156840296396,-0.519340602547392,
-17.8990473762172));
#36402=CARTESIAN_POINT('Ctrl Pts',(7.24376168775053,-0.535923052101836,
-17.5860758002247));
#36403=CARTESIAN_POINT('Ctrl Pts',(6.9931674919517,-0.552841667182328,-17.2690690103583));
#36404=CARTESIAN_POINT('Ctrl Pts',(46.2947220098623,-2.14030259993981,-25.7688006063388));
#36405=CARTESIAN_POINT('Ctrl Pts',(45.941959111431,-2.14321532053782,-25.9630972825016));
#36406=CARTESIAN_POINT('Ctrl Pts',(45.5841524820316,-2.14576465810466,-26.15133557776));
#36407=CARTESIAN_POINT('Ctrl Pts',(44.036157375114,-2.15494826818845,-26.9279311689218));
#36408=CARTESIAN_POINT('Ctrl Pts',(41.6219424526533,-2.16016260296573,-27.9526124656332));
#36409=CARTESIAN_POINT('Ctrl Pts',(37.9121954585346,-2.1481556077715,-29.0050620130212));
#36410=CARTESIAN_POINT('Ctrl Pts',(33.5309876602201,-2.11918777525101,-29.678331446371));
#36411=CARTESIAN_POINT('Ctrl Pts',(29.1458287536112,-2.08197924289826,-29.6719949919839));
#36412=CARTESIAN_POINT('Ctrl Pts',(24.850450699298,-2.05170003121316,-29.0070497291441));
#36413=CARTESIAN_POINT('Ctrl Pts',(20.6768296464201,-2.03426137368081,-27.8267065281117));
#36414=CARTESIAN_POINT('Ctrl Pts',(16.7177727938086,-2.04135770257883,-26.0166226684537));
#36415=CARTESIAN_POINT('Ctrl Pts',(13.0666111841149,-2.08278583441843,-23.5989471937519));
#36416=CARTESIAN_POINT('Ctrl Pts',(10.1907160216954,-2.14471303148954,-21.1202535264619));
#36417=CARTESIAN_POINT('Ctrl Pts',(8.47087180152222,-2.20477046252904,-19.2036851023432));
#36418=CARTESIAN_POINT('Ctrl Pts',(7.4136936437243,-2.25046208753918,-17.8582514463191));
#36419=CARTESIAN_POINT('Ctrl Pts',(7.16760061362021,-2.26180965939547,-17.5314923980718));
#36420=CARTESIAN_POINT('Ctrl Pts',(6.92907933707999,-2.27353152926925,-17.2010333337206));
#36421=CARTESIAN_POINT('Ctrl Pts',(46.1037904071156,-3.83428286431684,-26.6551216886457));
#36422=CARTESIAN_POINT('Ctrl Pts',(45.7468392473426,-3.83237339034492,-26.8431064726811));
#36423=CARTESIAN_POINT('Ctrl Pts',(45.384933450483,-3.83006698099443,-27.0248826050977));
#36424=CARTESIAN_POINT('Ctrl Pts',(43.8198552158363,-3.81839846831683,-27.7732596177199));
#36425=CARTESIAN_POINT('Ctrl Pts',(41.3821512642932,-3.79185933798401,-28.7526727554059));
#36426=CARTESIAN_POINT('Ctrl Pts',(37.6456155051948,-3.73301479320489,-29.7316906927672));
#36427=CARTESIAN_POINT('Ctrl Pts',(33.2435059855666,-3.65055513724086,-30.3136066492174));
#36428=CARTESIAN_POINT('Ctrl Pts',(28.8510048450698,-3.56151400652134,-30.2097891824573));
#36429=CARTESIAN_POINT('Ctrl Pts',(24.5627595764646,-3.48120332570528,-29.4427347388257));
#36430=CARTESIAN_POINT('Ctrl Pts',(20.4083312364158,-3.41513875248544,-28.1573941121625));
#36431=CARTESIAN_POINT('Ctrl Pts',(16.4841372973616,-3.37526128513496,-26.2397257261537));
#36432=CARTESIAN_POINT('Ctrl Pts',(12.8843854212511,-3.37099617994084,-23.7134252414379));
#36433=CARTESIAN_POINT('Ctrl Pts',(10.0642958903975,-3.39437469848804,-21.1416193490947));
#36434=CARTESIAN_POINT('Ctrl Pts',(8.38974213062551,-3.42893690611626,-19.1634442433015));
#36435=CARTESIAN_POINT('Ctrl Pts',(7.36510236943545,-3.45783930783476,-17.7777914941477));
#36436=CARTESIAN_POINT('Ctrl Pts',(7.1270679382079,-3.46518513130081,-17.441619342386));
#36437=CARTESIAN_POINT('Ctrl Pts',(6.89684614274116,-3.47293757911652,-17.1019872449569));
#36438=CARTESIAN_POINT('Ctrl Pts',(46.0528159428914,-4.30636894546118,-26.8921103922779));
#36439=CARTESIAN_POINT('Ctrl Pts',(45.6947067519107,-4.3031084050989,-27.0783820415091));
#36440=CARTESIAN_POINT('Ctrl Pts',(45.3316670409603,-4.29944065268701,-27.2584034254891));
#36441=CARTESIAN_POINT('Ctrl Pts',(43.7618609679394,-4.28192251284736,-27.9991144594585));
#36442=CARTESIAN_POINT('Ctrl Pts',(41.3176536774688,-4.24645759656194,-28.9662083465854));
#36443=CARTESIAN_POINT('Ctrl Pts',(37.573695569515,-4.17439213330946,-29.9251866742588));
#36444=CARTESIAN_POINT('Ctrl Pts',(33.165788764262,-4.07676875425951,-30.4821188840162));
#36445=CARTESIAN_POINT('Ctrl Pts',(28.7712425645872,-3.97294922980807,-30.3515908256571));
#36446=CARTESIAN_POINT('Ctrl Pts',(24.4849562345802,-3.87828739688684,-29.5565265077524));
#36447=CARTESIAN_POINT('Ctrl Pts',(20.3358191796481,-3.79820251809058,-28.2423765542426));
#36448=CARTESIAN_POINT('Ctrl Pts',(16.4212365487571,-3.74469501429227,-26.2951939954818));
#36449=CARTESIAN_POINT('Ctrl Pts',(12.835640508744,-3.72710099262819,-23.7391203941118));
#36450=CARTESIAN_POINT('Ctrl Pts',(10.0308926410816,-3.7392015362719,-21.1418289429546));
#36451=CARTESIAN_POINT('Ctrl Pts',(8.36877216587862,-3.76629674044718,-19.1468130501193));
#36452=CARTESIAN_POINT('Ctrl Pts',(7.35305705617724,-3.79028538091932,-17.7501753024402));
#36453=CARTESIAN_POINT('Ctrl Pts',(7.11723098643449,-3.79646095010219,-17.4114340805589));
#36454=CARTESIAN_POINT('Ctrl Pts',(6.88928170242563,-3.80305340259771,-17.0693002554959));
#36455=CARTESIAN_POINT('Ctrl Pts',(46.0037076365571,-4.78145508078572,-27.120777531992));
#36456=CARTESIAN_POINT('Ctrl Pts',(45.6444433560399,-4.77682808742727,-27.305369940422));
#36457=CARTESIAN_POINT('Ctrl Pts',(45.2802717676693,-4.7717826224726,-27.4836706378466));
#36458=CARTESIAN_POINT('Ctrl Pts',(43.7057426010136,-4.74834091216943,-28.2168616760953));
#36459=CARTESIAN_POINT('Ctrl Pts',(41.2550359871502,-4.70381966688121,-29.1718493157503));
#36460=CARTESIAN_POINT('Ctrl Pts',(37.5036551789753,-4.61828583278682,-30.1110783850339));
#36461=CARTESIAN_POINT('Ctrl Pts',(33.0899455447831,-4.50515190400754,-30.6433355850274));
#36462=CARTESIAN_POINT('Ctrl Pts',(28.6933453214368,-4.38613315046716,-30.4863760222648));
#36463=CARTESIAN_POINT('Ctrl Pts',(24.4090037684511,-4.27662792828432,-29.6635634830365));
#36464=CARTESIAN_POINT('Ctrl Pts',(20.2651358983066,-4.18197237106197,-28.3208663256634));
#36465=CARTESIAN_POINT('Ctrl Pts',(16.3601222932309,-4.11421750462538,-26.3444433325659));
#36466=CARTESIAN_POINT('Ctrl Pts',(12.7886013364524,-4.08262421860679,-23.7588994143533));
#36467=CARTESIAN_POINT('Ctrl Pts',(9.99908233100923,-4.0828488851085,-21.1364173862108));
#36468=CARTESIAN_POINT('Ctrl Pts',(8.34928571759199,-4.10207414795096,-19.1247770659859));
#36469=CARTESIAN_POINT('Ctrl Pts',(7.34240870565719,-4.12088738197538,-17.7173046985667));
#36470=CARTESIAN_POINT('Ctrl Pts',(7.10876813411939,-4.12583098108427,-17.3760304556457));
#36471=CARTESIAN_POINT('Ctrl Pts',(6.88306649246102,-4.13120272145022,-17.0314308181555));
#36472=CARTESIAN_POINT('',(46.8671786463539,20.7105311502984,0.856680668514059));
#36473=CARTESIAN_POINT('Ctrl Pts',(46.8671786463539,20.7105311502984,0.85668066851405));
#36474=CARTESIAN_POINT('Ctrl Pts',(42.9014764671361,20.5483438544848,-2.48144010722812));
#36475=CARTESIAN_POINT('Ctrl Pts',(38.2828465564874,20.4520245495079,-5.02872828673426));
#36476=CARTESIAN_POINT('Ctrl Pts',(28.4491423215176,20.3052748660675,-8.30400152038972));
#36477=CARTESIAN_POINT('Ctrl Pts',(23.2335530202462,20.248474007324,-9.03506651020502));
#36478=CARTESIAN_POINT('Ctrl Pts',(18.0621112303383,20.1925493450898,-8.74422771304759));
#36479=CARTESIAN_POINT('',(36.2576798233721,-3.27137091447503,-29.7093686459786));
#36480=CARTESIAN_POINT('Ctrl Pts',(46.8671786463482,20.7105311502992,0.856680668513758));
#36481=CARTESIAN_POINT('Ctrl Pts',(46.9249887269589,19.9641948262067,-2.30600051616087));
#36482=CARTESIAN_POINT('Ctrl Pts',(46.6560935232336,18.7336174322536,-5.37662766955232));
#36483=CARTESIAN_POINT('Ctrl Pts',(45.5710956442331,15.6437709263415,-11.4562521714677));
#36484=CARTESIAN_POINT('Ctrl Pts',(44.6678816065033,13.6706054953476,-14.5214537476068));
#36485=CARTESIAN_POINT('Ctrl Pts',(42.5169745662042,9.45712578015162,-19.9441390711336));
#36486=CARTESIAN_POINT('Ctrl Pts',(41.2615426847051,7.18268855808127,-22.3812734554399));
#36487=CARTESIAN_POINT('Ctrl Pts',(38.6998696152663,2.26699026933656,-26.5599268565702));
#36488=CARTESIAN_POINT('Ctrl Pts',(37.3979964354348,-0.36522399219511,-28.317712640974));
#36489=CARTESIAN_POINT('Ctrl Pts',(36.2576793998219,-3.27137053313468,-29.709369095263));
#36490=CARTESIAN_POINT('Ctrl Pts',(36.2576797497044,-3.2713710013512,-29.7093681727007));
#36491=CARTESIAN_POINT('Ctrl Pts',(35.4899009191443,-3.25992112204952,-29.8267742981394));
#36492=CARTESIAN_POINT('Ctrl Pts',(34.7207207197571,-3.24789096533568,-29.9144772584936));
#36493=CARTESIAN_POINT('Ctrl Pts',(33.9517915369502,-3.23555894384663,-29.9728534820301));
#36494=CARTESIAN_POINT('Ctrl Pts',(32.0686564302618,-3.2053573815679,-30.1158189441238));
#36495=CARTESIAN_POINT('Ctrl Pts',(30.1870269834765,-3.17334534347451,-30.0828890834105));
#36496=CARTESIAN_POINT('Ctrl Pts',(28.3311759587029,-3.14345008158505,-29.8797419860564));
#36497=CARTESIAN_POINT('Ctrl Pts',(27.0939418794257,-3.12351990598108,-29.7443105809502));
#36498=CARTESIAN_POINT('Ctrl Pts',(25.8681648777386,-3.10453051989494,-29.5332270629972));
#36499=CARTESIAN_POINT('Ctrl Pts',(24.6610277249437,-3.08752071373525,-29.2482168634081));
#36500=CARTESIAN_POINT('Ctrl Pts',(23.4538905727806,-3.07051090758448,-28.9632066639682));
#36501=CARTESIAN_POINT('Ctrl Pts',(22.2653932694828,-3.0554806813514,-28.6042697829724));
#36502=CARTESIAN_POINT('Ctrl Pts',(21.1027127831863,-3.04339100491456,-28.1731487078922));
#36503=CARTESIAN_POINT('Ctrl Pts',(19.358692055909,-3.02525649028182,-27.5264670960756));
#36504=CARTESIAN_POINT('Ctrl Pts',(17.6727591667208,-3.01373821257335,-26.7173710480374));
#36505=CARTESIAN_POINT('Ctrl Pts',(16.0690765496337,-3.01128625574909,-25.7518436565054));
#36506=CARTESIAN_POINT('Ctrl Pts',(14.9999548074193,-3.00965161787008,-25.1081587303288));
#36507=CARTESIAN_POINT('Ctrl Pts',(13.9673887414643,-3.01204645592803,-24.3949487628904));
#36508=CARTESIAN_POINT('Ctrl Pts',(12.9785164402689,-3.01891855380822,-23.6140047827048));
#36509=CARTESIAN_POINT('Ctrl Pts',(11.9896442576446,-3.02579065086441,-22.8330608961585));
#36510=CARTESIAN_POINT('Ctrl Pts',(11.0444658292623,-3.03714000665748,-21.9843830131019));
#36511=CARTESIAN_POINT('Ctrl Pts',(10.1501043009641,-3.05321938564873,-21.069763289763));
#36512=CARTESIAN_POINT('Ctrl Pts',(9.78156805938634,-3.05984515577954,-20.6928793288064));
#36513=CARTESIAN_POINT('Ctrl Pts',(9.42166046939857,-3.06727406915266,-20.3047985397277));
#36514=CARTESIAN_POINT('Ctrl Pts',(9.07087845564185,-3.07550335254719,-19.9056465116819));
#36515=CARTESIAN_POINT('Ctrl Pts',(45.973362676981,-4.68328060676847,-27.2756663271766));
#36516=CARTESIAN_POINT('Ctrl Pts',(45.6126991612577,-4.67927906663786,-27.4604236536159));
#36517=CARTESIAN_POINT('Ctrl Pts',(45.2471033099969,-4.67486342687383,-27.6388296622253));
#36518=CARTESIAN_POINT('Ctrl Pts',(43.6710473719894,-4.65418501649615,-28.3700492381431));
#36519=CARTESIAN_POINT('Ctrl Pts',(41.2202507588911,-4.61395560865182,-29.3209731200025));
#36520=CARTESIAN_POINT('Ctrl Pts',(37.4689495057187,-4.53496565777432,-30.2540302896408));
#36521=CARTESIAN_POINT('Ctrl Pts',(33.055595633981,-4.42959393838223,-30.7790187239315));
#36522=CARTESIAN_POINT('Ctrl Pts',(28.659697939306,-4.31850354734918,-30.6147326637025));
#36523=CARTESIAN_POINT('Ctrl Pts',(24.3764348754538,-4.2170896233612,-29.7845731359287));
#36524=CARTESIAN_POINT('Ctrl Pts',(20.2339666249731,-4.13063759391767,-28.4345208839583));
#36525=CARTESIAN_POINT('Ctrl Pts',(16.3307767357573,-4.07121155600733,-26.4507623239868));
#36526=CARTESIAN_POINT('Ctrl Pts',(12.7615353803547,-4.04803120464602,-23.8579397816895));
#36527=CARTESIAN_POINT('Ctrl Pts',(9.97429755410247,-4.055480889925,-21.2292769138081));
#36528=CARTESIAN_POINT('Ctrl Pts',(8.32624150720379,-4.07952578289679,-19.2135755950718));
#36529=CARTESIAN_POINT('Ctrl Pts',(7.31929162466779,-4.10152925776619,-17.801647007576));
#36530=CARTESIAN_POINT('Ctrl Pts',(7.08474911781699,-4.1072571624472,-17.4579084277431));
#36531=CARTESIAN_POINT('Ctrl Pts',(6.85824142480293,-4.11341014061892,-17.1108288866612));
#36532=CARTESIAN_POINT('Ctrl Pts',(46.0345375598687,-4.24009445412503,-26.9919991555953));
#36533=CARTESIAN_POINT('Ctrl Pts',(45.6750556727933,-4.23725223817857,-27.1786531095111));
#36534=CARTESIAN_POINT('Ctrl Pts',(45.3106133083243,-4.23400446880359,-27.3590016647185));
#36535=CARTESIAN_POINT('Ctrl Pts',(43.7393368113889,-4.21832863439708,-28.0986817692919));
#36536=CARTESIAN_POINT('Ctrl Pts',(41.2950934490877,-4.18572164472913,-29.0631532067729));
#36537=CARTESIAN_POINT('Ctrl Pts',(37.5512149138899,-4.11799618192084,-30.0181518488659));
#36538=CARTESIAN_POINT('Ctrl Pts',(33.1435649281886,-4.02550335874969,-30.5704030878674));
#36539=CARTESIAN_POINT('Ctrl Pts',(28.7494912840676,-3.92690475481451,-30.4351662245983));
#36540=CARTESIAN_POINT('Ctrl Pts',(24.4639098993022,-3.83755718932749,-29.6353920659615));
#36541=CARTESIAN_POINT('Ctrl Pts',(20.3156741014525,-3.76285616468038,-28.3165409874486));
#36542=CARTESIAN_POINT('Ctrl Pts',(16.4022501763199,-3.71481495977278,-26.3646862042512));
#36543=CARTESIAN_POINT('Ctrl Pts',(12.8180874502053,-3.70275434803773,-23.8039921794956));
#36544=CARTESIAN_POINT('Ctrl Pts',(10.014764308943,-3.71962751323487,-21.2027861208478));
#36545=CARTESIAN_POINT('Ctrl Pts',(8.35372688131093,-3.74992063397164,-19.2052003915485));
#36546=CARTESIAN_POINT('Ctrl Pts',(7.3374661001949,-3.77604797989279,-17.8050928273303));
#36547=CARTESIAN_POINT('Ctrl Pts',(7.10061080602625,-3.78276245762616,-17.464127862853));
#36548=CARTESIAN_POINT('Ctrl Pts',(6.87172363105669,-3.78989370687861,-17.1197471100359));
#36549=CARTESIAN_POINT('Ctrl Pts',(46.0970059190559,-3.80075287541765,-26.7026202149032));
#36550=CARTESIAN_POINT('Ctrl Pts',(45.7387037966384,-3.79905339336963,-26.8911923080337));
#36551=CARTESIAN_POINT('Ctrl Pts',(45.3754124664879,-3.79695621683146,-27.0735048418965));
#36552=CARTESIAN_POINT('Ctrl Pts',(43.8089024562329,-3.78620663871065,-27.8217362732406));
#36553=CARTESIAN_POINT('Ctrl Pts',(41.371192364366,-3.76109400159902,-28.7998819866087));
#36554=CARTESIAN_POINT('Ctrl Pts',(37.6347096129005,-3.70440674399875,-29.7769780940438));
#36555=CARTESIAN_POINT('Ctrl Pts',(33.2327383479775,-3.62448835210827,-30.3566365749797));
#36556=CARTESIAN_POINT('Ctrl Pts',(28.8404756925361,-3.53802316526296,-30.250552988433));
#36557=CARTESIAN_POINT('Ctrl Pts',(24.5525760323583,-3.46032715355504,-29.4812382422582));
#36558=CARTESIAN_POINT('Ctrl Pts',(20.3985825728977,-3.39690914788247,-28.1936488639279));
#36559=CARTESIAN_POINT('Ctrl Pts',(16.4749395169915,-3.35971861494906,-26.2737543336035));
#36560=CARTESIAN_POINT('Ctrl Pts',(12.8758609544234,-3.35817927654809,-23.7452608637003));
#36561=CARTESIAN_POINT('Ctrl Pts',(10.056435360143,-3.38391914529348,-21.1716020610987));
#36562=CARTESIAN_POINT('Ctrl Pts',(8.38238397495209,-3.42007079724739,-19.1922119346188));
#36563=CARTESIAN_POINT('Ctrl Pts',(7.35678013783898,-3.45006162272336,-17.8039874884584));
#36564=CARTESIAN_POINT('Ctrl Pts',(7.11760246326198,-3.45770043113048,-17.4658116774344));
#36565=CARTESIAN_POINT('Ctrl Pts',(6.8863244697825,-3.46574819271174,-17.1241457257504));
#36566=CARTESIAN_POINT('Ctrl Pts',(46.3218499125173,-2.2653457359543,-25.6621009480906));
#36567=CARTESIAN_POINT('Ctrl Pts',(45.9676956475964,-2.26761569662348,-25.8575133309122));
#36568=CARTESIAN_POINT('Ctrl Pts',(45.6084503547893,-2.26951335386862,-26.0468269264624));
#36569=CARTESIAN_POINT('Ctrl Pts',(44.0586916831692,-2.27586002752392,-26.8255305361844));
#36570=CARTESIAN_POINT('Ctrl Pts',(41.6439336730249,-2.27671432942662,-27.8523380738304));
#36571=CARTESIAN_POINT('Ctrl Pts',(37.9334156521198,-2.25814179129592,-28.9078977789232));
#36572=CARTESIAN_POINT('Ctrl Pts',(33.5513614110281,-2.2214798205824,-29.5846993393589));
#36573=CARTESIAN_POINT('Ctrl Pts',(29.1654252452448,-2.17652897108851,-29.5817711347714));
#36574=CARTESIAN_POINT('Ctrl Pts',(24.8693434695226,-2.13845241575724,-28.9201093573139));
#36575=CARTESIAN_POINT('Ctrl Pts',(20.6950799083771,-2.11316923258448,-27.7429517662975));
#36576=CARTESIAN_POINT('Ctrl Pts',(16.7354600708946,-2.11235831802136,-25.9359348634863));
#36577=CARTESIAN_POINT('Ctrl Pts',(13.0838196040227,-2.14581153060268,-23.5212178093802));
#36578=CARTESIAN_POINT('Ctrl Pts',(10.2075738210828,-2.20085463389179,-21.0449921098509));
#36579=CARTESIAN_POINT('Ctrl Pts',(8.48753717971688,-2.25628908058851,-19.1300289525424));
#36580=CARTESIAN_POINT('Ctrl Pts',(7.42888933073493,-2.29898278275007,-17.7839145087321));
#36581=CARTESIAN_POINT('Ctrl Pts',(7.18149013898659,-2.30966173471912,-17.4556298037868));
#36582=CARTESIAN_POINT('Ctrl Pts',(6.94174097526185,-2.32072459453129,-17.1235981440825));
#36583=CARTESIAN_POINT('Ctrl Pts',(46.7450706088707,0.42091842584111,-23.7082581849838));
#36584=CARTESIAN_POINT('Ctrl Pts',(46.3983038112075,0.412015546281074,-23.9161367305282));
#36585=CARTESIAN_POINT('Ctrl Pts',(46.0462690198602,0.403442573942463,-24.1182027052624));
#36586=CARTESIAN_POINT('Ctrl Pts',(44.5263831245904,0.368526239150617,-24.9523849210783));
#36587=CARTESIAN_POINT('Ctrl Pts',(42.1525358259181,0.324281374370589,-26.0676939450635));
#36588=CARTESIAN_POINT('Ctrl Pts',(38.4882271453103,0.279215865745994,-27.2657018770151));
#36589=CARTESIAN_POINT('Ctrl Pts',(34.1415021026478,0.243759038204317,-28.1186055579968));
#36590=CARTESIAN_POINT('Ctrl Pts',(29.7665531301524,0.21967725703067,-28.3023951485284));
#36591=CARTESIAN_POINT('Ctrl Pts',(25.4554695335823,0.192114722189047,-27.8353545953069));
#36592=CARTESIAN_POINT('Ctrl Pts',(21.2445496907064,0.154437491851918,-26.8576751479132));
#36593=CARTESIAN_POINT('Ctrl Pts',(17.2201347615873,0.0954817696064694,
-25.2543692928801));
#36594=CARTESIAN_POINT('Ctrl Pts',(13.4739839232542,0.0048363712043943,
-23.0448309980406));
#36595=CARTESIAN_POINT('Ctrl Pts',(10.4956451040933,-0.0979118428630517,
-20.7442185796579));
#36596=CARTESIAN_POINT('Ctrl Pts',(8.6930230569115,-0.184631554593919,-18.945324770953));
#36597=CARTESIAN_POINT('Ctrl Pts',(7.57504200713313,-0.247909792323189,
-17.6750591709347));
#36598=CARTESIAN_POINT('Ctrl Pts',(7.31286586886589,-0.263520166061751,
-17.3646161592107));
#36599=CARTESIAN_POINT('Ctrl Pts',(7.05787648054576,-0.279478515480188,
-17.0499880689702));
#36600=CARTESIAN_POINT('Ctrl Pts',(47.404986111522,3.93922736422659,-20.6755997409199));
#36601=CARTESIAN_POINT('Ctrl Pts',(47.0684640420326,3.92273017306588,-20.9015567403437));
#36602=CARTESIAN_POINT('Ctrl Pts',(46.7264339108031,3.90651491483579,-21.122098655959));
#36603=CARTESIAN_POINT('Ctrl Pts',(45.2480229962362,3.83888692720806,-22.0365898282304));
#36604=CARTESIAN_POINT('Ctrl Pts',(42.9309251724468,3.74496038387833,-23.27972878241));
#36605=CARTESIAN_POINT('Ctrl Pts',(39.3305341019574,3.6271896762232,-24.6827159172831));
#36606=CARTESIAN_POINT('Ctrl Pts',(35.0323762557642,3.50969140214063,-25.7882334176081));
#36607=CARTESIAN_POINT('Ctrl Pts',(30.6719240550635,3.40771510315772,-26.2389829367879));
#36608=CARTESIAN_POINT('Ctrl Pts',(26.3389517794478,3.30695483103527,-26.0494460750817));
#36609=CARTESIAN_POINT('Ctrl Pts',(22.075820938881,3.1998573133211,-25.3556539412325));
#36610=CARTESIAN_POINT('Ctrl Pts',(17.9597861203445,3.07607789704229,-24.0416439011457));
#36611=CARTESIAN_POINT('Ctrl Pts',(14.0803885674248,2.92448144596071,-22.1229486412386));
#36612=CARTESIAN_POINT('Ctrl Pts',(10.9582980306177,2.77158317941627,-20.0709337271445));
#36613=CARTESIAN_POINT('Ctrl Pts',(9.03949054530486,2.65236568914073,-18.4361422761851));
#36614=CARTESIAN_POINT('Ctrl Pts',(7.83806324235876,2.56779645721963,-17.2730525922546));
#36615=CARTESIAN_POINT('Ctrl Pts',(7.55508253700517,2.54707902977605,-16.9878808614455));
#36616=CARTESIAN_POINT('Ctrl Pts',(7.27861346550577,2.52604544176493,-16.6979630171119));
#36617=CARTESIAN_POINT('Ctrl Pts',(48.2293875139225,7.64857049485316,-16.8981516990451));
#36618=CARTESIAN_POINT('Ctrl Pts',(47.9044854606453,7.62538079009264,-17.1453036599416));
#36619=CARTESIAN_POINT('Ctrl Pts',(47.5738209702538,7.6024320797305,-17.387480874535));
#36620=CARTESIAN_POINT('Ctrl Pts',(46.142612130283,7.50598047950645,-18.3959113196943));
#36621=CARTESIAN_POINT('Ctrl Pts',(43.8900756880785,7.36825978906471,-19.7883331202706));
#36622=CARTESIAN_POINT('Ctrl Pts',(40.3623101677245,7.18657585481396,-21.4300219986148));
#36623=CARTESIAN_POINT('Ctrl Pts',(36.1191823553037,6.99739878870591,-22.8289978138919));
#36624=CARTESIAN_POINT('Ctrl Pts',(31.7748392253983,6.82819742189185,-23.5890542762665));
#36625=CARTESIAN_POINT('Ctrl Pts',(27.4163985899668,6.66543158101024,-23.7203074035036));
#36626=CARTESIAN_POINT('Ctrl Pts',(23.0931437411946,6.50060855796851,-23.3541400227856));
#36627=CARTESIAN_POINT('Ctrl Pts',(18.871936060649,6.32441606849526,-22.3733522608672));
#36628=CARTESIAN_POINT('Ctrl Pts',(14.8397692169601,6.12505774886043,-20.789058032324));
#36629=CARTESIAN_POINT('Ctrl Pts',(11.5529516632508,5.93384517916791,-19.022472123698));
#36630=CARTESIAN_POINT('Ctrl Pts',(9.50104963584418,5.79035915091665,-17.5758361408519));
#36631=CARTESIAN_POINT('Ctrl Pts',(8.2040429508047,5.69001969995687,-16.53554757429));
#36632=CARTESIAN_POINT('Ctrl Pts',(7.89722279090849,5.66551509710643,-16.2794272231178));
#36633=CARTESIAN_POINT('Ctrl Pts',(7.59612832462127,5.64071489355821,-16.0180105688444));
#36634=CARTESIAN_POINT('Ctrl Pts',(49.0074290450359,10.6050661536892,-13.3398928188639));
#36635=CARTESIAN_POINT('Ctrl Pts',(48.6926428289153,10.5777689837161,-13.6059506753262));
#36636=CARTESIAN_POINT('Ctrl Pts',(48.3718894359035,10.5506896266998,-13.867401871622));
#36637=CARTESIAN_POINT('Ctrl Pts',(46.9819221114144,10.4365567481294,-14.9594187343244));
#36638=CARTESIAN_POINT('Ctrl Pts',(44.785792189829,10.2719415070743,-16.4845031570036));
#36639=CARTESIAN_POINT('Ctrl Pts',(41.3214668828266,10.0511774947007,-18.3378392475286));
#36640=CARTESIAN_POINT('Ctrl Pts',(37.1263846220837,9.81863871620139,-19.9964958281689));
#36641=CARTESIAN_POINT('Ctrl Pts',(32.7960498298375,9.60967367489776,-21.0296519428195));
#36642=CARTESIAN_POINT('Ctrl Pts',(28.4152465042761,9.41153176383594,-21.4435784231541));
#36643=CARTESIAN_POINT('Ctrl Pts',(24.0393070860599,9.21500541081661,-21.3656747993208));
#36644=CARTESIAN_POINT('Ctrl Pts',(19.7259921649729,9.01175979868378,-20.6775485689242));
#36645=CARTESIAN_POINT('Ctrl Pts',(15.5600549717428,8.78956564702969,-19.3864322787829));
#36646=CARTESIAN_POINT('Ctrl Pts',(12.1290015717314,8.58124477590158,-17.8697330625877));
#36647=CARTESIAN_POINT('Ctrl Pts',(9.96056099183191,8.42762540105217,-16.5875825895315));
#36648=CARTESIAN_POINT('Ctrl Pts',(8.57986327584419,8.32086564673385,-15.6545659656521));
#36649=CARTESIAN_POINT('Ctrl Pts',(8.25218357257416,8.29482075310626,-15.4239074282687));
#36650=CARTESIAN_POINT('Ctrl Pts',(7.9295530816775,8.26849188852043,-15.1875542054435));
#36651=CARTESIAN_POINT('Ctrl Pts',(49.9530904856153,13.6252616883324,-9.01825571656003));
#36652=CARTESIAN_POINT('Ctrl Pts',(49.6498521530964,13.5952855444977,-9.30614285476429));
#36653=CARTESIAN_POINT('Ctrl Pts',(49.3404326906899,13.5655149131873,-9.58981807772683));
#36654=CARTESIAN_POINT('Ctrl Pts',(47.9977231570628,13.4398628522405,-10.7780905257659));
#36655=CARTESIAN_POINT('Ctrl Pts',(45.8662585664357,13.2576618204372,-12.4558237781188));
#36656=CARTESIAN_POINT('Ctrl Pts',(42.474764561552,13.0115743729063,-14.5523271530002));
#36657=CARTESIAN_POINT('Ctrl Pts',(38.3350016346459,12.751644575675,-16.5089212299443));
#36658=CARTESIAN_POINT('Ctrl Pts',(34.0211144068637,12.5189796899122,-17.8548947174334));
#36659=CARTESIAN_POINT('Ctrl Pts',(29.615209004902,12.301865256328,-18.5920822373384));
#36660=CARTESIAN_POINT('Ctrl Pts',(25.1795213846675,12.0904144587841,-18.8434107242654));
#36661=CARTESIAN_POINT('Ctrl Pts',(20.7614048765242,11.8774764455751,-18.4889962355741));
#36662=CARTESIAN_POINT('Ctrl Pts',(16.4430392282013,11.6504923923572,-17.5316024294851));
#36663=CARTESIAN_POINT('Ctrl Pts',(12.8475180499629,11.4410171343385,-16.2989298354701));
#36664=CARTESIAN_POINT('Ctrl Pts',(10.5461259110488,11.2882220371981,-15.2034411599271));
#36665=CARTESIAN_POINT('Ctrl Pts',(9.06993062890748,11.1823584691134,-14.3920548118685));
#36666=CARTESIAN_POINT('Ctrl Pts',(8.71849421176945,11.1565388193505,-14.1903535125101));
#36667=CARTESIAN_POINT('Ctrl Pts',(8.37137676108469,11.1304479812224,-13.982592023269));
#36668=CARTESIAN_POINT('Ctrl Pts',(50.8248043471025,15.9398275064074,-5.03469583101935));
#36669=CARTESIAN_POINT('Ctrl Pts',(50.531689720598,15.9092719019138,-5.34176956106061));
#36670=CARTESIAN_POINT('Ctrl Pts',(50.2322216993377,15.8789225535602,-5.64495084018071));
#36671=CARTESIAN_POINT('Ctrl Pts',(48.9310805715447,15.7507918597713,-6.91759254606773));
#36672=CARTESIAN_POINT('Ctrl Pts',(46.856540968822,15.5646999212503,-8.72905784910073));
#36673=CARTESIAN_POINT('Ctrl Pts',(43.5293146351041,15.3133344724918,-11.0383768254307));
#36674=CARTESIAN_POINT('Ctrl Pts',(39.4386131135355,15.0487502016962,-13.2554538905063));
#36675=CARTESIAN_POINT('Ctrl Pts',(35.1398025651756,14.8142492774957,-14.8745682218989));
#36676=CARTESIAN_POINT('Ctrl Pts',(30.7126367899701,14.5991383033468,-15.8936292613155));
#36677=CARTESIAN_POINT('Ctrl Pts',(26.225383041263,14.3930646018661,-16.4317101448757));
#36678=CARTESIAN_POINT('Ctrl Pts',(21.7162835651667,14.1899609567462,-16.3675092373584));
#36679=CARTESIAN_POINT('Ctrl Pts',(17.26525500769,13.977122935371,-15.6998422171581));
#36680=CARTESIAN_POINT('Ctrl Pts',(13.5264251178423,13.7824369346935,-14.713381358643));
#36681=CARTESIAN_POINT('Ctrl Pts',(11.1090908355661,13.6409944051188,-13.7794319835509));
#36682=CARTESIAN_POINT('Ctrl Pts',(9.54958799636594,13.5429643472183,-13.0732079429502));
#36683=CARTESIAN_POINT('Ctrl Pts',(9.17748643978684,13.5190447294408,-12.8966048355516));
#36684=CARTESIAN_POINT('Ctrl Pts',(8.80912250506288,13.4948677704672,-12.7136870295246));
#36685=CARTESIAN_POINT('Ctrl Pts',(51.8622440502334,18.188947172369,-0.289545832901423));
#36686=CARTESIAN_POINT('Ctrl Pts',(51.5807701807973,18.1597316481657,-0.618456087500125));
#36687=CARTESIAN_POINT('Ctrl Pts',(51.2927600533601,18.1307342364494,-0.943805954907987));
#36688=CARTESIAN_POINT('Ctrl Pts',(50.0395554717762,18.0083786966032,-2.31220075101254));
#36689=CARTESIAN_POINT('Ctrl Pts',(48.0307425794066,17.830846834045,-4.27543281823846));
#36690=CARTESIAN_POINT('Ctrl Pts',(44.778002741115,17.5925027676131,-6.82619040609315));
#36691=CARTESIAN_POINT('Ctrl Pts',(40.7446169869983,17.3443426911773,-9.33864581572932));
#36692=CARTESIAN_POINT('Ctrl Pts',(36.4643204356845,17.1289494695207,-11.2672600886416));
#36693=CARTESIAN_POINT('Ctrl Pts',(32.0141683740696,16.9369213116231,-12.6053959862687));
#36694=CARTESIAN_POINT('Ctrl Pts',(27.4693092848983,16.7575317657622,-13.4677724902511));
#36695=CARTESIAN_POINT('Ctrl Pts',(22.8575688046928,16.5859876106103,-13.7313406272161));
#36696=CARTESIAN_POINT('Ctrl Pts',(18.2562644932297,16.4095763329362,-13.3903470280312));
#36697=CARTESIAN_POINT('Ctrl Pts',(14.3547946342421,16.2491906636996,-12.6810668013076));
#36698=CARTESIAN_POINT('Ctrl Pts',(11.8057078793454,16.1323920433636,-11.9286495487117));
#36699=CARTESIAN_POINT('Ctrl Pts',(10.1514883569898,16.0510402241362,-11.3404810809659));
#36700=CARTESIAN_POINT('Ctrl Pts',(9.75597558972479,16.0311583490605,-11.1921012097805));
#36701=CARTESIAN_POINT('Ctrl Pts',(9.36361992511381,16.01103806515,-11.0371697661498));
#36702=CARTESIAN_POINT('Ctrl Pts',(52.8005712434362,19.7983627848149,4.00856019691356));
#36703=CARTESIAN_POINT('Ctrl Pts',(52.5293769678043,19.7720645135703,3.66073478500352));
#36704=CARTESIAN_POINT('Ctrl Pts',(52.2514949487339,19.7460021313493,3.31620884467359));
#36705=CARTESIAN_POINT('Ctrl Pts',(51.0407143360908,19.6361820466171,1.86509964359795));
#36706=CARTESIAN_POINT('Ctrl Pts',(49.0901569813625,19.4774394485581,-0.229263744330297));
#36707=CARTESIAN_POINT('Ctrl Pts',(45.9037408638273,19.2670183310104,-2.98866537396808));
#36708=CARTESIAN_POINT('Ctrl Pts',(41.9218786695201,19.0520629838802,-5.75635326875137));
#36709=CARTESIAN_POINT('Ctrl Pts',(37.6591904462393,18.8717166252608,-7.95229818907755));
#36710=CARTESIAN_POINT('Ctrl Pts',(33.1903616902194,18.7178122962125,-9.5658253198722));
#36711=CARTESIAN_POINT('Ctrl Pts',(28.5965511857935,18.5794411422907,-10.707876735862));
#36712=CARTESIAN_POINT('Ctrl Pts',(23.8964674609503,18.4529446490623,-11.2537653259037));
#36713=CARTESIAN_POINT('Ctrl Pts',(19.1651429878408,18.3257380682571,-11.1936823159398));
#36714=CARTESIAN_POINT('Ctrl Pts',(15.1226214079936,18.2102139945187,-10.7223744229274));
#36715=CARTESIAN_POINT('Ctrl Pts',(12.4590849026629,18.1249152482566,-10.125515214314));
#36716=CARTESIAN_POINT('Ctrl Pts',(10.7225346207661,18.064727637235,-9.63839747515494));
#36717=CARTESIAN_POINT('Ctrl Pts',(10.3067513445607,18.0499634327475,-9.51419720566911));
#36718=CARTESIAN_POINT('Ctrl Pts',(9.89369712912435,18.0349776243875,-9.38326573097788));
#36719=CARTESIAN_POINT('Ctrl Pts',(53.4863370250255,20.6836496418694,7.15694860497204));
#36720=CARTESIAN_POINT('Ctrl Pts',(53.2225809627893,20.6606519170286,6.79587106594126));
#36721=CARTESIAN_POINT('Ctrl Pts',(52.952032742616,20.6379063239872,6.43792468941075));
#36722=CARTESIAN_POINT('Ctrl Pts',(51.7719980977726,20.5422448076096,4.92898918929371));
#36723=CARTESIAN_POINT('Ctrl Pts',(49.8637381959815,20.4047755971079,2.74288789221826));
#36724=CARTESIAN_POINT('Ctrl Pts',(46.7257495251636,20.225761668211,-0.162608626170642));
#36725=CARTESIAN_POINT('Ctrl Pts',(42.7819444547883,20.0475517349526,-3.10909821565097));
#36726=CARTESIAN_POINT('Ctrl Pts',(38.5331171200345,19.9048724048602,-5.49235143170712));
#36727=CARTESIAN_POINT('Ctrl Pts',(34.0522545486923,19.790507905872,-7.29876156315941));
#36728=CARTESIAN_POINT('Ctrl Pts',(29.4248004114224,19.6935273080542,-8.63658437963781));
#36729=CARTESIAN_POINT('Ctrl Pts',(24.6629501157001,19.6110850660289,-9.37988832701164));
#36730=CARTESIAN_POINT('Ctrl Pts',(19.8400964602983,19.530779076001,-9.51591962186098));
#36731=CARTESIAN_POINT('Ctrl Pts',(15.697975272498,19.4573327991495,-9.21047942885606));
#36732=CARTESIAN_POINT('Ctrl Pts',(12.9534550617257,19.4012238336331,-8.72182627864199));
#36733=CARTESIAN_POINT('Ctrl Pts',(11.1586004449949,19.3605693891818,-8.30491329803392));
#36734=CARTESIAN_POINT('Ctrl Pts',(10.7285107947356,19.3505226070412,-8.19751403024314));
#36735=CARTESIAN_POINT('Ctrl Pts',(10.3008944253755,19.3402634731691,-8.08326215051905));
#36736=CARTESIAN_POINT('Ctrl Pts',(53.8717271214901,21.117312799858,8.92829900095583));
#36737=CARTESIAN_POINT('Ctrl Pts',(53.6121489835061,21.0964267127388,8.55989544261294));
#36738=CARTESIAN_POINT('Ctrl Pts',(53.3457209337029,21.0758020890032,8.19453489651512));
#36739=CARTESIAN_POINT('Ctrl Pts',(52.1829645833057,20.9891913310095,6.6536739220593));
#36740=CARTESIAN_POINT('Ctrl Pts',(50.2984941161407,20.8653273744228,4.41690405101842));
#36741=CARTESIAN_POINT('Ctrl Pts',(47.1878108923031,20.7063681300896,1.43067040790121));
#36742=CARTESIAN_POINT('Ctrl Pts',(43.2655731566299,20.5515335415639,-1.6146666396427));
#36743=CARTESIAN_POINT('Ctrl Pts',(39.0248124328953,20.4326519806542,-4.10149377374684));
#36744=CARTESIAN_POINT('Ctrl Pts',(34.5375663594191,20.3430531321453,-6.01455607201149));
#36745=CARTESIAN_POINT('Ctrl Pts',(29.8916687633621,20.2718184169426,-7.46061039168494));
#36746=CARTESIAN_POINT('Ctrl Pts',(25.095679036358,20.2165549432469,-8.31301457851303));
#36747=CARTESIAN_POINT('Ctrl Pts',(20.222073018947,20.164982094833,-8.55735906158925));
#36748=CARTESIAN_POINT('Ctrl Pts',(16.0246456841948,20.117197691553,-8.34346646267442));
#36749=CARTESIAN_POINT('Ctrl Pts',(13.2351131391784,20.0788282397779,-7.91448534989634));
#36750=CARTESIAN_POINT('Ctrl Pts',(11.4078395864424,20.0500302875854,-7.53626778012411));
#36751=CARTESIAN_POINT('Ctrl Pts',(10.9698103207056,20.0428451797642,-7.43812761261326));
#36752=CARTESIAN_POINT('Ctrl Pts',(10.5341268922228,20.0354515632684,-7.33306706741316));
#36753=CARTESIAN_POINT('Ctrl Pts',(53.9812860025028,21.2334813897109,9.43208375200366));
#36754=CARTESIAN_POINT('Ctrl Pts',(53.722894343233,21.2132228077857,9.06160546170904));
#36755=CARTESIAN_POINT('Ctrl Pts',(53.457636234034,21.1932283095702,8.69414579528152));
#36756=CARTESIAN_POINT('Ctrl Pts',(52.2997857115371,21.1093059289188,7.14424851817797));
#36757=CARTESIAN_POINT('Ctrl Pts',(50.4220705832473,20.9894835119608,4.89313906637515));
#36758=CARTESIAN_POINT('Ctrl Pts',(47.3191460135461,20.8364792943525,1.88406529232576));
#36759=CARTESIAN_POINT('Ctrl Pts',(43.4030459066543,20.6885792302246,-1.18922048567419));
#36760=CARTESIAN_POINT('Ctrl Pts',(39.1646030660498,20.5767478260626,-3.70530894006767));
#36761=CARTESIAN_POINT('Ctrl Pts',(34.675589875711,20.4944756050622,-5.64847247317747));
#36762=CARTESIAN_POINT('Ctrl Pts',(30.0245195766032,20.4308554028779,-7.12504250766887));
#36763=CARTESIAN_POINT('Ctrl Pts',(25.2189244368836,20.3836340081555,-8.00816612769719));
#36764=CARTESIAN_POINT('Ctrl Pts',(20.3310177005882,20.340580727313,-8.28296238675351));
#36765=CARTESIAN_POINT('Ctrl Pts',(16.1179909263383,20.3004356869138,-8.09477141097565));
#36766=CARTESIAN_POINT('Ctrl Pts',(13.3157463284093,20.2673681898868,-7.682522571651));
#36767=CARTESIAN_POINT('Ctrl Pts',(11.4793096661362,20.2421246596599,-7.31514879108788));
#36768=CARTESIAN_POINT('Ctrl Pts',(11.0390389775994,20.2357981340653,-7.21960298661229));
#36769=CARTESIAN_POINT('Ctrl Pts',(10.6010806842436,20.2292648564311,-7.11711746623022));
#36770=CARTESIAN_POINT('Ctrl Pts',(54.0911200992672,21.3428689572265,9.93733722545763));
#36771=CARTESIAN_POINT('Ctrl Pts',(53.8339160771895,21.323266505305,9.56478777996708));
#36772=CARTESIAN_POINT('Ctrl Pts',(53.5698289525631,21.303930781031,9.1952328547344));
#36773=CARTESIAN_POINT('Ctrl Pts',(52.4168883164214,21.2228186866547,7.63631699932278));
#36774=CARTESIAN_POINT('Ctrl Pts',(50.5459347798675,21.1072213437662,5.37089768690188));
#36775=CARTESIAN_POINT('Ctrl Pts',(47.4507803460891,20.9604400919523,2.33903941389612));
#36776=CARTESIAN_POINT('Ctrl Pts',(43.5408353390201,20.819779963638,-0.762113079351122));
#36777=CARTESIAN_POINT('Ctrl Pts',(39.3047370968672,20.7152993064879,-3.30735423302198));
#36778=CARTESIAN_POINT('Ctrl Pts',(34.8139967414564,20.6406553883908,-5.28047852159549));
#36779=CARTESIAN_POINT('Ctrl Pts',(30.1578084903746,20.5849601975755,-6.78739123617449));
#36780=CARTESIAN_POINT('Ctrl Pts',(25.342681856911,20.5461109852346,-7.70101963370857));
#36781=CARTESIAN_POINT('Ctrl Pts',(20.4405655462474,20.5119420676311,-8.00600926239656));
#36782=CARTESIAN_POINT('Ctrl Pts',(16.212024900435,20.4797911688045,-7.84326492086165));
#36783=CARTESIAN_POINT('Ctrl Pts',(13.3971231763776,20.4522911786996,-7.44756158079435));
#36784=CARTESIAN_POINT('Ctrl Pts',(11.5515559411525,20.4307901345004,-7.09090367684731));
#36785=CARTESIAN_POINT('Ctrl Pts',(11.1090536044908,20.4253683033402,-6.99792131334964));
#36786=CARTESIAN_POINT('Ctrl Pts',(10.6688320741027,20.4197421663948,-6.89797979485316));
#36787=CARTESIAN_POINT('',(46.8667964697728,20.5529756002067,0.877339649208841));
#36788=CARTESIAN_POINT('Ctrl Pts',(36.2576800729436,-3.27137127985418,-29.7093682737774));
#36789=CARTESIAN_POINT('Ctrl Pts',(38.8712563024324,1.76302065360657,-26.519728653349));
#36790=CARTESIAN_POINT('Ctrl Pts',(41.7528145455644,6.26298702224536,-22.1049479564332));
#36791=CARTESIAN_POINT('Ctrl Pts',(44.8544505987311,12.5188402724798,-13.9136701764686));
#36792=CARTESIAN_POINT('Ctrl Pts',(45.663807377154,14.4577038717083,-11.0195527891233));
#36793=CARTESIAN_POINT('Ctrl Pts',(46.6763124148208,17.8486374263941,-5.17928678953648));
#36794=CARTESIAN_POINT('Ctrl Pts',(46.9241791761197,19.3555632898772,-2.18801330074644));
#36795=CARTESIAN_POINT('Ctrl Pts',(46.8667964697728,20.5529756002057,0.877339649209231));
#36796=CARTESIAN_POINT('Ctrl Pts',(18.6922256707601,19.9464420456703,-8.75371524283479));
#36797=CARTESIAN_POINT('Ctrl Pts',(23.7687459556886,20.0189549105364,-8.95811201716394));
#36798=CARTESIAN_POINT('Ctrl Pts',(28.8732165143738,20.0954766247834,-8.18217898492732));
#36799=CARTESIAN_POINT('Ctrl Pts',(38.4807809072633,20.2752040736289,-4.89538748035974));
#36800=CARTESIAN_POINT('Ctrl Pts',(42.9847320388888,20.3824974081049,-2.38626645795844));
#36801=CARTESIAN_POINT('Ctrl Pts',(46.8667964697727,20.5529756002056,0.877339649208949));
#36802=CARTESIAN_POINT('Ctrl Pts',(53.2371989972853,20.9435908393615,7.71126064895046));
#36803=CARTESIAN_POINT('Ctrl Pts',(53.1446919057712,20.9358615047579,7.58646941752768));
#36804=CARTESIAN_POINT('Ctrl Pts',(53.0521848142571,20.9281321701544,7.4616781861049));
#36805=CARTESIAN_POINT('Ctrl Pts',(52.959677722743,20.9204028355509,7.33688695468212));
#36806=CARTESIAN_POINT('Ctrl Pts',(43.7089685713345,20.1474693751975,-5.14223618759627));
#36807=CARTESIAN_POINT('Ctrl Pts',(26.9145688537952,20.0812550388979,-11.2680756118925));
#36808=CARTESIAN_POINT('Ctrl Pts',(11.77453820435,19.8399463130827,-7.84596586922967));
#36809=CARTESIAN_POINT('Ctrl Pts',(53.2371847394383,20.9469886892296,7.71116661896362));
#36810=CARTESIAN_POINT('Ctrl Pts',(53.1446826144396,20.9392720585054,7.58636902784782));
#36811=CARTESIAN_POINT('Ctrl Pts',(53.0521804894409,20.9315554277811,7.46157143673202));
#36812=CARTESIAN_POINT('Ctrl Pts',(52.9596783644423,20.9238387970569,7.33677384561622));
#36813=CARTESIAN_POINT('Ctrl Pts',(43.7094658645762,20.1521757246323,-5.14298526596396));
#36814=CARTESIAN_POINT('Ctrl Pts',(26.9147671963741,20.0873688943554,-11.2684775349938));
#36815=CARTESIAN_POINT('Ctrl Pts',(11.7747583744327,19.8474084919615,-7.8466185942614));
#36816=CARTESIAN_POINT('Ctrl Pts',(53.2371704815913,20.9503865390978,7.71107258897678));
#36817=CARTESIAN_POINT('Ctrl Pts',(53.144673323108,20.9426826122528,7.58626863816796));
#36818=CARTESIAN_POINT('Ctrl Pts',(53.0521761646248,20.9349786854078,7.46146468735915));
#36819=CARTESIAN_POINT('Ctrl Pts',(52.9596790061415,20.9272747585629,7.33666073655033));
#36820=CARTESIAN_POINT('Ctrl Pts',(43.7099631578178,20.1568820740671,-5.14373434433165));
#36821=CARTESIAN_POINT('Ctrl Pts',(26.9149655389531,20.093482749813,-11.2688794580951));
#36822=CARTESIAN_POINT('Ctrl Pts',(11.7749785445154,19.8548706708402,-7.84727131929312));
#36823=CARTESIAN_POINT('Ctrl Pts',(53.2371562237442,20.9537843889659,7.71097855898994));
#36824=CARTESIAN_POINT('Ctrl Pts',(53.1446640317764,20.9460931660003,7.58616824848811));
#36825=CARTESIAN_POINT('Ctrl Pts',(53.0521718398086,20.9384019430346,7.46135793798627));
#36826=CARTESIAN_POINT('Ctrl Pts',(52.9596796478408,20.9307107200689,7.33654762748443));
#36827=CARTESIAN_POINT('Ctrl Pts',(43.7104604510594,20.1615884235019,-5.14448342269933));
#36828=CARTESIAN_POINT('Ctrl Pts',(26.915163881532,20.0995966052706,-11.2692813811964));
#36829=CARTESIAN_POINT('Ctrl Pts',(11.7751987145981,19.862332849719,-7.84792404432485));
#36830=CARTESIAN_POINT('Ctrl Pts',(53.2371129264224,20.9641027630587,7.71069301471406));
#36831=CARTESIAN_POINT('Ctrl Pts',(53.1446358164523,20.9564501184246,7.58586339150147));
#36832=CARTESIAN_POINT('Ctrl Pts',(53.0521587064822,20.9487974737906,7.46103376828889));
#36833=CARTESIAN_POINT('Ctrl Pts',(52.9596815965122,20.9411448291565,7.3362041450763));
#36834=CARTESIAN_POINT('Ctrl Pts',(43.7119705995062,20.1758803657488,-5.14675817618243));
#36835=CARTESIAN_POINT('Ctrl Pts',(26.9157661956446,20.1181627721728,-11.2705019156746));
#36836=CARTESIAN_POINT('Ctrl Pts',(11.7758673130841,19.8849935193208,-7.8499061981334));
#36837=CARTESIAN_POINT('Ctrl Pts',(53.2370263315175,20.9847395112521,7.71012192605225));
#36838=CARTESIAN_POINT('Ctrl Pts',(53.1445793856301,20.9771640232786,7.58525367745488));
#36839=CARTESIAN_POINT('Ctrl Pts',(53.0521324397426,20.9695885353052,7.4603854288575));
#36840=CARTESIAN_POINT('Ctrl Pts',(52.9596854938552,20.9620130473318,7.33551718026014));
#36841=CARTESIAN_POINT('Ctrl Pts',(43.7149909051107,20.2044642499886,-5.15130767947685));
#36842=CARTESIAN_POINT('Ctrl Pts',(26.916970820079,20.1552951062578,-11.2729429882015));
#36843=CARTESIAN_POINT('Ctrl Pts',(11.777204510056,19.9303148585245,-7.85387050575054));
#36844=CARTESIAN_POINT('Ctrl Pts',(53.2368964218958,21.0156946339229,7.70926528516895));
#36845=CARTESIAN_POINT('Ctrl Pts',(53.144494727887,21.0082348808134,7.58433910112455));
#36846=CARTESIAN_POINT('Ctrl Pts',(53.0520930338782,21.000775127704,7.45941291708015));
#36847=CARTESIAN_POINT('Ctrl Pts',(52.9596913398694,20.9933153745945,7.33448673303575));
#36848=CARTESIAN_POINT('Ctrl Pts',(43.7195219389881,20.2473400636495,-5.15813167140387));
#36849=CARTESIAN_POINT('Ctrl Pts',(26.9187775261177,20.2109936225946,-11.2766048230408));
#36850=CARTESIAN_POINT('Ctrl Pts',(11.779210305514,19.9982968673298,-7.85981696717621));
#36851=CARTESIAN_POINT('Ctrl Pts',(53.2367664895543,21.0466497571015,7.70840863393207));
#36852=CARTESIAN_POINT('Ctrl Pts',(53.1444100549975,21.0393057386868,7.58342451789186));
#36853=CARTESIAN_POINT('Ctrl Pts',(53.0520536204406,21.0319617202721,7.45844040185166));
#36854=CARTESIAN_POINT('Ctrl Pts',(52.9596971858838,21.0246177018574,7.33345628581145));
#36855=CARTESIAN_POINT('Ctrl Pts',(43.7240537302011,20.2902158603888,-5.16495531820909));
#36856=CARTESIAN_POINT('Ctrl Pts',(26.9205839257141,20.2666921589687,-11.2802669552304));
#36857=CARTESIAN_POINT('Ctrl Pts',(11.7812161009719,20.0662788761352,-7.86576342860189));
#36858=CARTESIAN_POINT('Ctrl Pts',(53.236679856522,21.0672865061488,7.70783752790633));
#36859=CARTESIAN_POINT('Ctrl Pts',(53.1443535987569,21.0600196441101,7.5828147922693));
#36860=CARTESIAN_POINT('Ctrl Pts',(53.0520273409918,21.0527527820714,7.45779205663226));
#36861=CARTESIAN_POINT('Ctrl Pts',(52.9597010832266,21.0454859200326,7.33276932099522));
#36862=CARTESIAN_POINT('Ctrl Pts',(43.7270753067131,20.3187997161584,-5.16950424270833));
#36863=CARTESIAN_POINT('Ctrl Pts',(26.9217880354578,20.3038245267329,-11.2827085269013));
#36864=CARTESIAN_POINT('Ctrl Pts',(11.7825532979438,20.1116002153389,-7.86972773621902));
#36865=CARTESIAN_POINT('Ctrl Pts',(53.236636539877,21.0776048806767,7.70755197484126));
#36866=CARTESIAN_POINT('Ctrl Pts',(53.1443253705507,21.0703765968246,7.58250992942321));
#36867=CARTESIAN_POINT('Ctrl Pts',(53.0520142012244,21.0631483129724,7.45746788400516));
#36868=CARTESIAN_POINT('Ctrl Pts',(52.9597030318981,21.0559200291202,7.33242583858711));
#36869=CARTESIAN_POINT('Ctrl Pts',(43.7285860992663,20.3330916439037,-5.17177870321784));
#36870=CARTESIAN_POINT('Ctrl Pts',(26.9223900882949,20.3223907107576,-11.2839293144965));
#36871=CARTESIAN_POINT('Ctrl Pts',(11.7832218964298,20.1342608849406,-7.87170989002758));
#36872=CARTESIAN_POINT('Ctrl Pts',(53.236632365876,21.0785991614118,7.70752445888798));
#36873=CARTESIAN_POINT('Ctrl Pts',(53.1443226504748,21.0713745949617,7.58248055277538));
#36874=CARTESIAN_POINT('Ctrl Pts',(53.0520129350737,21.0641500285117,7.45743664666278));
#36875=CARTESIAN_POINT('Ctrl Pts',(52.9597032196725,21.0569254620617,7.33239274055018));
#36876=CARTESIAN_POINT('Ctrl Pts',(43.7287316795538,20.3344688170607,-5.17199787070987));
#36877=CARTESIAN_POINT('Ctrl Pts',(26.9224481022327,20.3241797521467,-11.2840469498454));
#36878=CARTESIAN_POINT('Ctrl Pts',(11.7832863227202,20.1364444718193,-7.87190089078457));
#36879=CARTESIAN_POINT('Ctrl Pts',(53.236628191875,21.0795934421468,7.7074969429347));
#36880=CARTESIAN_POINT('Ctrl Pts',(53.144319930399,21.0723725930989,7.58245117612755));
#36881=CARTESIAN_POINT('Ctrl Pts',(53.0520116689229,21.0651517440511,7.4574054093204));
#36882=CARTESIAN_POINT('Ctrl Pts',(52.9597034074469,21.0579308950032,7.33235964251325));
#36883=CARTESIAN_POINT('Ctrl Pts',(43.7288772598413,20.3358459902176,-5.17221703820191));
#36884=CARTESIAN_POINT('Ctrl Pts',(26.9225061161704,20.3259687935359,-11.2841645851943));
#36885=CARTESIAN_POINT('Ctrl Pts',(11.7833507490106,20.1386280586979,-7.87209189154155));
#36886=CARTESIAN_POINT('Ctrl Pts',(53.236624017874,21.0805877228818,7.70746942698142));
#36887=CARTESIAN_POINT('Ctrl Pts',(53.1443172103231,21.0733705912361,7.58242179947972));
#36888=CARTESIAN_POINT('Ctrl Pts',(53.0520104027722,21.0661534595904,7.45737417197801));
#36889=CARTESIAN_POINT('Ctrl Pts',(52.9597035952212,21.0589363279447,7.33232654447631));
#36890=CARTESIAN_POINT('Ctrl Pts',(43.7290228401288,20.3372231633746,-5.17243620569395));
#36891=CARTESIAN_POINT('Ctrl Pts',(26.9225641301082,20.327757834925,-11.2842822205432));
#36892=CARTESIAN_POINT('Ctrl Pts',(11.783415175301,20.1408116455766,-7.87228289229854));
#36893=CARTESIAN_POINT('',(46.8667964697728,20.5529756002067,0.877339649208832));
#36894=CARTESIAN_POINT('Ctrl Pts',(25.9230198769569,21.2883239772394,48.5187615226217));
#36895=CARTESIAN_POINT('Ctrl Pts',(26.0539515103827,21.2711623310641,48.0878393189679));
#36896=CARTESIAN_POINT('Ctrl Pts',(26.1782967764799,21.2542807820542,47.6534307220407));
#36897=CARTESIAN_POINT('Ctrl Pts',(26.6802445993609,21.1834525291307,45.7852132990113));
#36898=CARTESIAN_POINT('Ctrl Pts',(27.288585715814,21.0834264338425,42.914751594488));
#36899=CARTESIAN_POINT('Ctrl Pts',(27.7344129255298,20.9598507183575,38.6101384297008));
#36900=CARTESIAN_POINT('Ctrl Pts',(27.7267262169894,20.8461335954997,33.6244561521861));
#36901=CARTESIAN_POINT('Ctrl Pts',(27.0801344432569,20.7684839093916,28.7282178850793));
#36902=CARTESIAN_POINT('Ctrl Pts',(25.8262070857061,20.7206230093664,23.987509714119));
#36903=CARTESIAN_POINT('Ctrl Pts',(24.1034285018224,20.6916936542703,19.4064911568363));
#36904=CARTESIAN_POINT('Ctrl Pts',(21.8159838238208,20.6796111419738,15.0691197456759));
#36905=CARTESIAN_POINT('Ctrl Pts',(18.9964020956871,20.6722203558656,11.0412903808993));
#36906=CARTESIAN_POINT('Ctrl Pts',(16.2297782829761,20.6630225594897,7.83114746321505));
#36907=CARTESIAN_POINT('Ctrl Pts',(14.1622593406336,20.6508204531822,5.87251256806097));
#36908=CARTESIAN_POINT('Ctrl Pts',(12.7321233110437,20.6394053700742,4.6502519272584));
#36909=CARTESIAN_POINT('Ctrl Pts',(12.3848420399471,20.6364191357732,4.36299885106413));
#36910=CARTESIAN_POINT('Ctrl Pts',(12.033600930572,20.6332209087108,4.0818235088649));
#36911=CARTESIAN_POINT('Ctrl Pts',(26.2604130869634,21.2398788304839,48.1049156951145));
#36912=CARTESIAN_POINT('Ctrl Pts',(26.3890228772049,21.2217224127637,47.6743582450841));
#36913=CARTESIAN_POINT('Ctrl Pts',(26.5110378923674,21.2038412173392,47.2403414023796));
#36914=CARTESIAN_POINT('Ctrl Pts',(27.0030058479278,21.1287309618461,45.3739126709932));
#36915=CARTESIAN_POINT('Ctrl Pts',(27.5961224061632,21.0222253289507,42.5070844035404));
#36916=CARTESIAN_POINT('Ctrl Pts',(28.0195357773322,20.8890564489947,38.2105610058552));
#36917=CARTESIAN_POINT('Ctrl Pts',(27.9864836476654,20.7641817659416,33.237344487507));
#36918=CARTESIAN_POINT('Ctrl Pts',(27.3158697008056,20.6752847595175,28.3572877847353));
#36919=CARTESIAN_POINT('Ctrl Pts',(26.0398030951076,20.6159219251614,23.6363760825188));
#36920=CARTESIAN_POINT('Ctrl Pts',(24.2966827408469,20.5752144761384,19.0779816153495));
#36921=CARTESIAN_POINT('Ctrl Pts',(21.991500040255,20.5509334123338,14.7667026515359));
#36922=CARTESIAN_POINT('Ctrl Pts',(19.1573179832986,20.5308579865904,10.7683362842277));
#36923=CARTESIAN_POINT('Ctrl Pts',(16.3805824951291,20.510426256151,7.58571157269837));
#36924=CARTESIAN_POINT('Ctrl Pts',(14.3080816454852,20.4905046142392,5.64691895319579));
#36925=CARTESIAN_POINT('Ctrl Pts',(12.8753010992689,20.4739374093561,4.43819828994725));
#36926=CARTESIAN_POINT('Ctrl Pts',(12.5274194918876,20.469713411733,4.15420637215013));
#36927=CARTESIAN_POINT('Ctrl Pts',(12.1756128765411,20.4652767483487,3.87630351967435));
#36928=CARTESIAN_POINT('Ctrl Pts',(26.5978977585567,21.1822016013635,47.6908646032478));
#36929=CARTESIAN_POINT('Ctrl Pts',(26.7241687502308,21.1630886105529,47.2606817005154));
#36930=CARTESIAN_POINT('Ctrl Pts',(26.8438362667628,21.1442460408093,46.827066958471));
#36931=CARTESIAN_POINT('Ctrl Pts',(27.3257495502969,21.0650173413637,44.9624735955608));
#36932=CARTESIAN_POINT('Ctrl Pts',(27.9035295741986,20.9522796229575,42.0993524422593));
#36933=CARTESIAN_POINT('Ctrl Pts',(28.3043662171167,20.8098799445818,37.8110397719833));
#36934=CARTESIAN_POINT('Ctrl Pts',(28.2457618908011,20.6742608619688,32.8504467932067));
#36935=CARTESIAN_POINT('Ctrl Pts',(27.5509398519194,20.5745198093833,27.9867571563878));
#36936=CARTESIAN_POINT('Ctrl Pts',(26.2525464356161,20.5040526001987,23.2858628858746));
#36937=CARTESIAN_POINT('Ctrl Pts',(24.4888919980713,20.4519664047462,18.7503504098016));
#36938=CARTESIAN_POINT('Ctrl Pts',(22.1657719532826,20.4158956934967,14.4654712264667));
#36939=CARTESIAN_POINT('Ctrl Pts',(19.316780166669,20.3835681705302,10.496928045425));
#36940=CARTESIAN_POINT('Ctrl Pts',(16.5297402438784,20.3523071857454,7.34216931551517));
#36941=CARTESIAN_POINT('Ctrl Pts',(14.4521203095409,20.3249607749065,5.42346942398235));
#36942=CARTESIAN_POINT('Ctrl Pts',(13.0166006108032,20.3034475984546,4.22845797086557));
#36943=CARTESIAN_POINT('Ctrl Pts',(12.6680970903426,20.2980359714688,3.9477695260792));
#36944=CARTESIAN_POINT('Ctrl Pts',(12.3157045007277,20.29241155197,3.67318310060867));
#36945=CARTESIAN_POINT('Ctrl Pts',(27.8042303352092,20.942701117012,46.2104819450654));
#36946=CARTESIAN_POINT('Ctrl Pts',(27.9220864002744,20.9203083949833,45.7816721251138));
#36947=CARTESIAN_POINT('Ctrl Pts',(28.0333058486476,20.898168919688,45.3495315848581));
#36948=CARTESIAN_POINT('Ctrl Pts',(28.479027267791,20.8048139743737,43.4916681867343));
#36949=CARTESIAN_POINT('Ctrl Pts',(29.001609853494,20.6706999592586,40.6420644930631));
#36950=CARTESIAN_POINT('Ctrl Pts',(29.321194751232,20.496623371127,36.3835358770081));
#36951=CARTESIAN_POINT('Ctrl Pts',(29.1706179809275,20.3241023157428,31.4686302216622));
#36952=CARTESIAN_POINT('Ctrl Pts',(28.3886246832073,20.1870685788371,26.664106447373));
#36953=CARTESIAN_POINT('Ctrl Pts',(27.0097717402225,20.0783595881962,22.0355517219541));
#36954=CARTESIAN_POINT('Ctrl Pts',(25.1720430323228,19.9870599496472,17.5827492484273));
#36955=CARTESIAN_POINT('Ctrl Pts',(22.7840975954265,19.9103458023656,13.3933296353274));
#36956=CARTESIAN_POINT('Ctrl Pts',(19.8814149628274,19.8358125374395,9.53266872594138));
#36957=CARTESIAN_POINT('Ctrl Pts',(17.0568419677846,19.767331746443,6.47874833434411));
#36958=CARTESIAN_POINT('Ctrl Pts',(14.9604215493633,19.7145309927478,4.63275273616586));
#36959=CARTESIAN_POINT('Ctrl Pts',(13.5147630489044,19.6760973304852,3.48733920738447));
#36960=CARTESIAN_POINT('Ctrl Pts',(13.1639588284761,19.6666248028076,3.21861022039478));
#36961=CARTESIAN_POINT('Ctrl Pts',(12.809399673684,19.6569408091057,2.95603772191131));
#36962=CARTESIAN_POINT('Ctrl Pts',(29.521986074236,20.4780024533914,44.1011384618627));
#36963=CARTESIAN_POINT('Ctrl Pts',(29.6276533884862,20.4514551579611,43.6744145807348));
#36964=CARTESIAN_POINT('Ctrl Pts',(29.7266308829499,20.4251375618498,43.2445117569686));
#36965=CARTESIAN_POINT('Ctrl Pts',(30.1198857679885,20.3138746691076,41.3968573299702));
#36966=CARTESIAN_POINT('Ctrl Pts',(30.5624530626371,20.1526659052326,38.5675133009135));
#36967=CARTESIAN_POINT('Ctrl Pts',(30.7642453491852,19.938389785095,34.3530777137597));
#36968=CARTESIAN_POINT('Ctrl Pts',(30.4803031817061,19.7189203495023,29.5053887059681));
#36969=CARTESIAN_POINT('Ctrl Pts',(29.5718411556588,19.5342279169114,24.7875278899887));
#36970=CARTESIAN_POINT('Ctrl Pts',(28.0761487535003,19.3763677050182,20.2646564748078));
#36971=CARTESIAN_POINT('Ctrl Pts',(26.1307371975581,19.2344308170631,15.9325175110228));
#36972=CARTESIAN_POINT('Ctrl Pts',(23.6483675649021,19.1049298841923,11.88218726952));
#36973=CARTESIAN_POINT('Ctrl Pts',(20.667216710507,18.9752993129734,8.17858276534581));
#36974=CARTESIAN_POINT('Ctrl Pts',(17.7875458146746,18.8580619466085,5.27139096265361));
#36975=CARTESIAN_POINT('Ctrl Pts',(15.6633058517737,18.7718242877839,3.53114688412792));
#36976=CARTESIAN_POINT('Ctrl Pts',(14.2025389775091,18.7111415689428,2.45786531596827));
#36977=CARTESIAN_POINT('Ctrl Pts',(13.8483121118092,18.6963263828107,2.2065451923323));
#36978=CARTESIAN_POINT('Ctrl Pts',(13.4905360193496,18.6812985797984,1.96147587216487));
#36979=CARTESIAN_POINT('Ctrl Pts',(32.0272347697465,19.4355555088431,41.0215590310772));
#36980=CARTESIAN_POINT('Ctrl Pts',(32.1144819741636,19.4044605226273,40.5982064715866));
#36981=CARTESIAN_POINT('Ctrl Pts',(32.1949477980604,19.3735658358572,40.1719179195087));
#36982=CARTESIAN_POINT('Ctrl Pts',(32.5088196418466,19.2426748194849,38.3407454628268));
#36983=CARTESIAN_POINT('Ctrl Pts',(32.8303234267137,19.0517849995255,35.5435871503504));
#36984=CARTESIAN_POINT('Ctrl Pts',(32.853854400985,18.7933185397158,31.3980268277304));
#36985=CARTESIAN_POINT('Ctrl Pts',(32.3679847439182,18.5218580841843,26.6544248517635));
#36986=CARTESIAN_POINT('Ctrl Pts',(31.2678462688368,18.2836948825759,22.0699343228032));
#36987=CARTESIAN_POINT('Ctrl Pts',(29.594773201358,18.0697821020849,17.7091129242814));
#36988=CARTESIAN_POINT('Ctrl Pts',(27.4855694135664,17.8693333343866,13.5616312265872));
#36989=CARTESIAN_POINT('Ctrl Pts',(24.8590776326079,17.6778661310593,9.72378981616505));
#36990=CARTESIAN_POINT('Ctrl Pts',(21.757468922915,17.4826662284719,6.25984891758698));
#36991=CARTESIAN_POINT('Ctrl Pts',(18.7925807133286,17.3068805329357,3.57641430602537));
#36992=CARTESIAN_POINT('Ctrl Pts',(16.6247429863748,17.1802068447994,1.99736191703145));
#36993=CARTESIAN_POINT('Ctrl Pts',(15.1400283234621,17.0925519552341,1.03400839035698));
#36994=CARTESIAN_POINT('Ctrl Pts',(14.7803936608885,17.0712544126695,0.809254098100135));
#36995=CARTESIAN_POINT('Ctrl Pts',(14.417553197045,17.0497370990139,0.590927633578045));
#36996=CARTESIAN_POINT('Ctrl Pts',(34.8534706325002,17.8320672383652,37.5445499124197));
#36997=CARTESIAN_POINT('Ctrl Pts',(34.9191540130177,17.7976045693245,37.1253023664157));
#36998=CARTESIAN_POINT('Ctrl Pts',(34.9779337159588,17.7633163796081,36.7034247748685));
#36999=CARTESIAN_POINT('Ctrl Pts',(35.1987483607876,17.6178640028275,34.8924120264708));
#37000=CARTESIAN_POINT('Ctrl Pts',(35.3783275375406,17.4049846203341,32.1342451211723));
#37001=CARTESIAN_POINT('Ctrl Pts',(35.1928167690002,17.1135517229592,28.071271996886));
#37002=CARTESIAN_POINT('Ctrl Pts',(34.4700307079904,16.8027253827761,23.4518154045472));
#37003=CARTESIAN_POINT('Ctrl Pts',(33.1447876860525,16.523022337621,19.0257930993187));
#37004=CARTESIAN_POINT('Ctrl Pts',(31.2630832463472,16.2641978724915,14.8570951032009));
#37005=CARTESIAN_POINT('Ctrl Pts',(28.9609075929285,16.0157341831644,10.9282861435268));
#37006=CARTESIAN_POINT('Ctrl Pts',(26.164113782871,15.7719994721116,7.34182712399574));
#37007=CARTESIAN_POINT('Ctrl Pts',(22.9194789776465,15.5202180684676,4.16124318963596));
#37008=CARTESIAN_POINT('Ctrl Pts',(19.852782333304,15.2931736272884,1.74227197016013));
#37009=CARTESIAN_POINT('Ctrl Pts',(17.6323041133784,15.130708702949,0.353694351278024));
#37010=CARTESIAN_POINT('Ctrl Pts',(16.118415924838,15.0190926843839,-0.479769477849797));
#37011=CARTESIAN_POINT('Ctrl Pts',(15.7522333195276,14.9920326361705,-0.673092285248657));
#37012=CARTESIAN_POINT('Ctrl Pts',(15.3833028254314,14.9647422323135,-0.859739042833271));
#37013=CARTESIAN_POINT('Ctrl Pts',(37.542377320307,15.7638142683891,34.2340379990305));
#37014=CARTESIAN_POINT('Ctrl Pts',(37.5864967275411,15.7283726072843,33.8189895177017));
#37015=CARTESIAN_POINT('Ctrl Pts',(37.623576054751,15.6930928161318,33.4016424442209));
#37016=CARTESIAN_POINT('Ctrl Pts',(37.751216544469,15.543379415412,31.6114150579845));
#37017=CARTESIAN_POINT('Ctrl Pts',(37.7886730339078,15.3241289383934,28.8932275168839));
#37018=CARTESIAN_POINT('Ctrl Pts',(37.3937306124187,15.0227233638938,24.9144383133945));
#37019=CARTESIAN_POINT('Ctrl Pts',(36.4334261401257,14.6988957424381,20.4211498872596));
#37020=CARTESIAN_POINT('Ctrl Pts',(34.8822465580896,14.4035050799014,16.155848302069));
#37021=CARTESIAN_POINT('Ctrl Pts',(32.7907838851794,14.1252237593235,12.1817954315162));
#37022=CARTESIAN_POINT('Ctrl Pts',(30.2942408069272,13.8539516979883,8.47441520091897));
#37023=CARTESIAN_POINT('Ctrl Pts',(27.32537306915,13.5829362127958,5.14241023042879));
#37024=CARTESIAN_POINT('Ctrl Pts',(23.9355050652897,13.2994842764397,2.24860259607305));
#37025=CARTESIAN_POINT('Ctrl Pts',(20.764783485743,13.0425486753816,0.0972780310443223));
#37026=CARTESIAN_POINT('Ctrl Pts',(18.4899534807288,12.8585920936854,-1.09852526744414));
#37027=CARTESIAN_POINT('Ctrl Pts',(16.9456836958165,12.7324540777387,-1.80052542287351));
#37028=CARTESIAN_POINT('Ctrl Pts',(16.5727366200309,12.7018988467546,-1.96200324615093));
#37029=CARTESIAN_POINT('Ctrl Pts',(16.1975722418824,12.6711030837425,-2.11652390033856));
#37030=CARTESIAN_POINT('Ctrl Pts',(40.0687256573802,13.2592937677246,31.1228441461166));
#37031=CARTESIAN_POINT('Ctrl Pts',(40.0914257254572,13.2252177231213,30.7119049446456));
#37032=CARTESIAN_POINT('Ctrl Pts',(40.1069388012238,13.191306123502,30.2990220397433));
#37033=CARTESIAN_POINT('Ctrl Pts',(40.141937508551,13.0474600457288,28.5294034284981));
#37034=CARTESIAN_POINT('Ctrl Pts',(40.038048613647,12.8372075593629,25.8509681782089));
#37035=CARTESIAN_POINT('Ctrl Pts',(39.4346952432425,12.5484949329477,21.9561736216729));
#37036=CARTESIAN_POINT('Ctrl Pts',(38.2378601831066,12.2377054846042,17.5890305686027));
#37037=CARTESIAN_POINT('Ctrl Pts',(36.4614388310332,11.9522310106351,13.4846984409205));
#37038=CARTESIAN_POINT('Ctrl Pts',(34.160565676204,11.6797819251771,9.70584142430889));
#37039=CARTESIAN_POINT('Ctrl Pts',(31.4696986733579,11.4108111467242,6.22069601970489));
#37040=CARTESIAN_POINT('Ctrl Pts',(28.3283877321082,11.1374939458242,3.1442866710006));
#37041=CARTESIAN_POINT('Ctrl Pts',(24.7924587223825,10.8473681096278,0.538753743941756));
#37042=CARTESIAN_POINT('Ctrl Pts',(21.5166685226697,10.5820480444149,-1.3433864264039));
#37043=CARTESIAN_POINT('Ctrl Pts',(19.1865556611937,10.3910369789073,-2.34521593896695));
#37044=CARTESIAN_POINT('Ctrl Pts',(17.6112105856552,10.2599216927486,-2.91490446819573));
#37045=CARTESIAN_POINT('Ctrl Pts',(17.2314099331844,10.2281653805015,-3.04431791604507));
#37046=CARTESIAN_POINT('Ctrl Pts',(16.8499985273585,10.1961599190035,-3.1664797330386));
#37047=CARTESIAN_POINT('Ctrl Pts',(42.4513879531089,10.420684636249,28.1887961890181));
#37048=CARTESIAN_POINT('Ctrl Pts',(42.4528615514467,10.3898269637342,27.7817853751185));
#37049=CARTESIAN_POINT('Ctrl Pts',(42.4469943536053,10.3591499865554,27.3732089758612));
#37050=CARTESIAN_POINT('Ctrl Pts',(42.3901211918335,10.2291883131935,25.6236312047506));
#37051=CARTESIAN_POINT('Ctrl Pts',(42.1460260161208,10.0401067219452,22.984119835829));
#37052=CARTESIAN_POINT('Ctrl Pts',(41.3358278887554,9.78206378055234,19.1722162135672));
#37053=CARTESIAN_POINT('Ctrl Pts',(39.9040992893687,9.50499638561923,14.9301076971436));
#37054=CARTESIAN_POINT('Ctrl Pts',(37.9038077627142,9.24981780003299,10.9858713610508));
#37055=CARTESIAN_POINT('Ctrl Pts',(35.394592979796,9.00337535985762,7.40159323672565));
#37056=CARTESIAN_POINT('Ctrl Pts',(32.5102108332376,8.75677479408939,4.13827932323636));
#37057=CARTESIAN_POINT('Ctrl Pts',(29.1969188360728,8.50116890088297,1.31733874904121));
#37058=CARTESIAN_POINT('Ctrl Pts',(25.5150150389335,8.22444592813344,-0.999758566332292));
#37059=CARTESIAN_POINT('Ctrl Pts',(22.1339602470639,7.96804930448713,-2.61237505739787));
#37060=CARTESIAN_POINT('Ctrl Pts',(19.7482465529448,7.78162503245108,-3.4198681063926));
#37061=CARTESIAN_POINT('Ctrl Pts',(18.1415532826121,7.65323614745839,-3.85696102050637));
#37062=CARTESIAN_POINT('Ctrl Pts',(17.7549106912631,7.62212996336316,-3.95424830145647));
#37063=CARTESIAN_POINT('Ctrl Pts',(17.3673388607139,7.59076668565169,-4.04399793803123));
#37064=CARTESIAN_POINT('Ctrl Pts',(44.6372900743475,7.18298363715391,25.4983456154475));
#37065=CARTESIAN_POINT('Ctrl Pts',(44.6178691074574,7.15763661423686,25.0949333155389));
#37066=CARTESIAN_POINT('Ctrl Pts',(44.5909499550986,7.13250342173354,24.6903522149865));
#37067=CARTESIAN_POINT('Ctrl Pts',(44.4435968973406,7.02634360727853,22.9595720745829));
#37068=CARTESIAN_POINT('Ctrl Pts',(44.0613654920327,6.87350147707393,20.3571404287178));
#37069=CARTESIAN_POINT('Ctrl Pts',(43.0472175782345,6.66841421880391,16.6255566287883));
#37070=CARTESIAN_POINT('Ctrl Pts',(41.3837014192008,6.45075222930465,12.505726151791));
#37071=CARTESIAN_POINT('Ctrl Pts',(39.1622763252268,6.25122984378583,8.71914937469031));
#37072=CARTESIAN_POINT('Ctrl Pts',(36.4470480163677,6.05595707526583,5.32735253621606));
#37073=CARTESIAN_POINT('Ctrl Pts',(33.3711340094357,5.8568061689083,2.28405026921364));
#37074=CARTESIAN_POINT('Ctrl Pts',(29.8873919147407,5.64398234710963,-0.282886838428735));
#37075=CARTESIAN_POINT('Ctrl Pts',(26.0605646588228,5.40587468584602,-2.31265259581178));
#37076=CARTESIAN_POINT('Ctrl Pts',(22.5748071053324,5.18017895256177,-3.6564426503721));
#37077=CARTESIAN_POINT('Ctrl Pts',(20.1336349934671,5.01301666232781,-4.26989781319475));
#37078=CARTESIAN_POINT('Ctrl Pts',(18.4956094199414,4.89707445701614,-4.57453714520048));
#37079=CARTESIAN_POINT('Ctrl Pts',(18.1021997947913,4.86894780999335,-4.63975778560386));
#37080=CARTESIAN_POINT('Ctrl Pts',(17.7086109162641,4.84055053954568,-4.69718161228497));
#37081=CARTESIAN_POINT('Ctrl Pts',(46.6002512122511,3.57357815210241,23.0851472908221));
#37082=CARTESIAN_POINT('Ctrl Pts',(46.5604134978277,3.55599962931061,22.6848298673109));
#37083=CARTESIAN_POINT('Ctrl Pts',(46.5129192765137,3.53868515668548,22.2837522544351));
#37084=CARTESIAN_POINT('Ctrl Pts',(46.2771234824041,3.46609807861293,20.5697250603014));
#37085=CARTESIAN_POINT('Ctrl Pts',(45.7597972462748,3.36435917107101,18.0013127653728));
#37086=CARTESIAN_POINT('Ctrl Pts',(44.5460060590501,3.23426720235262,14.3456829986935));
#37087=CARTESIAN_POINT('Ctrl Pts',(42.6554075408894,3.10147907156715,10.3433104165254));
#37088=CARTESIAN_POINT('Ctrl Pts',(40.2171323555533,2.98285053627008,6.70992527865091));
#37089=CARTESIAN_POINT('Ctrl Pts',(37.29972468766,2.86388130857434,3.50650323924174));
#37090=CARTESIAN_POINT('Ctrl Pts',(34.0357422770818,2.73730530568202,0.679396844997027));
#37091=CARTESIAN_POINT('Ctrl Pts',(30.384537644396,2.59247375589619,-1.63698871367901));
#37092=CARTESIAN_POINT('Ctrl Pts',(26.4152859351303,2.41842603756845,-3.38251562380317));
#37093=CARTESIAN_POINT('Ctrl Pts',(22.8266296158437,2.24547053120763,-4.45988818251451));
#37094=CARTESIAN_POINT('Ctrl Pts',(20.3309757484496,2.11246131963295,-4.88075398812767));
#37095=CARTESIAN_POINT('Ctrl Pts',(18.6621864827798,2.01884144332686,-5.05384262057585));
#37096=CARTESIAN_POINT('Ctrl Pts',(18.2622021015115,1.99605339732081,-5.08725599825241));
#37097=CARTESIAN_POINT('Ctrl Pts',(17.8628413159654,1.9729679754383,-5.11265663696635));
#37098=CARTESIAN_POINT('Ctrl Pts',(48.1177386369166,0.237308438758995,21.2223754846663));
#37099=CARTESIAN_POINT('Ctrl Pts',(48.0607951996036,0.227921876287717,20.8242811153145));
#37100=CARTESIAN_POINT('Ctrl Pts',(47.9960602567766,0.218854274805993,20.4257840939615));
#37101=CARTESIAN_POINT('Ctrl Pts',(47.6861498686287,0.181679983795775,18.724346543423));
#37102=CARTESIAN_POINT('Ctrl Pts',(47.0555604149621,0.133848323063104,16.1824364307684));
#37103=CARTESIAN_POINT('Ctrl Pts',(45.6742498357681,0.0830496793456984,
12.5880909151258));
#37104=CARTESIAN_POINT('Ctrl Pts',(43.5929738746605,0.0403924264632703,
8.68214080760531));
#37105=CARTESIAN_POINT('Ctrl Pts',(40.9724801352348,0.00837005963384143,
5.17606176509414));
#37106=CARTESIAN_POINT('Ctrl Pts',(37.8851037245238,-0.0279539839125438,
2.13035959848029));
#37107=CARTESIAN_POINT('Ctrl Pts',(34.4629830745002,-0.0750512999789021,
-0.51497625431155));
#37108=CARTESIAN_POINT('Ctrl Pts',(30.6709672266821,-0.14423024726241,-2.61989139939369));
#37109=CARTESIAN_POINT('Ctrl Pts',(26.5820286964953,-0.245792879606331,
-4.12482945449056));
#37110=CARTESIAN_POINT('Ctrl Pts',(22.9069936436346,-0.358291148292244,
-4.97629232812478));
#37111=CARTESIAN_POINT('Ctrl Pts',(20.3657037027299,-0.451704594358635,
-5.23361066140274));
#37112=CARTESIAN_POINT('Ctrl Pts',(18.6711961566749,-0.519340602547392,
-5.29491549463405));
#37113=CARTESIAN_POINT('Ctrl Pts',(18.26576526766,-0.535923052101836,-5.30134231507661));
#37114=CARTESIAN_POINT('Ctrl Pts',(17.8616764537007,-0.552841667182328,
-5.29961424607418));
#37115=CARTESIAN_POINT('Ctrl Pts',(49.0111526470788,-2.14030259993981,20.1280824173318));
#37116=CARTESIAN_POINT('Ctrl Pts',(48.9431158357957,-2.14321532053782,19.7311392813689));
#37117=CARTESIAN_POINT('Ctrl Pts',(48.8671976767669,-2.14576465810466,19.3340301364558));
#37118=CARTESIAN_POINT('Ctrl Pts',(48.5092053965927,-2.15494826818845,17.6395593959033));
#37119=CARTESIAN_POINT('Ctrl Pts',(47.8050951102084,-2.16016260296573,15.1131718254244));
#37120=CARTESIAN_POINT('Ctrl Pts',(46.3149438817565,-2.1481556077715,11.556583273664));
#37121=CARTESIAN_POINT('Ctrl Pts',(44.1096887388597,-2.11918777525101,7.71144046011049));
#37122=CARTESIAN_POINT('Ctrl Pts',(41.370632841532,-2.08197924289826,4.28693588598887));
#37123=CARTESIAN_POINT('Ctrl Pts',(38.1726332889339,-2.05170003121316,1.34326068419944));
#37124=CARTESIAN_POINT('Ctrl Pts',(34.6475936509573,-2.03426137368081,-1.18387570229488));
#37125=CARTESIAN_POINT('Ctrl Pts',(30.7639815309873,-2.04135770257883,-3.15062216354145));
#37126=CARTESIAN_POINT('Ctrl Pts',(26.5973047018925,-2.08278583441843,-4.49781925489811));
#37127=CARTESIAN_POINT('Ctrl Pts',(22.8662926524275,-2.14471303148954,-5.20084440966807));
#37128=CARTESIAN_POINT('Ctrl Pts',(20.2955537880838,-2.20477046252904,-5.35051189893769));
#37129=CARTESIAN_POINT('Ctrl Pts',(18.5845115980973,-2.25046208753918,-5.33818290167311));
#37130=CARTESIAN_POINT('Ctrl Pts',(18.1756045924178,-2.26180965939547,-5.3268552459772));
#37131=CARTESIAN_POINT('Ctrl Pts',(17.7685257087919,-2.27353152926925,-5.30730083266003));
#37132=CARTESIAN_POINT('Ctrl Pts',(49.5850624656363,-3.83428286431684,19.4261939233155));
#37133=CARTESIAN_POINT('Ctrl Pts',(49.5094794801401,-3.83237339034492,19.0299116731508));
#37134=CARTESIAN_POINT('Ctrl Pts',(49.4259532096492,-3.83006698099443,18.6336267626953));
#37135=CARTESIAN_POINT('Ctrl Pts',(49.0352476004593,-3.81839846831683,16.9433938910075));
#37136=CARTESIAN_POINT('Ctrl Pts',(48.2811000721071,-3.79185933798401,14.4268660936007));
#37137=CARTESIAN_POINT('Ctrl Pts',(46.7168351773588,-3.73301479320489,10.8951171019885));
#37138=CARTESIAN_POINT('Ctrl Pts',(44.4271250001086,-3.65055513724086,7.09059062588532));
#37139=CARTESIAN_POINT('Ctrl Pts',(41.6072775704128,-3.56151400652134,3.72112407924795));
#37140=CARTESIAN_POINT('Ctrl Pts',(38.3338930647704,-3.48120332570528,0.846689546782518));
#37141=CARTESIAN_POINT('Ctrl Pts',(34.7387295945766,-3.41513875248544,-1.59997654848575));
#37142=CARTESIAN_POINT('Ctrl Pts',(30.7927411759451,-3.37526128513496,-3.47238823132519));
#37143=CARTESIAN_POINT('Ctrl Pts',(26.5731913388433,-3.37099617994084,-4.71166498849067));
#37144=CARTESIAN_POINT('Ctrl Pts',(22.8041754625968,-3.39437469848804,-5.31300502085438));
#37145=CARTESIAN_POINT('Ctrl Pts',(20.2135086951711,-3.42893690611626,-5.38885186457644));
#37146=CARTESIAN_POINT('Ctrl Pts',(18.4913093104333,-3.45783930783476,-5.32600713004844));
#37147=CARTESIAN_POINT('Ctrl Pts',(18.0800672982954,-3.46518513130081,-5.30251003400118));
#37148=CARTESIAN_POINT('Ctrl Pts',(17.6709912904296,-3.47293757911652,-5.27074753251649));
#37149=CARTESIAN_POINT('Ctrl Pts',(49.7385656365263,-4.30636894546118,19.2385804425128));
#37150=CARTESIAN_POINT('Ctrl Pts',(49.6609212476581,-4.3031084050989,18.8424609291718));
#37151=CARTESIAN_POINT('Ctrl Pts',(49.5753160757238,-4.29944065268701,18.4463835567366));
#37152=CARTESIAN_POINT('Ctrl Pts',(49.1756692040682,-4.28192251284736,16.7572339716752));
#37153=CARTESIAN_POINT('Ctrl Pts',(48.4078353322892,-4.24645759656194,14.2433025862439));
#37154=CARTESIAN_POINT('Ctrl Pts',(46.8232750809732,-4.17439213330946,10.7182450608962));
#37155=CARTESIAN_POINT('Ctrl Pts',(44.5104172755431,-4.07676875425951,6.92476319565399));
#37156=CARTESIAN_POINT('Ctrl Pts',(41.6684115908783,-3.97294922980807,3.57035153883128));
#37157=CARTESIAN_POINT('Ctrl Pts',(38.3743494619475,-3.87828739688684,0.714912437194819));
#37158=CARTESIAN_POINT('Ctrl Pts',(34.7599610153453,-3.79820251809058,-1.70965444329932));
#37159=CARTESIAN_POINT('Ctrl Pts',(30.7968900398997,-3.74469501429227,-3.55614991710789));
#37160=CARTESIAN_POINT('Ctrl Pts',(26.5628886623099,-3.72710099262819,-4.76579596134831));
#37161=CARTESIAN_POINT('Ctrl Pts',(22.7835127443776,-3.7392015362719,-5.33925141242045));
#37162=CARTESIAN_POINT('Ctrl Pts',(20.1874313455853,-3.76629674044718,-5.39487746385998));
#37163=CARTESIAN_POINT('Ctrl Pts',(18.4622079723539,-3.79028538091932,-5.31820612127411));
#37164=CARTESIAN_POINT('Ctrl Pts',(18.0503342711803,-3.79646095010219,-5.29138066967352));
#37165=CARTESIAN_POINT('Ctrl Pts',(17.6407192216084,-3.80305340259771,-5.25628164552003));
#37166=CARTESIAN_POINT('Ctrl Pts',(49.8867262771747,-4.78145508078572,19.0576143929379));
#37167=CARTESIAN_POINT('Ctrl Pts',(49.8070488184353,-4.77682808742727,18.6616387837467));
#37168=CARTESIAN_POINT('Ctrl Pts',(49.7193926455521,-4.7717826224726,18.2657493044296));
#37169=CARTESIAN_POINT('Ctrl Pts',(49.3109216037794,-4.74834091216943,16.5775956967118));
#37170=CARTESIAN_POINT('Ctrl Pts',(48.5295704247379,-4.70381966688121,14.0661310574747));
#37171=CARTESIAN_POINT('Ctrl Pts',(46.9249416035674,-4.61828583278682,10.5475836926096));
#37172=CARTESIAN_POINT('Ctrl Pts',(44.5891740940081,-4.50515190400754,6.76494960996389));
#37173=CARTESIAN_POINT('Ctrl Pts',(41.7252227642596,-4.38613315046716,3.42541182621241));
#37174=CARTESIAN_POINT('Ctrl Pts',(38.4106787509553,-4.27662792828432,0.58879394549261));
#37175=CARTESIAN_POINT('Ctrl Pts',(34.7772564846155,-4.18197237106197,-1.81385442996729));
#37176=CARTESIAN_POINT('Ctrl Pts',(30.7972906070539,-4.11421750462538,-3.63463742552607));
#37177=CARTESIAN_POINT('Ctrl Pts',(26.5490240788154,-4.08262421860679,-4.81490468456639));
#37178=CARTESIAN_POINT('Ctrl Pts',(22.759448415022,-4.0828488851085,-5.36074766386016));
#37179=CARTESIAN_POINT('Ctrl Pts',(20.1580533176614,-4.10207414795096,-5.39637337123085));
#37180=CARTESIAN_POINT('Ctrl Pts',(18.429869561442,-4.12088738197538,-5.30603685065097));
#37181=CARTESIAN_POINT('Ctrl Pts',(18.0173781005166,-4.12583098108427,-5.27592339496274));
#37182=CARTESIAN_POINT('Ctrl Pts',(17.607236583243,-4.13120272145022,-5.23752968435663));
#37183=CARTESIAN_POINT('',(28.5514340253946,20.7105311502984,37.17636308254));
#37184=CARTESIAN_POINT('Ctrl Pts',(28.5514340253946,20.7105311502984,37.17636308254));
#37185=CARTESIAN_POINT('Ctrl Pts',(28.6887070741992,20.5483438544848,31.9945680076874));
#37186=CARTESIAN_POINT('Ctrl Pts',(27.8005885200067,20.4520245495079,26.7953695353565));
#37187=CARTESIAN_POINT('Ctrl Pts',(24.2300859427647,20.3052748660675,17.0649705156928));
#37188=CARTESIAN_POINT('Ctrl Pts',(21.5497888275062,20.248474007324,12.5314470346895));
#37189=CARTESIAN_POINT('Ctrl Pts',(18.0980606826517,20.1925493450898,8.66958605760119));
#37190=CARTESIAN_POINT('',(45.834019355174,-3.27137091447504,9.82390285882801));
#37191=CARTESIAN_POINT('Ctrl Pts',(28.5514340253913,20.7105311502992,37.1763630825353));
#37192=CARTESIAN_POINT('Ctrl Pts',(31.0601642882562,19.9641940681954,35.2496594015446));
#37193=CARTESIAN_POINT('Ctrl Pts',(33.2932193363368,18.7336189223949,33.1249281443677));
#37194=CARTESIAN_POINT('Ctrl Pts',(37.3699780270222,15.6437709263415,28.4860565308901));
#37195=CARTESIAN_POINT('Ctrl Pts',(39.2033043779382,13.6706054953475,25.8687734374218));
#37196=CARTESIAN_POINT('Ctrl Pts',(42.1018618790161,9.45712578015146,20.8061375995457));
#37197=CARTESIAN_POINT('Ctrl Pts',(43.224541292629,7.18268855808118,18.3050729961215));
#37198=CARTESIAN_POINT('Ctrl Pts',(44.8943670414634,2.26699026933697,13.6969285615372));
#37199=CARTESIAN_POINT('Ctrl Pts',(45.4569546562068,-0.365223992194631,
11.583121612936));
#37200=CARTESIAN_POINT('Ctrl Pts',(45.8340194423595,-3.27137053313469,9.82390224755894));
#37201=CARTESIAN_POINT('Ctrl Pts',(45.8340189392194,-3.27137100135121,9.82390309631628));
#37202=CARTESIAN_POINT('Ctrl Pts',(45.4471084733847,-3.25992112204953,9.15042791312507));
#37203=CARTESIAN_POINT('Ctrl Pts',(45.0361013987857,-3.24789096533569,8.49437671617948));
#37204=CARTESIAN_POINT('Ctrl Pts',(44.6023222643424,-3.23555894384663,7.85680669322666));
#37205=CARTESIAN_POINT('Ctrl Pts',(43.5399816289705,-3.2053573815679,6.29537487344335));
#37206=CARTESIAN_POINT('Ctrl Pts',(42.3410592562038,-3.17334534347451,4.84478916593907));
#37207=CARTESIAN_POINT('Ctrl Pts',(41.025128272205,-3.14345008158506,3.52048655147805));
#37208=CARTESIAN_POINT('Ctrl Pts',(40.1478409050367,-3.12351990598108,2.63761809705187));
#37209=CARTESIAN_POINT('Ctrl Pts',(39.2185497053661,-3.10453051989494,1.81087546743184));
#37210=CARTESIAN_POINT('Ctrl Pts',(38.2430820542904,-3.08752071373526,1.04479859058942));
#37211=CARTESIAN_POINT('Ctrl Pts',(37.2676144037253,-3.07051090758448,0.278721714147996));
#37212=CARTESIAN_POINT('Ctrl Pts',(36.245970301801,-3.0554806813514,-0.426689409586692));
#37213=CARTESIAN_POINT('Ctrl Pts',(35.183986846522,-3.04339100491455,-1.06691002414564));
#37214=CARTESIAN_POINT('Ctrl Pts',(33.5910116655829,-3.02525649028182,-2.02724094479067));
#37215=CARTESIAN_POINT('Ctrl Pts',(31.9072729398591,-3.01373821257335,-2.8408932202102));
#37216=CARTESIAN_POINT('Ctrl Pts',(30.1525134708022,-3.01128625574909,-3.49270629610018));
#37217=CARTESIAN_POINT('Ctrl Pts',(28.9826738275111,-3.00965161787009,-3.92724834567317));
#37218=CARTESIAN_POINT('Ctrl Pts',(27.7812694094895,-3.01204645592803,-4.2898618624831));
#37219=CARTESIAN_POINT('Ctrl Pts',(26.5541510246005,-3.01891855380822,-4.57608275222957));
#37220=CARTESIAN_POINT('Ctrl Pts',(25.3270327868496,-3.02579065086441,-4.86230360765662));
#37221=CARTESIAN_POINT('Ctrl Pts',(24.0742005883685,-3.03714000665748,-5.07213185436673));
#37222=CARTESIAN_POINT('Ctrl Pts',(22.8014968021072,-3.05321938564873,-5.20111578381779));
#37223=CARTESIAN_POINT('Ctrl Pts',(22.277058467955,-3.05984515577954,-5.25426571377315));
#37224=CARTESIAN_POINT('Ctrl Pts',(21.7492459773433,-3.06727406915266,-5.29368838411695));
#37225=CARTESIAN_POINT('Ctrl Pts',(21.2184673472733,-3.07550335254719,-5.31907358707771));
#37226=CARTESIAN_POINT('Ctrl Pts',(49.988903440698,-4.68328060676847,18.9373181639873));
#37227=CARTESIAN_POINT('Ctrl Pts',(49.9084825111689,-4.67927906663786,18.5401457639636));
#37228=CARTESIAN_POINT('Ctrl Pts',(49.8200206604983,-4.67486342687383,18.1430770906299));
#37229=CARTESIAN_POINT('Ctrl Pts',(49.4090563410411,-4.65418501649615,16.4549589916609));
#37230=CARTESIAN_POINT('Ctrl Pts',(48.6244718746128,-4.61395560865182,13.9459576997312));
#37231=CARTESIAN_POINT('Ctrl Pts',(47.0150672697257,-4.53496565777432,10.4313206499587));
#37232=CARTESIAN_POINT('Ctrl Pts',(44.6738386245635,-4.42959393838223,6.65349671488799));
#37233=CARTESIAN_POINT('Ctrl Pts',(41.8045972279016,-4.31850354734918,3.31907618662271));
#37234=CARTESIAN_POINT('Ctrl Pts',(38.4849815346274,-4.2170896233612,0.487882275093385));
#37235=CARTESIAN_POINT('Ctrl Pts',(34.8466814723617,-4.13063759391767,-1.90908600717672));
#37236=CARTESIAN_POINT('Ctrl Pts',(30.8621174859164,-4.07121155600733,-3.72386951312436));
#37237=CARTESIAN_POINT('Ctrl Pts',(26.6095816084296,-4.04803120464602,-4.89781636015318));
#37238=CARTESIAN_POINT('Ctrl Pts',(22.816595861502,-4.055480889925,-5.43802215119413));
#37239=CARTESIAN_POINT('Ctrl Pts',(20.2131109731287,-4.07952578289679,-5.46975503770605));
#37240=CARTESIAN_POINT('Ctrl Pts',(18.4813977696839,-4.10152925776619,-5.37669708188378));
#37241=CARTESIAN_POINT('Ctrl Pts',(18.0664172651078,-4.1072571624472,-5.34575229868548));
#37242=CARTESIAN_POINT('Ctrl Pts',(17.6538343163326,-4.11341014061892,-5.3064425898067));
#37243=CARTESIAN_POINT('Ctrl Pts',(49.8052654310235,-4.24009445412503,19.1620102019682));
#37244=CARTESIAN_POINT('Ctrl Pts',(49.7270640779776,-4.23725223817857,18.7645791085326));
#37245=CARTESIAN_POINT('Ctrl Pts',(49.6408401586447,-4.23400446880359,18.3672011094939));
#37246=CARTESIAN_POINT('Ctrl Pts',(49.2394704796158,-4.21832863439708,16.6775446746884));
#37247=CARTESIAN_POINT('Ctrl Pts',(48.469563803724,-4.18572164472913,14.1652201577743));
#37248=CARTESIAN_POINT('Ctrl Pts',(46.8819417217329,-4.11799618192084,10.6427061382864));
#37249=CARTESIAN_POINT('Ctrl Pts',(44.5655843103686,-4.02550335874969,6.85234360018412));
#37250=CARTESIAN_POINT('Ctrl Pts',(41.720191767349,-3.92690475481451,3.50123729401103));
#37251=CARTESIAN_POINT('Ctrl Pts',(38.4228868628256,-3.83755718932749,0.649285878422626));
#37252=CARTESIAN_POINT('Ctrl Pts',(34.8053848532926,-3.76285616468038,-1.771645267414));
#37253=CARTESIAN_POINT('Ctrl Pts',(30.8393834269129,-3.71481495977278,-3.61432174429343));
#37254=CARTESIAN_POINT('Ctrl Pts',(26.6026633134566,-3.70275434803773,-4.81996639174259));
#37255=CARTESIAN_POINT('Ctrl Pts',(22.8211151345275,-3.71962751323487,-5.38986722901264));
#37256=CARTESIAN_POINT('Ctrl Pts',(20.2236998257982,-3.74992063397164,-5.44304425293645));
#37257=CARTESIAN_POINT('Ctrl Pts',(18.4954234201959,-3.77604797989279,-5.36463613821515));
#37258=CARTESIAN_POINT('Ctrl Pts',(18.0811694161186,-3.78276245762616,-5.33722888584272));
#37259=CARTESIAN_POINT('Ctrl Pts',(17.6692128822404,-3.78989370687861,-5.30146219782923));
#37260=CARTESIAN_POINT('Ctrl Pts',(49.6179682497192,-3.80075287541765,19.3912747502332));
#37261=CARTESIAN_POINT('Ctrl Pts',(49.5420021295319,-3.79905339336963,18.9935700937101));
#37262=CARTESIAN_POINT('Ctrl Pts',(49.4580313687019,-3.79695621683146,18.5958674888762));
#37263=CARTESIAN_POINT('Ctrl Pts',(49.0663192419952,-3.78620663871065,16.9046059783843));
#37264=CARTESIAN_POINT('Ctrl Pts',(48.3111769729803,-3.76109400159902,14.3888636064159));
#37265=CARTESIAN_POINT('Ctrl Pts',(46.7454425808103,-3.70440674399875,10.8583542991997));
#37266=CARTESIAN_POINT('Ctrl Pts',(44.4540536385309,-3.62448835210827,7.05534342793885));
#37267=CARTESIAN_POINT('Ctrl Pts',(41.632583178043,-3.53802316526296,3.6874762390026));
#37268=CARTESIAN_POINT('Ctrl Pts',(38.3576469800422,-3.46032715355504,0.814721189671188));
#37269=CARTESIAN_POINT('Ctrl Pts',(34.7609965086106,-3.39690914788247,-1.63020282853092));
#37270=CARTESIAN_POINT('Ctrl Pts',(30.8136110902934,-3.35971861494906,-3.50079583530382));
#37271=CARTESIAN_POINT('Ctrl Pts',(26.5927665124587,-3.35817927654809,-4.73817887084428));
#37272=CARTESIAN_POINT('Ctrl Pts',(22.8227159303205,-3.38391914529348,-5.33784454604279));
#37273=CARTESIAN_POINT('Ctrl Pts',(20.2314124468981,-3.42007079724739,-5.41254106449418));
#37274=CARTESIAN_POINT('Ctrl Pts',(18.5066013369709,-3.45006162272336,-5.34884664801723));
#37275=CARTESIAN_POINT('Ctrl Pts',(18.0930800003721,-3.45770043113048,-5.32499411449625));
#37276=CARTESIAN_POINT('Ctrl Pts',(17.6817553325294,-3.46574819271174,-5.29278929448323));
#37277=CARTESIAN_POINT('Ctrl Pts',(48.944645465743,-2.2653457359543,20.2158180144603));
#37278=CARTESIAN_POINT('Ctrl Pts',(48.876613446234,-2.26761569662348,19.8170914326486));
#37279=CARTESIAN_POINT('Ctrl Pts',(48.8006389988634,-2.26951335386862,19.4181870566248));
#37280=CARTESIAN_POINT('Ctrl Pts',(48.4431952693583,-2.27586002752392,17.7210231775921));
#37281=CARTESIAN_POINT('Ctrl Pts',(47.7404087354438,-2.27671432942662,15.1928853145256));
#37282=CARTESIAN_POINT('Ctrl Pts',(46.2522083988626,-2.25814179129592,11.6337547981385));
#37283=CARTESIAN_POINT('Ctrl Pts',(44.0491870356822,-2.2214798205824,7.78574796375675));
#37284=CARTESIAN_POINT('Ctrl Pts',(41.3123112021794,-2.17652897108851,4.35851069495035));
#37285=CARTESIAN_POINT('Ctrl Pts',(38.1164400187034,-2.13845241575724,1.41223808195806));
#37286=CARTESIAN_POINT('Ctrl Pts',(34.5934903935758,-2.11316923258448,-1.11738683308532));
#37287=CARTESIAN_POINT('Ctrl Pts',(30.7119251016983,-2.11235831802136,-3.086485669945));
#37288=CARTESIAN_POINT('Ctrl Pts',(26.5472626963964,-2.14581153060268,-4.4359016919901));
#37289=CARTESIAN_POINT('Ctrl Pts',(22.8179615735058,-2.20085463389179,-5.14073972565149));
#37290=CARTESIAN_POINT('Ctrl Pts',(20.2483577846406,-2.25628908058851,-5.29155852335286));
#37291=CARTESIAN_POINT('Ctrl Pts',(18.5358669958649,-2.29898278275007,-5.27995411268357));
#37292=CARTESIAN_POINT('Ctrl Pts',(18.1249528052827,-2.30966173471912,-5.26869642388997));
#37293=CARTESIAN_POINT('Ctrl Pts',(17.7158788419632,-2.32072459453129,-5.24912151426549));
#37294=CARTESIAN_POINT('Ctrl Pts',(47.6809434698657,0.42091842584111,21.764906316134));
#37295=CARTESIAN_POINT('Ctrl Pts',(47.6272638993357,0.412015546281074,21.3641829634742));
#37296=CARTESIAN_POINT('Ctrl Pts',(47.565755337614,0.403442573942463,20.9629650061253));
#37297=CARTESIAN_POINT('Ctrl Pts',(47.2703119003642,0.368526239150617,19.2545662589912));
#37298=CARTESIAN_POINT('Ctrl Pts',(46.6622260261044,0.324281374370589,16.7032339039416));
#37299=CARTESIAN_POINT('Ctrl Pts',(45.3142072503292,0.279215865745994,13.0914162878439));
#37300=CARTESIAN_POINT('Ctrl Pts',(43.2708954640494,0.243759038204317,9.1612330567983));
#37301=CARTESIAN_POINT('Ctrl Pts',(40.6868518840738,0.21967725703067,5.62616928052599));
#37302=CARTESIAN_POINT('Ctrl Pts',(37.633788218554,0.192114722189047,2.54682342316403));
#37303=CARTESIAN_POINT('Ctrl Pts',(34.243942068342,0.154437491851918,-0.135833115208792));
#37304=CARTESIAN_POINT('Ctrl Pts',(30.4812454080981,0.0954817696064694,
-2.28260255543497));
#37305=CARTESIAN_POINT('Ctrl Pts',(26.4180719635485,0.0048363712043943,
-3.83383662526902));
#37306=CARTESIAN_POINT('Ctrl Pts',(22.7624168656732,-0.0979118428630517,
-4.72798729865453));
#37307=CARTESIAN_POINT('Ctrl Pts',(20.2320685893873,-0.184631554593919,
-5.01574202177787));
#37308=CARTESIAN_POINT('Ctrl Pts',(18.5418851689888,-0.247909792323189,
-5.09781715603392));
#37309=CARTESIAN_POINT('Ctrl Pts',(18.1357069004105,-0.263520166061751,
-5.10923666301494));
#37310=CARTESIAN_POINT('Ctrl Pts',(17.7307374709918,-0.279478515480188,
-5.11242798885562));
#37311=CARTESIAN_POINT('Ctrl Pts',(45.7213662087155,3.93922736422659,24.1716806442701));
#37312=CARTESIAN_POINT('Ctrl Pts',(45.688208426122,3.92273017306588,23.7676952109987));
#37313=CARTESIAN_POINT('Ctrl Pts',(45.6473827402039,3.90651491483579,23.3627796511822));
#37314=CARTESIAN_POINT('Ctrl Pts',(45.4405866009357,3.83888692720806,21.6367355343485));
#37315=CARTESIAN_POINT('Ctrl Pts',(44.9678249093539,3.74496038387833,19.0500710475274));
#37316=CARTESIAN_POINT('Ctrl Pts',(43.8199173057419,3.6271896762232,15.3604237886896));
#37317=CARTESIAN_POINT('Ctrl Pts',(42.0043881080348,3.50969140214063,11.3107097806898));
#37318=CARTESIAN_POINT('Ctrl Pts',(39.6381007942075,3.40771510315772,7.62053324398369));
#37319=CARTESIAN_POINT('Ctrl Pts',(36.7883508830545,3.30695483103527,4.35105340659633));
#37320=CARTESIAN_POINT('Ctrl Pts',(33.5879037474396,3.1998573133211,1.45057582162554));
#37321=CARTESIAN_POINT('Ctrl Pts',(29.9942635963678,3.07607789704229,-0.948197922906822));
#37322=CARTESIAN_POINT('Ctrl Pts',(26.075402425309,2.92448144596071,-2.7849461353621));
#37323=CARTESIAN_POINT('Ctrl Pts',(22.5244809527974,2.77158317941627,-3.9464844359537));
#37324=CARTESIAN_POINT('Ctrl Pts',(20.049992630345,2.65236568914073,-4.42739273892755));
#37325=CARTESIAN_POINT('Ctrl Pts',(18.3915748274528,2.56779645721963,-4.6415318716897));
#37326=CARTESIAN_POINT('Ctrl Pts',(17.9921830064857,2.54707902977605,-4.68497343012829));
#37327=CARTESIAN_POINT('Ctrl Pts',(17.5931404618472,2.52604544176493,-4.72036483483639));
#37328=CARTESIAN_POINT('Ctrl Pts',(43.2820442732254,7.64857049485316,27.1714239460178));
#37329=CARTESIAN_POINT('Ctrl Pts',(43.2727023403867,7.62538079009264,26.7633085649188));
#37330=CARTESIAN_POINT('Ctrl Pts',(43.2558781734963,7.6024320797305,26.353789632655));
#37331=CARTESIAN_POINT('Ctrl Pts',(43.1519567273492,7.50598047950645,24.6060794051385));
#37332=CARTESIAN_POINT('Ctrl Pts',(42.8361624278849,7.36825978906471,21.9768147066715));
#37333=CARTESIAN_POINT('Ctrl Pts',(41.9201606521025,7.18657585481396,18.195120286621));
#37334=CARTESIAN_POINT('Ctrl Pts',(40.3683770686699,6.99739878870591,14.0054622248624));
#37335=CARTESIAN_POINT('Ctrl Pts',(38.2539595021366,6.82819742189185,10.1350305421312));
#37336=CARTESIAN_POINT('Ctrl Pts',(35.6391340409848,6.66543158101024,6.64562945258854));
#37337=CARTESIAN_POINT('Ctrl Pts',(32.6573475458408,6.50060855796851,3.49387433273689));
#37338=CARTESIAN_POINT('Ctrl Pts',(29.2586568556057,6.32441606849526,0.805112441394477));
#37339=CARTESIAN_POINT('Ctrl Pts',(25.5059908438053,6.12505774886043,-1.35957124492499));
#37340=CARTESIAN_POINT('Ctrl Pts',(22.075521138649,5.93384517916791,-2.82786038740783));
#37341=CARTESIAN_POINT('Ctrl Pts',(19.6651555950876,5.79035915091665,-3.53013920906786));
#37342=CARTESIAN_POINT('Ctrl Pts',(18.0431548018333,5.69001969995687,-3.89557055616166));
#37343=CARTESIAN_POINT('Ctrl Pts',(17.6516126072861,5.66551509710643,-3.97576378962003));
#37344=CARTESIAN_POINT('Ctrl Pts',(17.2594995078076,5.64071489355821,-4.04817830458482));
#37345=CARTESIAN_POINT('Ctrl Pts',(40.985186418,10.6050661536892,29.9982594338762));
#37346=CARTESIAN_POINT('Ctrl Pts',(40.9969328308233,10.5777689837161,29.5862652996575));
#37347=CARTESIAN_POINT('Ctrl Pts',(41.0013571377618,10.5506896266998,29.1724780443182));
#37348=CARTESIAN_POINT('Ctrl Pts',(40.9884998486727,10.4365567481294,27.404896453078));
#37349=CARTESIAN_POINT('Ctrl Pts',(40.8115942540796,10.2719415070743,24.7370183562784));
#37350=CARTESIAN_POINT('Ctrl Pts',(40.1006192580091,10.0511774947007,20.8729636138941));
#37351=CARTESIAN_POINT('Ctrl Pts',(38.7818181838249,9.81863871620139,16.5589607680871));
#37352=CARTESIAN_POINT('Ctrl Pts',(36.8896525789635,9.60967367489776,12.5292063966697));
#37353=CARTESIAN_POINT('Ctrl Pts',(34.4818871352799,9.41153176383594,8.84607749903719));
#37354=CARTESIAN_POINT('Ctrl Pts',(31.6926260287593,9.21500541081661,5.47340241149087));
#37355=CARTESIAN_POINT('Ctrl Pts',(28.4653194124203,9.01175979868378,2.53015669942969));
#37356=CARTESIAN_POINT('Ctrl Pts',(24.8584646940975,8.78956564702969,0.0780936876946292));
#37357=CARTESIAN_POINT('Ctrl Pts',(21.5334346929017,8.58124477590158,-1.6587653846784));
#37358=CARTESIAN_POINT('Ctrl Pts',(19.1790085003012,8.42762540105217,-2.55471275350617));
#37359=CARTESIAN_POINT('Ctrl Pts',(17.5886957847182,8.32086564673385,-3.05245934568359));
#37360=CARTESIAN_POINT('Ctrl Pts',(17.2040547252269,8.29482075310626,-3.16483640809568));
#37361=CARTESIAN_POINT('Ctrl Pts',(16.8181095137966,8.26849188852043,-3.26971525901482));
#37362=CARTESIAN_POINT('Ctrl Pts',(38.1960047398292,13.6252616883324,33.4321039804979));
#37363=CARTESIAN_POINT('Ctrl Pts',(38.2320179600167,13.5952855444977,33.0155280106869));
#37364=CARTESIAN_POINT('Ctrl Pts',(38.2608843008179,13.5655149131873,32.596745525132));
#37365=CARTESIAN_POINT('Ctrl Pts',(38.3527474093692,13.4398628522405,30.8060971867503));
#37366=CARTESIAN_POINT('Ctrl Pts',(38.3355056499632,13.2576618204372,28.0936014929509));
#37367=CARTESIAN_POINT('Ctrl Pts',(37.860056066436,13.0115743729063,24.1348762335303));
#37368=CARTESIAN_POINT('Ctrl Pts',(36.8086829471625,12.751644575675,19.6783627939692));
#37369=CARTESIAN_POINT('Ctrl Pts',(35.171342701358,12.5189796899122,15.4664292044507));
#37370=CARTESIAN_POINT('Ctrl Pts',(33.0006620268248,12.301865256328,11.5621247517028));
#37371=CARTESIAN_POINT('Ctrl Pts',(30.4315525548981,12.0904144587841,7.93746377529417));
#37372=CARTESIAN_POINT('Ctrl Pts',(27.3998095635454,11.8774764455751,4.70421501534603));
#37373=CARTESIAN_POINT('Ctrl Pts',(23.9588320023988,11.6504923923572,1.92490607313789));
#37374=CARTESIAN_POINT('Ctrl Pts',(20.7533189738236,11.4410171343385,-0.117626788490311));
#37375=CARTESIAN_POINT('Ctrl Pts',(18.461936909906,11.2882220371981,-1.23390159894501));
#37376=CARTESIAN_POINT('Ctrl Pts',(16.907176814582,11.1823584691134,-1.88214643141196));
#37377=CARTESIAN_POINT('Ctrl Pts',(16.5303633666016,11.1565388193505,-2.03115178324461));
#37378=CARTESIAN_POINT('Ctrl Pts',(16.1515047029193,11.1304479812224,-2.17300196454322));
#37379=CARTESIAN_POINT('Ctrl Pts',(35.6250369117929,15.9398275064074,36.5973462848406));
#37380=CARTESIAN_POINT('Ctrl Pts',(35.6823628409769,15.9092719019138,36.176722702768));
#37381=CARTESIAN_POINT('Ctrl Pts',(35.7326842526493,15.8789225535602,35.7535587401085));
#37382=CARTESIAN_POINT('Ctrl Pts',(35.9164273802557,15.7507918597713,33.9428065182253));
#37383=CARTESIAN_POINT('Ctrl Pts',(36.0392336977157,15.5646999212503,31.191436002328));
#37384=CARTESIAN_POINT('Ctrl Pts',(35.7702402889224,15.3133344724918,27.15026887435));
#37385=CARTESIAN_POINT('Ctrl Pts',(34.9531102563103,15.0487502016962,22.5697046993983));
#37386=CARTESIAN_POINT('Ctrl Pts',(33.5387202772831,14.8142492774957,18.1992580018583));
#37387=CARTESIAN_POINT('Ctrl Pts',(31.5751615684769,14.5991383033468,14.1025862551498));
#37388=CARTESIAN_POINT('Ctrl Pts',(29.1980931926873,14.3930646018661,10.2588220611129));
#37389=CARTESIAN_POINT('Ctrl Pts',(26.3365213630746,14.1899609567462,6.77349474422793));
#37390=CARTESIAN_POINT('Ctrl Pts',(23.0393473535078,13.977122935371,3.70982406676064));
#37391=CARTESIAN_POINT('Ctrl Pts',(19.9369788908936,13.7824369346935,1.40173743650218));
#37392=CARTESIAN_POINT('Ctrl Pts',(17.6996045937325,13.6409944051188,0.0940973017916472));
#37393=CARTESIAN_POINT('Ctrl Pts',(16.175122288904,13.5429643472183,-0.684847627751295));
#37394=CARTESIAN_POINT('Ctrl Pts',(15.8050468938553,13.5190447294408,-0.865658102920624));
#37395=CARTESIAN_POINT('Ctrl Pts',(15.4323648377265,13.4948677704672,-1.0396092374574));
#37396=CARTESIAN_POINT('Ctrl Pts',(32.5619623291767,18.188947172369,40.3670019380271));
#37397=CARTESIAN_POINT('Ctrl Pts',(32.6436186340454,18.1597316481657,39.9418646159408));
#37398=CARTESIAN_POINT('Ctrl Pts',(32.7184160259125,18.1307342364494,39.5138369066759));
#37399=CARTESIAN_POINT('Ctrl Pts',(33.0069098816923,18.0083786966032,37.6808619105327));
#37400=CARTESIAN_POINT('Ctrl Pts',(33.2893521670055,17.830846834045,34.8862535762931));
#37401=CARTESIAN_POINT('Ctrl Pts',(33.2555646360601,17.5925027676131,30.7527878233976));
#37402=CARTESIAN_POINT('Ctrl Pts',(32.7051064889568,17.3443426911773,26.0328695343581));
#37403=CARTESIAN_POINT('Ctrl Pts',(31.5442365963815,17.1289494695207,21.4839276053616));
#37404=CARTESIAN_POINT('Ctrl Pts',(29.8158089418295,16.9369213116231,17.1703445361495));
#37405=CARTESIAN_POINT('Ctrl Pts',(27.6563687494004,16.7575317657622,13.0793476612587));
#37406=CARTESIAN_POINT('Ctrl Pts',(24.9870614584278,16.5859876106103,9.30941171936927));
#37407=CARTESIAN_POINT('Ctrl Pts',(21.8515956138191,16.4095763329362,5.92457317984241));
#37408=CARTESIAN_POINT('Ctrl Pts',(18.8645313333366,16.2491906636996,3.31651020420802));
#37409=CARTESIAN_POINT('Ctrl Pts',(16.6869382415737,16.1323920433636,1.79267841142363));
#37410=CARTESIAN_POINT('Ctrl Pts',(15.1957006142707,16.0510402241362,0.866074551347136));
#37411=CARTESIAN_POINT('Ctrl Pts',(14.8330943827188,16.0311583490605,0.649363554666546));
#37412=CARTESIAN_POINT('Ctrl Pts',(14.4673343468776,16.01103806515,0.43920571884));
#37413=CARTESIAN_POINT('Ctrl Pts',(29.7866051558503,19.7983627848149,43.7804409554261));
#37414=CARTESIAN_POINT('Ctrl Pts',(29.889459148105,19.7720645135703,43.3515471357187));
#37415=CARTESIAN_POINT('Ctrl Pts',(29.9855637697716,19.7460021313493,42.9194818145262));
#37416=CARTESIAN_POINT('Ctrl Pts',(30.3651772634003,19.6361820466171,41.0681036249458));
#37417=CARTESIAN_POINT('Ctrl Pts',(30.7864638771974,19.4774394485581,38.2372822629002));
#37418=CARTESIAN_POINT('Ctrl Pts',(30.9571529902603,19.2670183310104,34.025583050656));
#37419=CARTESIAN_POINT('Ctrl Pts',(30.6383680494902,19.0520629838802,29.1868126511722));
#37420=CARTESIAN_POINT('Ctrl Pts',(29.697484286248,18.8717166252608,24.4849595349987));
#37421=CARTESIAN_POINT('Ctrl Pts',(28.1727214392882,18.7178122962125,19.9850708127111));
#37422=CARTESIAN_POINT('Ctrl Pts',(26.2014191897252,18.5794411422907,15.6814277247905));
#37423=CARTESIAN_POINT('Ctrl Pts',(23.6977578050179,18.4529446490623,11.6663983296305));
#37424=CARTESIAN_POINT('Ctrl Pts',(20.7008504579983,18.3257380682571,8.00476104675949));
#37425=CARTESIAN_POINT('Ctrl Pts',(17.8118961304768,18.2102139945187,5.13804607190731));
#37426=CARTESIAN_POINT('Ctrl Pts',(15.6845649626298,18.1249152482566,3.42774500705276));
#37427=CARTESIAN_POINT('Ctrl Pts',(14.2209995873091,18.064727637235,2.37376826844734));
#37428=CARTESIAN_POINT('Ctrl Pts',(13.8646592739966,18.0499634327475,2.12613341463877));
#37429=CARTESIAN_POINT('Ctrl Pts',(13.5047578340977,18.0349776243875,1.88482906425678));
#37430=CARTESIAN_POINT('Ctrl Pts',(27.7526639506774,20.6836496418694,46.2795822977866));
#37431=CARTESIAN_POINT('Ctrl Pts',(27.8705165233211,20.6606519170286,45.8482413413726));
#37432=CARTESIAN_POINT('Ctrl Pts',(27.9816862133389,20.6379063239872,45.4135423099364));
#37433=CARTESIAN_POINT('Ctrl Pts',(28.4256799254442,20.5422448076096,43.5501481782092));
#37434=CARTESIAN_POINT('Ctrl Pts',(28.9450621552993,20.4047755971079,40.6951986457009));
#37435=CARTESIAN_POINT('Ctrl Pts',(29.2601668709738,20.225761668211,36.430272862676));
#37436=CARTESIAN_POINT('Ctrl Pts',(29.104902952896,20.0475517349526,31.5097756876155));
#37437=CARTESIAN_POINT('Ctrl Pts',(28.3191048348243,19.9048724048602,26.7019746382763));
#37438=CARTESIAN_POINT('Ctrl Pts',(26.9376410290806,19.790507905872,22.0724169164535));
#37439=CARTESIAN_POINT('Ctrl Pts',(25.0984225618106,19.6935273080542,17.6204087054907));
#37440=CARTESIAN_POINT('Ctrl Pts',(22.7105958915495,19.6110850660289,13.4340017986264));
#37441=CARTESIAN_POINT('Ctrl Pts',(19.8099493704634,19.530779076001,9.57852885042505));
#37442=CARTESIAN_POINT('Ctrl Pts',(16.9885762929046,19.4573327991495,6.53052694702122));
#37443=CARTESIAN_POINT('Ctrl Pts',(14.8953515136484,19.4012238336331,4.68944489777427));
#37444=CARTESIAN_POINT('Ctrl Pts',(13.4503222706086,19.3605693891818,3.54611204363267));
#37445=CARTESIAN_POINT('Ctrl Pts',(13.0981976310342,19.3505226070412,3.27681676297094));
#37446=CARTESIAN_POINT('Ctrl Pts',(12.7422574691309,19.3402634731691,3.01372770483773));
#37447=CARTESIAN_POINT('Ctrl Pts',(26.6080532394981,21.117312799858,47.6853113156483));
#37448=CARTESIAN_POINT('Ctrl Pts',(26.7342384178453,21.0964267127388,47.2526690936168));
#37449=CARTESIAN_POINT('Ctrl Pts',(26.8537736232549,21.0758020890032,46.8165686819745));
#37450=CARTESIAN_POINT('Ctrl Pts',(27.3335005166717,20.9891913310095,44.9467780571391));
#37451=CARTESIAN_POINT('Ctrl Pts',(27.9073295027061,20.8653273744228,42.0788365144294));
#37452=CARTESIAN_POINT('Ctrl Pts',(28.3025817120245,20.7063681300896,37.784920215597));
#37453=CARTESIAN_POINT('Ctrl Pts',(28.2380468618629,20.5515335415639,32.8196546797573));
#37454=CARTESIAN_POINT('Ctrl Pts',(27.5382555433897,20.4326519806542,27.9535830792282));
#37455=CARTESIAN_POINT('Ctrl Pts',(26.2361957108526,20.3430531321453,23.252537996115));
#37456=CARTESIAN_POINT('Ctrl Pts',(24.4700967317106,20.2718184169426,18.7186288699449));
#37457=CARTESIAN_POINT('Ctrl Pts',(22.1462824761541,20.2165549432469,14.4375077942308));
#37458=CARTESIAN_POINT('Ctrl Pts',(19.2986750354573,20.164982094833,10.4748228833348));
#37459=CARTESIAN_POINT('Ctrl Pts',(16.5143939304978,20.117197691553,7.32650190177016));
#37460=CARTESIAN_POINT('Ctrl Pts',(14.4397578973729,20.0788282397779,5.41302288571427));
#37461=CARTESIAN_POINT('Ctrl Pts',(13.0047690687654,20.0500302875854,4.22021769274083));
#37462=CARTESIAN_POINT('Ctrl Pts',(12.6549332160082,20.0428451797642,3.93894201614119));
#37463=CARTESIAN_POINT('Ctrl Pts',(12.3011493997076,20.0354515632684,3.66381517387371));
#37464=CARTESIAN_POINT('Ctrl Pts',(26.2824873057561,21.2334813897109,48.0850725526183));
#37465=CARTESIAN_POINT('Ctrl Pts',(26.4110343322392,21.2132228077857,47.6520643827852));
#37466=CARTESIAN_POINT('Ctrl Pts',(26.5329401420435,21.1932283095702,47.2155698874215));
#37467=CARTESIAN_POINT('Ctrl Pts',(27.022790635021,21.1093059289188,45.3439807507387));
#37468=CARTESIAN_POINT('Ctrl Pts',(27.6120426416372,20.9894835119608,42.4723801622684));
#37469=CARTESIAN_POINT('Ctrl Pts',(28.0299894261123,20.8364792943525,38.1702892347921));
#37470=CARTESIAN_POINT('Ctrl Pts',(27.991132522269,20.6885792302246,33.1923965419472));
#37471=CARTESIAN_POINT('Ctrl Pts',(27.3156638017101,20.5767478260626,28.3098930006326));
#37472=CARTESIAN_POINT('Ctrl Pts',(26.0360362828936,20.4944756050622,23.5886985169737));
#37473=CARTESIAN_POINT('Ctrl Pts',(24.2905703227061,20.4308554028779,19.0317189717236));
#37474=CARTESIAN_POINT('Ctrl Pts',(21.9847846102783,20.3836340081555,14.7239348286272));
#37475=CARTESIAN_POINT('Ctrl Pts',(19.1520689743563,20.340580727313,10.7310827937134));
#37476=CARTESIAN_POINT('Ctrl Pts',(16.3781561160741,20.3004356869138,7.55454097932343));
#37477=CARTESIAN_POINT('Ctrl Pts',(14.3086760657568,20.2673681898868,5.62069087823361));
#37478=CARTESIAN_POINT('Ctrl Pts',(12.8764521475924,20.2421246596599,4.41396068576133));
#37479=CARTESIAN_POINT('Ctrl Pts',(12.5272471452757,20.2357981340653,4.12931503535631));
#37480=CARTESIAN_POINT('Ctrl Pts',(12.1740582093971,20.2292648564311,3.85080413039918));
#37481=CARTESIAN_POINT('Ctrl Pts',(25.9559446728124,21.3428689572265,48.4859646953694));
#37482=CARTESIAN_POINT('Ctrl Pts',(26.0868514733104,21.323266505305,48.0525937135402));
#37483=CARTESIAN_POINT('Ctrl Pts',(26.2111255193517,21.303930781031,47.6157083582835));
#37484=CARTESIAN_POINT('Ctrl Pts',(26.7110882848482,21.2228186866547,45.7423349337262));
#37485=CARTESIAN_POINT('Ctrl Pts',(27.3157439744971,21.1072213437662,42.8670987183852));
#37486=CARTESIAN_POINT('Ctrl Pts',(27.7563489980754,20.9604400919523,38.5568768250566));
#37487=CARTESIAN_POINT('Ctrl Pts',(27.7431168114943,20.819779963638,33.5664217702629));
#37488=CARTESIAN_POINT('Ctrl Pts',(27.0919024222535,20.7152993064879,28.6675748991354));
#37489=CARTESIAN_POINT('Ctrl Pts',(25.8346222954885,20.6406553883908,23.9263498379602));
#37490=CARTESIAN_POINT('Ctrl Pts',(24.1096882069938,20.5849601975755,19.3464505651354));
#37491=CARTESIAN_POINT('Ctrl Pts',(21.8218093008398,20.5461109852346,15.0121949824723));
#37492=CARTESIAN_POINT('Ctrl Pts',(19.0038402671502,20.5119420676311,10.9894081969158));
#37493=CARTESIAN_POINT('Ctrl Pts',(16.2401496479356,20.4797911688045,7.78487143238121));
#37494=CARTESIAN_POINT('Ctrl Pts',(14.1757138007688,20.4522911786996,5.83080964155293));
#37495=CARTESIAN_POINT('Ctrl Pts',(12.7461750731845,20.4307901345004,4.6102596399058));
#37496=CARTESIAN_POINT('Ctrl Pts',(12.3975828398805,20.4253683033402,4.3222709374315));
#37497=CARTESIAN_POINT('Ctrl Pts',(12.0449717795587,20.4197421663948,4.04040440327869));
#37498=CARTESIAN_POINT('',(28.5350439006909,20.5529756002067,37.188944948637));
#37499=CARTESIAN_POINT('Ctrl Pts',(45.8340192197807,-3.27137127985418,9.82390328601451));
#37500=CARTESIAN_POINT('Ctrl Pts',(44.9697966722668,1.76302065361956,13.855987239011));
#37501=CARTESIAN_POINT('Ctrl Pts',(43.3148043132766,6.26298702225421,18.861450934027));
#37502=CARTESIAN_POINT('Ctrl Pts',(38.8444439114925,12.5188402724798,26.3935858075399));
#37503=CARTESIAN_POINT('Ctrl Pts',(37.0863575215197,14.4577038717082,28.8308190938515));
#37504=CARTESIAN_POINT('Ctrl Pts',(33.151540262371,17.848637426394,33.2637736993417));
#37505=CARTESIAN_POINT('Ctrl Pts',(30.9674108740526,19.3555632898772,35.3225922516136));
#37506=CARTESIAN_POINT('Ctrl Pts',(28.5350439006906,20.5529756002057,37.1889449486372));
#37507=CARTESIAN_POINT('Ctrl Pts',(18.4983482597372,19.9464420456703,9.15631398661356));
#37508=CARTESIAN_POINT('Ctrl Pts',(21.8233107194045,20.0189549105364,12.9978580624312));
#37509=CARTESIAN_POINT('Ctrl Pts',(24.3992471837434,20.0954766247834,17.4724801790673));
#37510=CARTESIAN_POINT('Ctrl Pts',(27.8197485288317,20.2752040736289,27.033257475201));
#37511=CARTESIAN_POINT('Ctrl Pts',(28.6662063188346,20.3824974081049,32.1189996344999));
#37512=CARTESIAN_POINT('Ctrl Pts',(28.5350439006908,20.5529756002056,37.188944948637));
#37513=CARTESIAN_POINT('Ctrl Pts',(27.1639503240327,20.9435908393615,46.4304062506873));
#37514=CARTESIAN_POINT('Ctrl Pts',(27.2038388093363,20.9358615047579,46.2802752340366));
#37515=CARTESIAN_POINT('Ctrl Pts',(27.2437272946399,20.9281321701544,46.1301442173858));
#37516=CARTESIAN_POINT('Ctrl Pts',(27.2836157799436,20.9204028355509,45.980013200735));
#37517=CARTESIAN_POINT('Ctrl Pts',(31.2724643103077,20.1474693751975,30.9669115356589));
#37518=CARTESIAN_POINT('Ctrl Pts',(25.5907014765415,20.0812550388979,14.0171226984615));
#37519=CARTESIAN_POINT('Ctrl Pts',(13.4755336335094,19.8399463130827,4.31382061658607));
#37520=CARTESIAN_POINT('Ctrl Pts',(27.1640149500145,20.9469886892296,46.4303364767158));
#37521=CARTESIAN_POINT('Ctrl Pts',(27.203911504098,20.9392720585054,46.2802053778394));
#37522=CARTESIAN_POINT('Ctrl Pts',(27.2438080581816,20.9315554277811,46.130074278963));
#37523=CARTESIAN_POINT('Ctrl Pts',(27.2837046122652,20.9238387970569,45.9799431800866));
#37524=CARTESIAN_POINT('Ctrl Pts',(31.2733600206231,20.1521757246323,30.9668332924482));
#37525=CARTESIAN_POINT('Ctrl Pts',(25.5911393772508,20.0873688943554,14.0170271739793));
#37526=CARTESIAN_POINT('Ctrl Pts',(13.4761812282898,19.8474084919615,4.31358578508753));
#37527=CARTESIAN_POINT('Ctrl Pts',(27.1640795759962,20.9503865390978,46.4302667027442));
#37528=CARTESIAN_POINT('Ctrl Pts',(27.2039841988597,20.9426826122528,46.2801355216422));
#37529=CARTESIAN_POINT('Ctrl Pts',(27.2438888217233,20.9349786854078,46.1300043405402));
#37530=CARTESIAN_POINT('Ctrl Pts',(27.2837934445868,20.9272747585629,45.9798731594382));
#37531=CARTESIAN_POINT('Ctrl Pts',(31.2742557309385,20.1568820740671,30.9667550492374));
#37532=CARTESIAN_POINT('Ctrl Pts',(25.5915772779602,20.093482749813,14.016931649497));
#37533=CARTESIAN_POINT('Ctrl Pts',(13.4768288230703,19.8548706708402,4.31335095358899));
#37534=CARTESIAN_POINT('Ctrl Pts',(27.164144201978,20.9537843889659,46.4301969287727));
#37535=CARTESIAN_POINT('Ctrl Pts',(27.2040568936215,20.9460931660003,46.2800656654451));
#37536=CARTESIAN_POINT('Ctrl Pts',(27.2439695852649,20.9384019430346,46.1299344021174));
#37537=CARTESIAN_POINT('Ctrl Pts',(27.2838822769084,20.9307107200689,45.9798031387898));
#37538=CARTESIAN_POINT('Ctrl Pts',(31.2751514412539,20.1615884235019,30.9666768060267));
#37539=CARTESIAN_POINT('Ctrl Pts',(25.5920151786696,20.0995966052706,14.0168361250147));
#37540=CARTESIAN_POINT('Ctrl Pts',(13.4774764178507,19.862332849719,4.31311612209045));
#37541=CARTESIAN_POINT('Ctrl Pts',(27.1643404540439,20.9641027630587,46.4299850436194));
#37542=CARTESIAN_POINT('Ctrl Pts',(27.2042776484444,20.9564501184246,46.2798535305942));
#37543=CARTESIAN_POINT('Ctrl Pts',(27.244214842845,20.9487974737906,46.129722017569));
#37544=CARTESIAN_POINT('Ctrl Pts',(27.2841520372455,20.9411448291565,45.9795905045439));
#37545=CARTESIAN_POINT('Ctrl Pts',(31.2778714772977,20.1758803657488,30.9664392020272));
#37546=CARTESIAN_POINT('Ctrl Pts',(25.5933449676568,20.1181627721728,14.0165460423503));
#37547=CARTESIAN_POINT('Ctrl Pts',(13.4794429924389,19.8849935193208,4.31240300075057));
#37548=CARTESIAN_POINT('Ctrl Pts',(27.1647329580989,20.9847395112521,46.4295612730399));
#37549=CARTESIAN_POINT('Ctrl Pts',(27.2047191580392,20.9771640232786,46.2794292607107));
#37550=CARTESIAN_POINT('Ctrl Pts',(27.2447053579794,20.9695885353052,46.1292972483814));
#37551=CARTESIAN_POINT('Ctrl Pts',(27.2846915579197,20.9620130473318,45.9791652360522));
#37552=CARTESIAN_POINT('Ctrl Pts',(31.2833115519458,20.2044642499886,30.9659640031278));
#37553=CARTESIAN_POINT('Ctrl Pts',(25.5960045460592,20.1552951062578,14.0159658718316));
#37554=CARTESIAN_POINT('Ctrl Pts',(13.4833761416152,19.9303148585245,4.31097675807076));
#37555=CARTESIAN_POINT('Ctrl Pts',(27.1653217095864,21.0156946339229,46.4289255987532));
#37556=CARTESIAN_POINT('Ctrl Pts',(27.2053814193679,21.0082348808134,46.278792843607));
#37557=CARTESIAN_POINT('Ctrl Pts',(27.2454411291495,21.000775127704,46.1286600884607));
#37558=CARTESIAN_POINT('Ctrl Pts',(27.285500838931,20.9933153745945,45.9785273333144));
#37559=CARTESIAN_POINT('Ctrl Pts',(31.2914718170848,20.2473400636495,30.9652518186868));
#37560=CARTESIAN_POINT('Ctrl Pts',(25.5999939466102,20.2109936225946,14.0150952948138));
#37561=CARTESIAN_POINT('Ctrl Pts',(13.4892758653797,19.9982968673298,4.30883739405111));
#37562=CARTESIAN_POINT('Ctrl Pts',(27.165910455003,21.0466497571015,46.4282899002481));
#37563=CARTESIAN_POINT('Ctrl Pts',(27.2060436766494,21.0393057386868,46.2781564103577));
#37564=CARTESIAN_POINT('Ctrl Pts',(27.2461768982959,21.0319617202721,46.1280229204672));
#37565=CARTESIAN_POINT('Ctrl Pts',(27.2863101199424,21.0246177018574,45.9778894305768));
#37566=CARTESIAN_POINT('Ctrl Pts',(31.2996322845879,20.2902158603888,30.9645404415346));
#37567=CARTESIAN_POINT('Ctrl Pts',(25.6039833885755,20.2666921589687,14.0142242928149));
#37568=CARTESIAN_POINT('Ctrl Pts',(13.4951755891442,20.0662788761352,4.30669803003142));
#37569=CARTESIAN_POINT('Ctrl Pts',(27.1663029488616,21.0672865061488,46.4278660890332));
#37570=CARTESIAN_POINT('Ctrl Pts',(27.2064851794466,21.0600196441101,46.2777321133838));
#37571=CARTESIAN_POINT('Ctrl Pts',(27.2466674100316,21.0527527820714,46.1275981377344));
#37572=CARTESIAN_POINT('Ctrl Pts',(27.2868496406165,21.0454859200326,45.977464162085));
#37573=CARTESIAN_POINT('Ctrl Pts',(31.3050726991135,20.3187997161584,30.9640665971437));
#37574=CARTESIAN_POINT('Ctrl Pts',(25.6066430363201,20.3038245267329,14.0136434086836));
#37575=CARTESIAN_POINT('Ctrl Pts',(13.4991087383205,20.1116002153389,4.30527178735164));
#37576=CARTESIAN_POINT('Ctrl Pts',(27.1664991957514,21.0776048806767,46.4276541832925));
#37577=CARTESIAN_POINT('Ctrl Pts',(27.2067059308188,21.0703765968246,46.277519964808));
#37578=CARTESIAN_POINT('Ctrl Pts',(27.2469126658862,21.0631483129724,46.1273857463236));
#37579=CARTESIAN_POINT('Ctrl Pts',(27.2871194009536,21.0559200291202,45.9772515278391));
#37580=CARTESIAN_POINT('Ctrl Pts',(31.3077929076951,20.3330916439037,30.9638296793928));
#37581=CARTESIAN_POINT('Ctrl Pts',(25.6079728602995,20.3223907107576,14.0133529639299));
#37582=CARTESIAN_POINT('Ctrl Pts',(13.5010753129087,20.1342608849406,4.30455866601175));
#37583=CARTESIAN_POINT('Ctrl Pts',(27.1665181061429,21.0785991614118,46.4276337640108));
#37584=CARTESIAN_POINT('Ctrl Pts',(27.2067272024674,21.0713745949617,46.2774995221267));
#37585=CARTESIAN_POINT('Ctrl Pts',(27.2469362987919,21.0641500285117,46.1273652802426));
#37586=CARTESIAN_POINT('Ctrl Pts',(27.2871453951164,21.0569254620617,45.9772310383585));
#37587=CARTESIAN_POINT('Ctrl Pts',(31.308055027565,20.3344688170607,30.9638068499487));
#37588=CARTESIAN_POINT('Ctrl Pts',(25.6081010024172,20.3241797521467,14.0133249766125));
#37589=CARTESIAN_POINT('Ctrl Pts',(13.5012648124487,20.1364444718193,4.30448994948977));
#37590=CARTESIAN_POINT('Ctrl Pts',(27.1665370165344,21.0795934421468,46.4276133447292));
#37591=CARTESIAN_POINT('Ctrl Pts',(27.2067484741159,21.0723725930989,46.2774790794455));
#37592=CARTESIAN_POINT('Ctrl Pts',(27.2469599316975,21.0651517440511,46.1273448141617));
#37593=CARTESIAN_POINT('Ctrl Pts',(27.287171389279,21.0579308950032,45.977210548878));
#37594=CARTESIAN_POINT('Ctrl Pts',(31.3083171474348,20.3358459902176,30.9637840205045));
#37595=CARTESIAN_POINT('Ctrl Pts',(25.608229144535,20.3259687935359,14.0132969892951));
#37596=CARTESIAN_POINT('Ctrl Pts',(13.5014543119888,20.1386280586979,4.3044212329678));
#37597=CARTESIAN_POINT('Ctrl Pts',(27.1665559269259,21.0805877228818,46.4275929254476));
#37598=CARTESIAN_POINT('Ctrl Pts',(27.2067697457645,21.0733705912361,46.2774586367642));
#37599=CARTESIAN_POINT('Ctrl Pts',(27.2469835646031,21.0661534595904,46.1273243480808));
#37600=CARTESIAN_POINT('Ctrl Pts',(27.2871973834418,21.0589363279447,45.9771900593974));
#37601=CARTESIAN_POINT('Ctrl Pts',(31.3085792673046,20.3372231633746,30.9637611910603));
#37602=CARTESIAN_POINT('Ctrl Pts',(25.6083572866527,20.327757834925,14.0132690019777));
#37603=CARTESIAN_POINT('Ctrl Pts',(13.5016438115288,20.1408116455766,4.30435251644582));
#37604=CARTESIAN_POINT('',(28.5350439006909,20.5529756002067,37.188944948637));
#37605=CARTESIAN_POINT('Origin',(7.5111559719605E-6,20.2903503023534,4.07573877568452E-6));
#37606=CARTESIAN_POINT('Origin',(7.5111559719605E-6,-3.14714969764662,4.07573877568452E-6));
#37607=CARTESIAN_POINT('Origin',(7.5111559719605E-6,21.2397676607012,4.07573877568452E-6));
#37608=CARTESIAN_POINT('Origin',(7.5111559719605E-6,21.2397676607012,4.07573877568452E-6));
#37609=CARTESIAN_POINT('Origin',(7.5111559719605E-6,21.2397676607012,4.07573877568452E-6));
#37610=CARTESIAN_POINT('Origin',(7.5111559719605E-6,21.2397676607012,4.07573877568452E-6));
#37611=CARTESIAN_POINT('Origin',(7.5111559719605E-6,21.2397676607012,4.07573877568452E-6));
#37612=CARTESIAN_POINT('Origin',(7.5111559719605E-6,21.2397676607012,4.07573877568452E-6));
#37613=CARTESIAN_POINT('Origin',(7.5111559719605E-6,15.6028503023534,4.07573877568452E-6));
#37614=CARTESIAN_POINT('Origin',(7.5111559719605E-6,13.1028503023534,4.07573877568452E-6));
#37615=CARTESIAN_POINT('Origin',(7.5111559719605E-6,15.6028503023534,4.07573877568452E-6));
#37616=CARTESIAN_POINT('',(36.2685409947933,38.2719360260717,-1.32653200043132));
#37617=CARTESIAN_POINT('',(36.3520594091432,32.4021811414129,-1.24409765091547));
#37618=UNCERTAINTY_MEASURE_WITH_UNIT(LENGTH_MEASURE(0.01),#37626,
'DISTANCE_ACCURACY_VALUE',
'Maximum model space distance between geometric entities at asserted c
onnectivities');
#37619=UNCERTAINTY_MEASURE_WITH_UNIT(LENGTH_MEASURE(0.01),#37626,
'DISTANCE_ACCURACY_VALUE',
'Maximum model space distance between geometric entities at asserted c
onnectivities');
#37620=UNCERTAINTY_MEASURE_WITH_UNIT(LENGTH_MEASURE(0.01),#37626,
'DISTANCE_ACCURACY_VALUE',
'Maximum model space distance between geometric entities at asserted c
onnectivities');
#37621=UNCERTAINTY_MEASURE_WITH_UNIT(LENGTH_MEASURE(0.01),#37626,
'DISTANCE_ACCURACY_VALUE',
'Maximum model space distance between geometric entities at asserted c
onnectivities');
#37622=(
GEOMETRIC_REPRESENTATION_CONTEXT(3)
GLOBAL_UNCERTAINTY_ASSIGNED_CONTEXT((#37618))
GLOBAL_UNIT_ASSIGNED_CONTEXT((#37626,#37628,#37629))
REPRESENTATION_CONTEXT('','3D')
);
#37623=(
GEOMETRIC_REPRESENTATION_CONTEXT(3)
GLOBAL_UNCERTAINTY_ASSIGNED_CONTEXT((#37619))
GLOBAL_UNIT_ASSIGNED_CONTEXT((#37626,#37628,#37629))
REPRESENTATION_CONTEXT('','3D')
);
#37624=(
GEOMETRIC_REPRESENTATION_CONTEXT(3)
GLOBAL_UNCERTAINTY_ASSIGNED_CONTEXT((#37620))
GLOBAL_UNIT_ASSIGNED_CONTEXT((#37626,#37628,#37629))
REPRESENTATION_CONTEXT('','3D')
);
#37625=(
GEOMETRIC_REPRESENTATION_CONTEXT(3)
GLOBAL_UNCERTAINTY_ASSIGNED_CONTEXT((#37621))
GLOBAL_UNIT_ASSIGNED_CONTEXT((#37626,#37628,#37629))
REPRESENTATION_CONTEXT('','3D')
);
#37626=(
LENGTH_UNIT()
NAMED_UNIT(*)
SI_UNIT(.MILLI.,.METRE.)
);
#37627=(
LENGTH_UNIT()
NAMED_UNIT(*)
SI_UNIT($,.METRE.)
);
#37628=(
NAMED_UNIT(*)
PLANE_ANGLE_UNIT()
SI_UNIT($,.RADIAN.)
);
#37629=(
NAMED_UNIT(*)
SI_UNIT($,.STERADIAN.)
SOLID_ANGLE_UNIT()
);
#37630=SHAPE_DEFINITION_REPRESENTATION(#37633,#37638);
#37631=SHAPE_DEFINITION_REPRESENTATION(#37634,#37639);
#37632=SHAPE_DEFINITION_REPRESENTATION(#37635,#37640);
#37633=PRODUCT_DEFINITION_SHAPE('',$,#37642);
#37634=PRODUCT_DEFINITION_SHAPE('',$,#37643);
#37635=PRODUCT_DEFINITION_SHAPE('',$,#37644);
#37636=PRODUCT_DEFINITION_SHAPE($,$,#17);
#37637=PRODUCT_DEFINITION_SHAPE($,$,#18);
#37638=SHAPE_REPRESENTATION('',(#11522,#12991,#12992),#37622);
#37639=SHAPE_REPRESENTATION('',(#11523),#37623);
#37640=SHAPE_REPRESENTATION('',(#12950),#37624);
#37641=PRODUCT_DEFINITION_CONTEXT('part definition',#37652,'design');
#37642=PRODUCT_DEFINITION('MAT-004','MAT-004',#37645,#37641);
#37643=PRODUCT_DEFINITION('Part 1 - Rim','Part 1 - Rim',#37646,#37641);
#37644=PRODUCT_DEFINITION('Part 2 - Fan','Part 2 - Fan',#37647,#37641);
#37645=PRODUCT_DEFINITION_FORMATION('',$,#37654);
#37646=PRODUCT_DEFINITION_FORMATION('',$,#37655);
#37647=PRODUCT_DEFINITION_FORMATION('',$,#37656);
#37648=PRODUCT_RELATED_PRODUCT_CATEGORY('MAT-004','MAT-004',(#37654));
#37649=PRODUCT_RELATED_PRODUCT_CATEGORY('Part 1 - Rim','Part 1 - Rim',(#37655));
#37650=PRODUCT_RELATED_PRODUCT_CATEGORY('Part 2 - Fan','Part 2 - Fan',(#37656));
#37651=APPLICATION_PROTOCOL_DEFINITION('international standard',
'automotive_design',2009,#37652);
#37652=APPLICATION_CONTEXT(
'Core Data for Automotive Mechanical Design Process');
#37653=PRODUCT_CONTEXT('part definition',#37652,'mechanical');
#37654=PRODUCT('MAT-004','MAT-004','STEP AP214',(#37653));
#37655=PRODUCT('Part 1 - Rim','Part 1 - Rim',$,(#37653));
#37656=PRODUCT('Part 2 - Fan','Part 2 - Fan',$,(#37653));
#37657=PRESENTATION_STYLE_ASSIGNMENT((#37660));
#37658=PRESENTATION_STYLE_ASSIGNMENT((#37661));
#37659=PRESENTATION_STYLE_ASSIGNMENT((#37662));
#37660=SURFACE_STYLE_USAGE(.BOTH.,#37663);
#37661=SURFACE_STYLE_USAGE(.BOTH.,#37664);
#37662=SURFACE_STYLE_USAGE(.BOTH.,#37665);
#37663=SURFACE_SIDE_STYLE('',(#37666));
#37664=SURFACE_SIDE_STYLE('',(#37667));
#37665=SURFACE_SIDE_STYLE('',(#37668));
#37666=SURFACE_STYLE_FILL_AREA(#37669);
#37667=SURFACE_STYLE_FILL_AREA(#37670);
#37668=SURFACE_STYLE_FILL_AREA(#37671);
#37669=FILL_AREA_STYLE('Steel - Satin',(#37672));
#37670=FILL_AREA_STYLE('Opaque(97,158,199)',(#37673));
#37671=FILL_AREA_STYLE('Opaque(61,176,222)',(#37674));
#37672=FILL_AREA_STYLE_COLOUR('Steel - Satin',#37675);
#37673=FILL_AREA_STYLE_COLOUR('Opaque(97,158,199)',#37676);
#37674=FILL_AREA_STYLE_COLOUR('Opaque(61,176,222)',#37677);
#37675=COLOUR_RGB('Steel - Satin',0.627450980392157,0.627450980392157,0.627450980392157);
#37676=COLOUR_RGB('Opaque(97,158,199)',0.380392156862745,0.619607843137255,
0.780392156862745);
#37677=COLOUR_RGB('Opaque(61,176,222)',0.23921568627451,0.690196078431373,
0.870588235294118);
ENDSEC;
END-ISO-10303-21;
